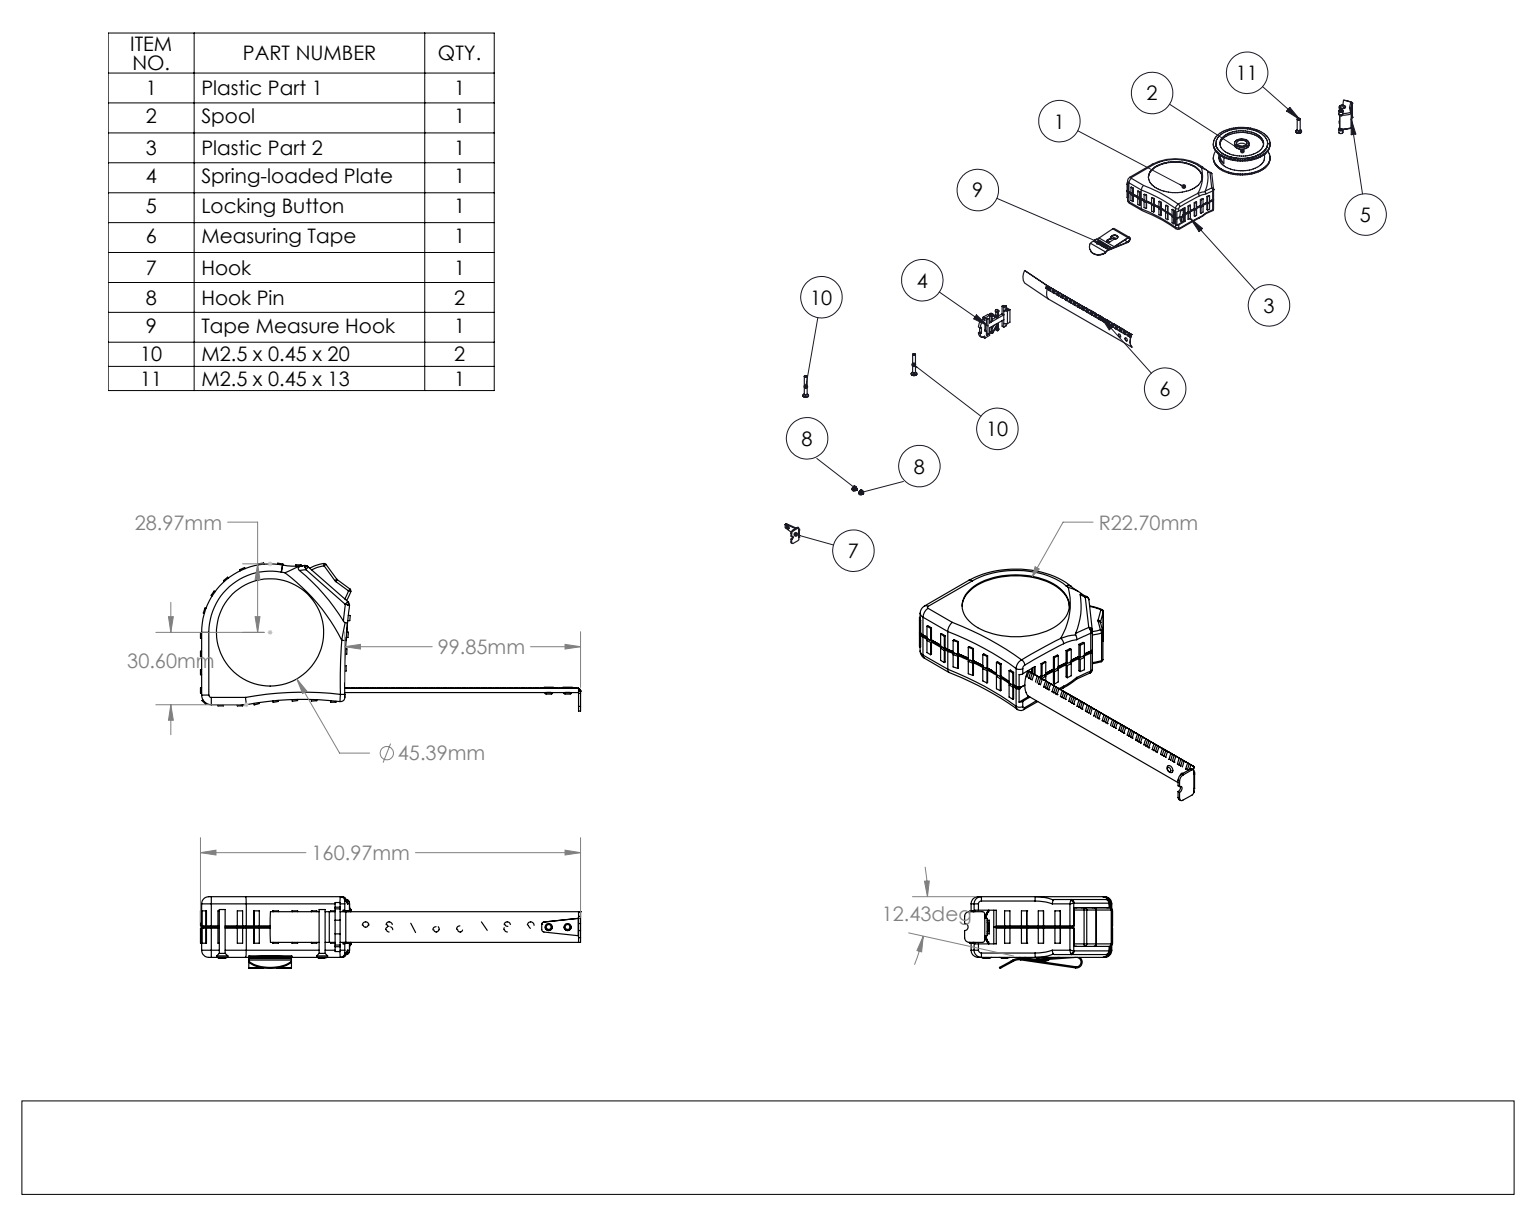
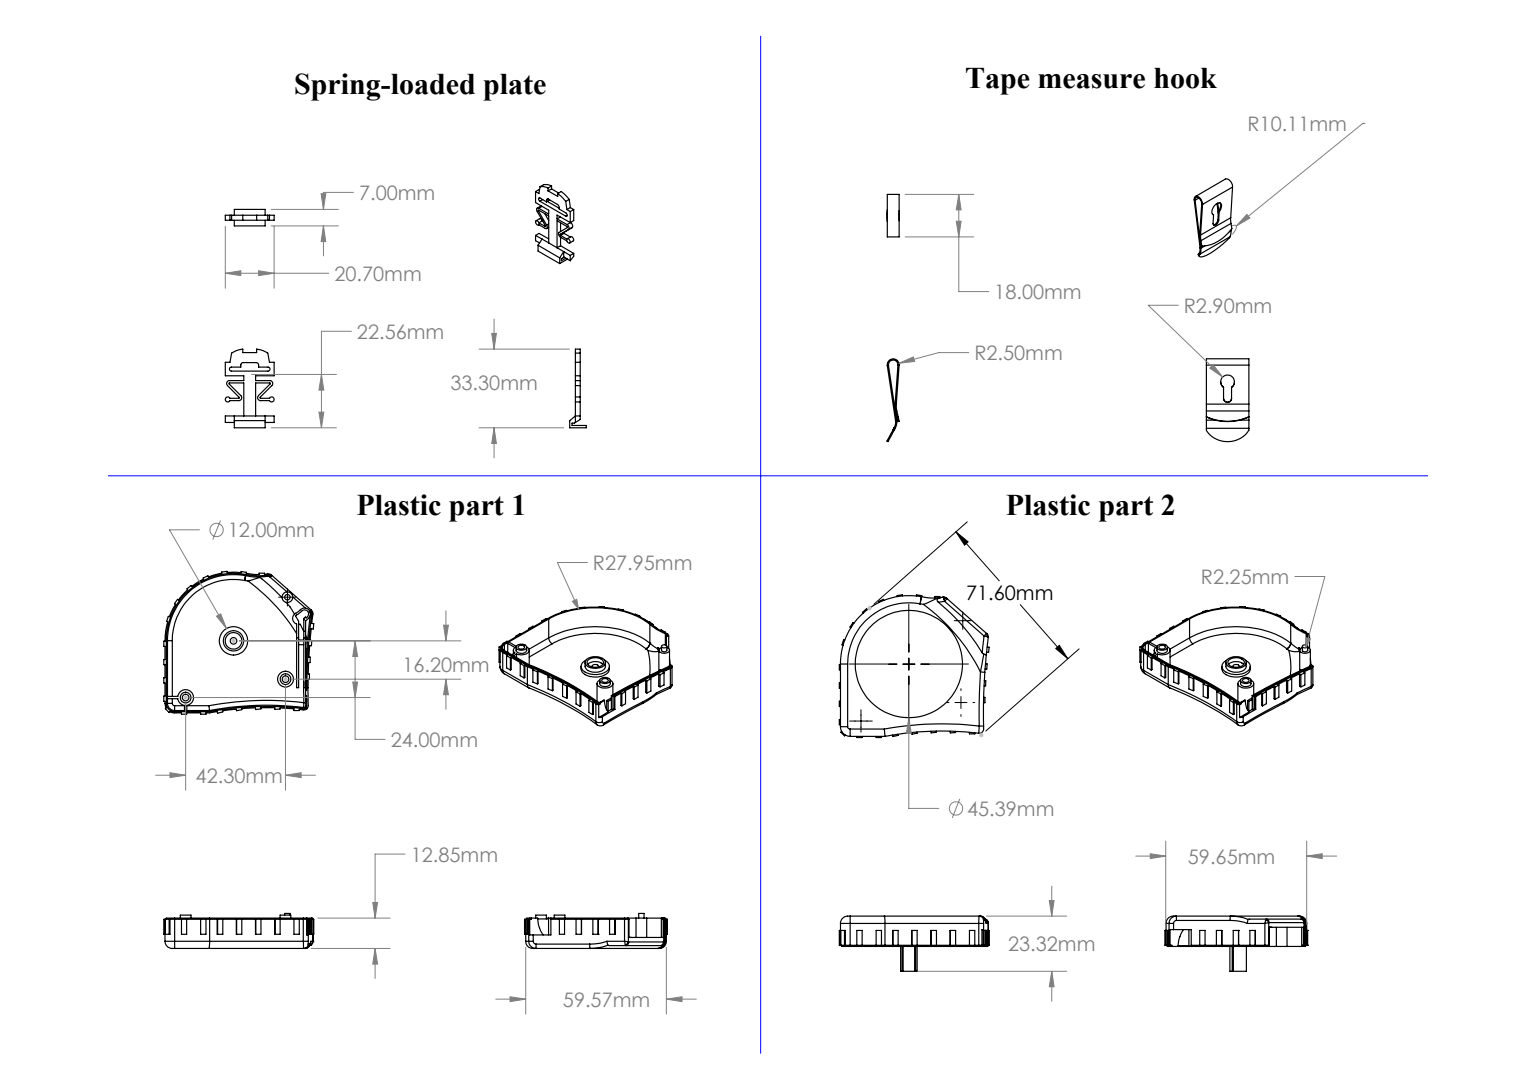
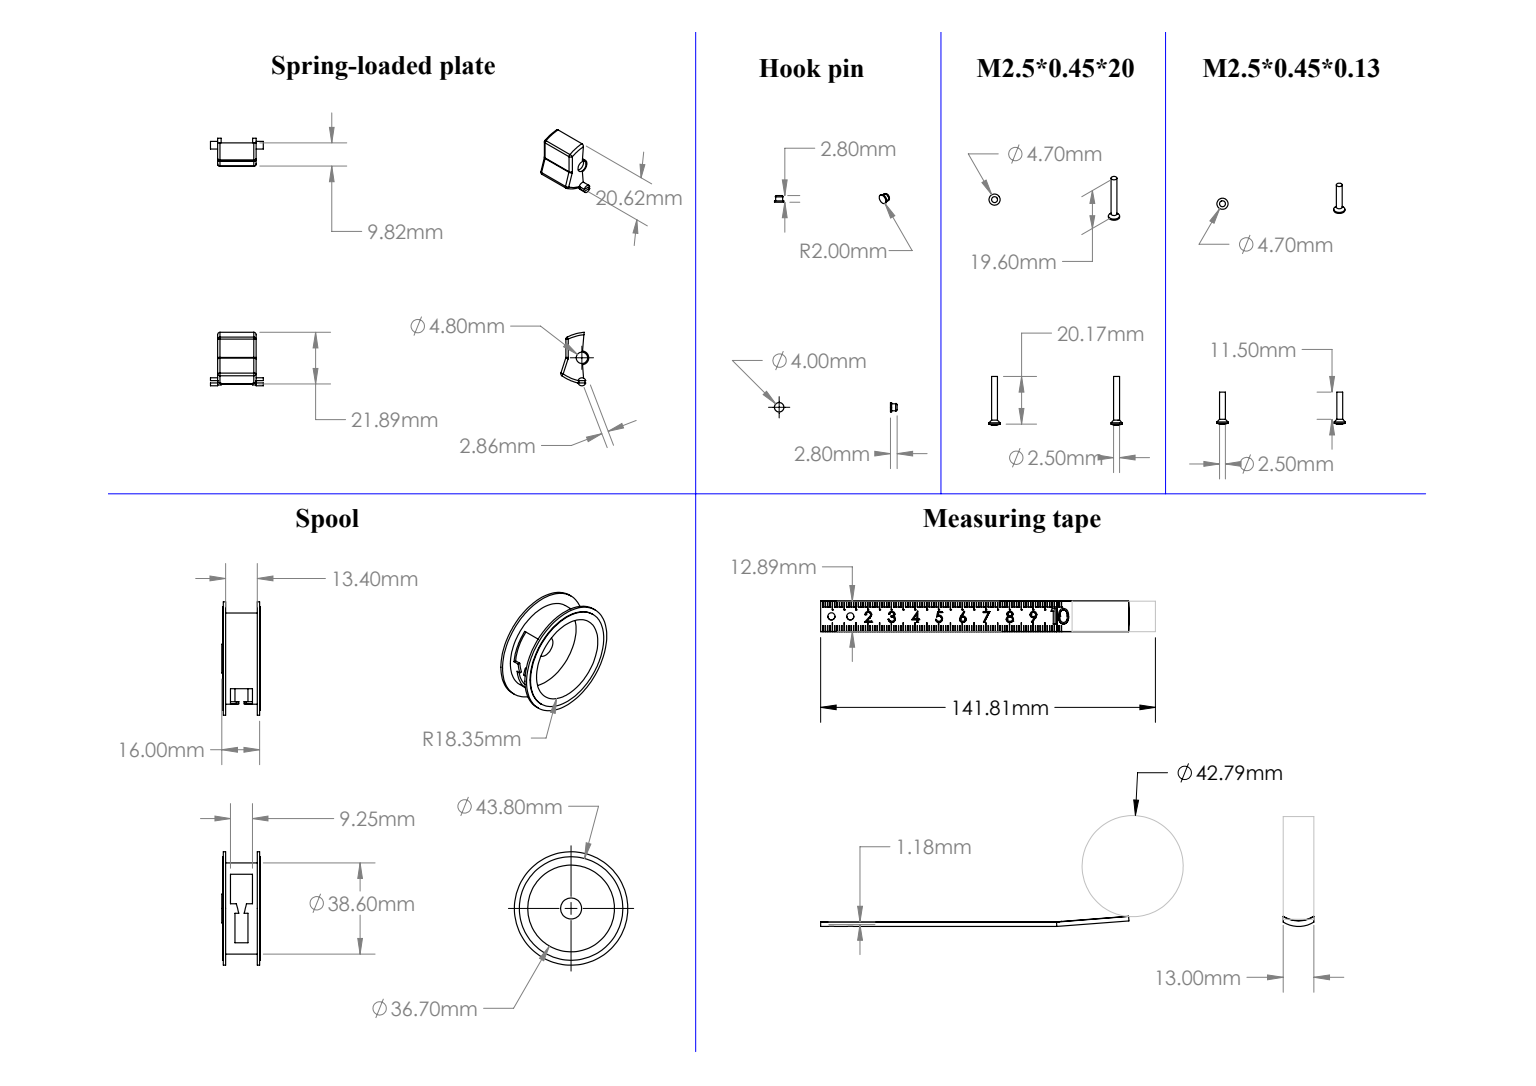
ISO-10303-21;
HEADER;
FILE_DESCRIPTION (('STEP AP203'),
    '1' );
FILE_NAME ('MAS-154',
    '2026-10-08T23:54:15',
    ( '' ),
    ( '' ),
    'SwSTEP 2.0',
    'SolidWorks 2024',
    '' );
FILE_SCHEMA (( 'AUTOMOTIVE_DESIGN' ));
ENDSEC;

DATA;
#1 = EDGE_LOOP ( 'NONE', ( #69285, #69519, #6373, #20333 ) ) ;
#2 = VECTOR ( 'NONE', #18887, 1000.000000000000000 ) ;
#3 = CARTESIAN_POINT ( 'NONE',  ( -28.32169924589829080, 0.3587747205143964613, -8.244178532169451401 ) ) ;
#4 = CARTESIAN_POINT ( 'NONE',  ( -80.94237186737068157, -25.14918324602283661, 7.008237357988867267 ) ) ;
#5 = EDGE_CURVE ( 'NONE', #2549, #11314, #80925, .T. ) ;
#6 = AXIS2_PLACEMENT_3D ( 'NONE', #5128, #50815, #66059 ) ;
#7 = CARTESIAN_POINT ( 'NONE',  ( -51.65200394065919909, -23.73791477778912196, 11.05961554403170766 ) ) ;
#9 = ORIENTED_EDGE ( 'NONE', *, *, #75672, .F. ) ;
#8 = CARTESIAN_POINT ( 'NONE',  ( 6.361473516681357410, -20.28576754457002451, 11.49999999999999645 ) ) ;
#10 = AXIS2_PLACEMENT_3D ( 'NONE', #33191, #48429, #34700 ) ;
#11 = EDGE_LOOP ( 'NONE', ( #61947, #2008, #96501, #28835 ) ) ;
#12 = CARTESIAN_POINT ( 'NONE',  ( -5.848988146064017180, 21.40304369876291446, 11.49999999999998934 ) ) ;
#13 = CARTESIAN_POINT ( 'NONE',  ( -4.704028875484805639, -20.06825252194306941, 11.49999999999998934 ) ) ;
#15 = ORIENTED_EDGE ( 'NONE', *, *, #21720, .F. ) ;
#14 = VECTOR ( 'NONE', #49997, 1000.000000000000000 ) ;
#16 = ORIENTED_EDGE ( 'NONE', *, *, #57693, .T. ) ;
#17 = DIRECTION ( 'NONE',  ( 1.000000000000000000, 3.773278334444166432E-23, 8.201307841325785021E-29 ) ) ;
#18 = CARTESIAN_POINT ( 'NONE',  ( -39.73355216781377663, -25.15155473006780795, 3.010709736661470348 ) ) ;
#19 = ORIENTED_EDGE ( 'NONE', *, *, #7474, .F. ) ;
#20 = CARTESIAN_POINT ( 'NONE',  ( -91.51201375565671015, -24.15543982623907482, -0.2315651400026614848 ) ) ;
#21 = VERTEX_POINT ( 'NONE', #59747 ) ;
#22 = CARTESIAN_POINT ( 'NONE',  ( -121.6228709571500559, -23.47596703998600631, 11.44779298504227683 ) ) ;
#23 = CARTESIAN_POINT ( 'NONE',  ( -44.52287095715004739, -23.94994826722564696, -0.6494450866342734718 ) ) ;
#24 = CARTESIAN_POINT ( 'NONE',  ( 9.770152518076534065, 18.40777400073588410, -1.500000000000002220 ) ) ;
#25 = CARTESIAN_POINT ( 'NONE',  ( 21.67628855941699939, -2.339797445609365756, 11.49999999999999645 ) ) ;
#26 = CARTESIAN_POINT ( 'NONE',  ( 25.13610348050010757, -5.148720480136078415, -8.780752235156151997 ) ) ;
#27 = LINE ( 'NONE', #61937, #7762 ) ;
#28 = CARTESIAN_POINT ( 'NONE',  ( 1.786768808452938950, -22.39398889530128756, -1.500000000000002220 ) ) ;
#29 = CARTESIAN_POINT ( 'NONE',  ( -118.5885948168727850, -24.51419770103160189, 9.386484678747168076 ) ) ;
#30 = ORIENTED_EDGE ( 'NONE', *, *, #89645, .T. ) ;
#31 = CARTESIAN_POINT ( 'NONE',  ( -4.993225604111834137, 0.3587747205143964613, -29.11654937215279304 ) ) ;
#32 = CARTESIAN_POINT ( 'NONE',  ( -51.15979583992254476, -25.14713903054791189, 3.043340899898625551 ) ) ;
#33 = EDGE_LOOP ( 'NONE', ( #82636, #82631 ) ) ;
#34 = ORIENTED_EDGE ( 'NONE', *, *, #61187, .T. ) ;
#35 = ORIENTED_EDGE ( 'NONE', *, *, #13828, .T. ) ;
#36 = B_SPLINE_CURVE_WITH_KNOTS ( 'NONE', 3,
 ( #15893, #77778, #86413, #8288 ),
 .UNSPECIFIED., .F., .F.,
 ( 4, 4 ),
 ( 0.000000000000000000, 1.000000000000000000 ),
 .UNSPECIFIED. ) ;
#37 = EDGE_CURVE ( 'NONE', #33217, #73517, #53079, .T. ) ;
#38 = CARTESIAN_POINT ( 'NONE',  ( -21.27170209485220198, -2.091907790468015005, -1.500000000000002220 ) ) ;
#39 = ORIENTED_EDGE ( 'NONE', *, *, #46353, .T. ) ;
#40 = CARTESIAN_POINT ( 'NONE',  ( -19.40065202112720755, 8.109199488025859992, -1.500000000000002220 ) ) ;
#41 = CARTESIAN_POINT ( 'NONE',  ( 8.376690734369038438, 12.50000000000004974, 2.100000000000000089 ) ) ;
#42 = CARTESIAN_POINT ( 'NONE',  ( -110.8023840715768671, -25.20836527976632624, 3.390575860289634313 ) ) ;
#43 = CARTESIAN_POINT ( 'NONE',  ( -49.64804092875103692, -25.07480650350090556, 7.411405559915849928 ) ) ;
#44 = CARTESIAN_POINT ( 'NONE',  ( 21.11370014442628218, -6.196533921283487345, -1.500000000000002220 ) ) ;
#45 = CARTESIAN_POINT ( 'NONE',  ( -52.62287095715006302, -23.94994826722515668, -0.6494450866351718643 ) ) ;
#46 = ORIENTED_EDGE ( 'NONE', *, *, #67580, .T. ) ;
#47 = DIRECTION ( 'NONE',  ( 0.000000000000000000, 1.000000000000000000, 0.000000000000000000 ) ) ;
#48 = B_SPLINE_CURVE_WITH_KNOTS ( 'NONE', 3,
 ( #59465, #45731, #6661, #91892, #14263, #52846 ),
 .UNSPECIFIED., .F., .F.,
 ( 4, 2, 4 ),
 ( 6.384118695835943749E-06, 0.001386860460836991790, 0.002767336802978147530 ),
 .UNSPECIFIED. ) ;
#49 = EDGE_CURVE ( 'NONE', #39472, #30477, #6341, .T. ) ;
#50 = FACE_OUTER_BOUND ( 'NONE', #1014, .T. ) ;
#51 = CARTESIAN_POINT ( 'NONE',  ( 2.550444227103870531, -20.70361394434535285, 11.49999999999999645 ) ) ;
#52 = EDGE_CURVE ( 'NONE', #64249, #62056, #30271, .T. ) ;
#53 = ADVANCED_FACE ( 'NONE', ( #51630 ), #45520, .T. ) ;
#54 = CYLINDRICAL_SURFACE ( 'NONE', #70588, 1.499999999999999556 ) ;
#55 = CARTESIAN_POINT ( 'NONE',  ( 0.000000000000000000, -4.056774720514426669, 0.000000000000000000 ) ) ;
#56 = ADVANCED_FACE ( 'NONE', ( #60747 ), #53135, .F. ) ;
#57 = CARTESIAN_POINT ( 'NONE',  ( -0.07181233839971890021, -22.12033284636826025, 9.440663514584143101 ) ) ;
#58 = CARTESIAN_POINT ( 'NONE',  ( 6.557060941508195739, 20.25493142521265355, 11.49999999999998934 ) ) ;
#59 = CARTESIAN_POINT ( 'NONE',  ( -31.24388727629349916, -25.30630219089158928, 5.533642405256624208 ) ) ;
#60 = CARTESIAN_POINT ( 'NONE',  ( -107.6235340483385130, -24.66019654487200441, 8.947790411086112172 ) ) ;
#61 = AXIS2_PLACEMENT_3D ( 'NONE', #34218, #56566, #41326 ) ;
#62 = CARTESIAN_POINT ( 'NONE',  ( -29.55620429048338949, -23.39166825546095296, 11.44779303307417706 ) ) ;
#63 = DIRECTION ( 'NONE',  ( -0.9762960071199348056, -0.2164396139380966033, -0.000000000000000000 ) ) ;
#64 = CARTESIAN_POINT ( 'NONE',  ( -19.74168752133572724, 10.86179948771369297, -1.500000000000002220 ) ) ;
#65 = CARTESIAN_POINT ( 'NONE',  ( -121.6228709571500417, -29.50250786944525672, 11.44777988621622811 ) ) ;
#66 = ORIENTED_EDGE ( 'NONE', *, *, #66534, .T. ) ;
#67 = DIRECTION ( 'NONE',  ( 0.000000000000000000, -0.000000000000000000, -1.000000000000000000 ) ) ;
#68 = CARTESIAN_POINT ( 'NONE',  ( 12.01011565470214393, -15.49198969801113890, 11.49999999999999645 ) ) ;
#69 = DIRECTION ( 'NONE',  ( -3.773278334453079030E-23, 0.9999999999976377785, 2.173523156925979128E-06 ) ) ;
#70 = CARTESIAN_POINT ( 'NONE',  ( 14.43441819135929194, -3.316774720514426456, -28.36222020317710957 ) ) ;
#71 = ADVANCED_FACE ( 'NONE', ( #37402 ), #6941, .F. ) ;
#72 = ORIENTED_EDGE ( 'NONE', *, *, #32563, .F. ) ;
#73 = CARTESIAN_POINT ( 'NONE',  ( -88.59478516332772813, -23.96169478059713853, 10.65365249895717703 ) ) ;
#74 = CARTESIAN_POINT ( 'NONE',  ( -124.7734663299911091, -25.37177631213229390, 5.922859790593148155 ) ) ;
#75 = FACE_OUTER_BOUND ( 'NONE', #16920, .T. ) ;
#77 = ADVANCED_FACE ( 'NONE', ( #5939 ), #75439, .F. ) ;
#76 = CARTESIAN_POINT ( 'NONE',  ( 19.18382676146983457, -4.683391092530263755, 11.49999999999998934 ) ) ;
#78 = B_SPLINE_CURVE_WITH_KNOTS ( 'NONE', 3,
 ( #65257, #57627, #41392, #64254 ),
 .UNSPECIFIED., .F., .F.,
 ( 4, 4 ),
 ( 0.2289244050901574346, 0.2299251521309229884 ),
 .UNSPECIFIED. ) ;
#79 = AXIS2_PLACEMENT_3D ( 'NONE', #87672, #18153, #64361 ) ;
#80 = VERTEX_POINT ( 'NONE', #68847 ) ;
#81 = CIRCLE ( 'NONE', #97288, 2.000000000000001776 ) ;
#82 = CARTESIAN_POINT ( 'NONE',  ( -109.4089209358690056, -25.26578872481861993, 3.901360433916359671 ) ) ;
#83 = ADVANCED_FACE ( 'NONE', ( #38389 ), #14547, .F. ) ;
#84 = VECTOR ( 'NONE', #37121, 1000.000000000000114 ) ;
#85 = SHAPE_DEFINITION_REPRESENTATION ( #13430, #26923 ) ;
#86 = VERTEX_POINT ( 'NONE', #90184 ) ;
#87 = CARTESIAN_POINT ( 'NONE',  ( -8.160000000000000142, -9.652339641703484574, -1.621096496867199033 ) ) ;
#88 = CARTESIAN_POINT ( 'NONE',  ( 30.93860345374796594, 0.6647747205144265426, 28.83647319851474933 ) ) ;
#89 = CARTESIAN_POINT ( 'NONE',  ( -41.52287095715006870, -23.47596703998600631, 11.44779298504229281 ) ) ;
#90 = CARTESIAN_POINT ( 'NONE',  ( -66.52287095715006160, -24.64898659630528854, 1.056161002820824368 ) ) ;
#91 = CARTESIAN_POINT ( 'NONE',  ( -1.836964591723098117, -5.876774720514410966, 19.23384392940399223 ) ) ;
#92 = CYLINDRICAL_SURFACE ( 'NONE', #60343, 8.452410033082761842 ) ;
#93 = CARTESIAN_POINT ( 'NONE',  ( -61.52287095715008292, -24.51283580621364777, 0.6167428607019722619 ) ) ;
#94 = CARTESIAN_POINT ( 'NONE',  ( -19.26508835251014773, 5.270845654819066084, 11.49999999999998934 ) ) ;
#95 = EDGE_CURVE ( 'NONE', #59480, #61101, #43375, .T. ) ;
#96 = CARTESIAN_POINT ( 'NONE',  ( -65.52287095715006160, -23.47596703998600631, 11.44779298504228748 ) ) ;
#97 = CARTESIAN_POINT ( 'NONE',  ( -45.58890605949096653, -24.52399227489127043, 9.353111116836528183 ) ) ;
#98 = ORIENTED_EDGE ( 'NONE', *, *, #94745, .T. ) ;
#99 = EDGE_CURVE ( 'NONE', #55720, #33243, #52622, .T. ) ;
#100 = EDGE_CURVE ( 'NONE', #61817, #96286, #13544, .T. ) ;
#101 = CARTESIAN_POINT ( 'NONE',  ( -104.6228709571500133, -23.96177878511308634, 10.65340807706329684 ) ) ;
#102 = CARTESIAN_POINT ( 'NONE',  ( -109.5174377349821953, -25.29012814469902182, 3.703579023877377807 ) ) ;
#103 = CARTESIAN_POINT ( 'NONE',  ( -35.52193570048709148, -23.48783264082477729, -1.443836473390077479 ) ) ;
#104 = CARTESIAN_POINT ( 'NONE',  ( -61.62287095715004881, -29.50247984919015209, -1.443849546365056913 ) ) ;
#105 = CARTESIAN_POINT ( 'NONE',  ( 8.971512145086506962, -2.028487854913504140, -5.500000000000000000 ) ) ;
#106 = CARTESIAN_POINT ( 'NONE',  ( 0.000000000000000000, -6.376774720514426953, 0.000000000000000000 ) ) ;
#107 = CARTESIAN_POINT ( 'NONE',  ( -63.62287095715004881, -23.48786465467241058, 11.44779295918254824 ) ) ;
#108 = LINE ( 'NONE', #99052, #42049 ) ;
#109 = ORIENTED_EDGE ( 'NONE', *, *, #9060, .T. ) ;
#110 = CARTESIAN_POINT ( 'NONE',  ( -6.888417027594036846, 19.07602104198033643, 11.49999999999998934 ) ) ;
#111 = B_SPLINE_CURVE_WITH_KNOTS ( 'NONE', 3,
 ( #12004, #4406, #74405, #5887 ),
 .UNSPECIFIED., .F., .F.,
 ( 4, 4 ),
 ( 0.5701930854029353402, 0.5791995166750508739 ),
 .UNSPECIFIED. ) ;
#112 = CARTESIAN_POINT ( 'NONE',  ( -8.978253834636468866, -6.376774720514426953, 0.000000000000000000 ) ) ;
#113 = DIRECTION ( 'NONE',  ( -3.773278334453080206E-23, 0.9999999999976377785, 2.173523156925979975E-06 ) ) ;
#114 = EDGE_LOOP ( 'NONE', ( #28040, #100187, #84080, #84178 ) ) ;
#115 = DIRECTION ( 'NONE',  ( 0.9940716917543757081, 0.000000000000000000, -0.1087265912856348327 ) ) ;
#116 = CARTESIAN_POINT ( 'NONE',  ( 17.11712468798820908, 10.61635618877791742, -1.500000000000002220 ) ) ;
#117 = CARTESIAN_POINT ( 'NONE',  ( -19.68365937621761219, -7.520201837432793468, 11.49999999999999645 ) ) ;
#118 = CARTESIAN_POINT ( 'NONE',  ( -16.97254739485517661, -14.18817111035334655, 11.49999999999998934 ) ) ;
#119 = CIRCLE ( 'NONE', #69815, 6.000000000000000888 ) ;
#120 = CARTESIAN_POINT ( 'NONE',  ( -17.34406541665444124, 10.97931167347951842, -1.500000000000002220 ) ) ;
#121 = CARTESIAN_POINT ( 'NONE',  ( -95.51720277341769361, -23.85016227208581441, -0.8807180028928280890 ) ) ;
#122 = CARTESIAN_POINT ( 'NONE',  ( 14.83405752585718496, 4.881907540129191148, -27.54622755360254516 ) ) ;
#123 = ORIENTED_EDGE ( 'NONE', *, *, #75034, .F. ) ;
#124 = CARTESIAN_POINT ( 'NONE',  ( -32.62287095715004881, -23.47593901973091235, -1.443836447539013301 ) ) ;
#125 = VERTEX_POINT ( 'NONE', #61249 ) ;
#126 = DIRECTION ( 'NONE',  ( 0.000000000000000000, 0.000000000000000000, 1.000000000000000000 ) ) ;
#127 = DIRECTION ( 'NONE',  ( -3.773278334453079618E-23, 0.9999999999976377785, 2.173523156925979975E-06 ) ) ;
#128 = ORIENTED_EDGE ( 'NONE', *, *, #60112, .T. ) ;
#129 = EDGE_LOOP ( 'NONE', ( #2287, #83763, #40797, #42125 ) ) ;
#130 = ORIENTED_EDGE ( 'NONE', *, *, #14486, .T. ) ;
#131 = LINE ( 'NONE', #46818, #56738 ) ;
#132 = CARTESIAN_POINT ( 'NONE',  ( -71.62287095715005592, -23.72773821059536559, 11.05748984161097681 ) ) ;
#133 = CARTESIAN_POINT ( 'NONE',  ( -68.53707658420209725, -24.66019654487199375, 8.947790411086122830 ) ) ;
#134 = CARTESIAN_POINT ( 'NONE',  ( 13.18972694569024640, 15.87703813876158598, -1.500000000000002220 ) ) ;
#135 = CARTESIAN_POINT ( 'NONE',  ( 1.064956243273112557, 21.61254047163424019, 11.49999999999999645 ) ) ;
#136 = ORIENTED_EDGE ( 'NONE', *, *, #10032, .F. ) ;
#137 = CARTESIAN_POINT ( 'NONE',  ( -83.62287095715005592, -24.64898659630528854, 1.056161002820826145 ) ) ;
#138 = CARTESIAN_POINT ( 'NONE',  ( 33.74607884027702909, -5.965225279485572685, -4.999864028243830916 ) ) ;
#139 = CARTESIAN_POINT ( 'NONE',  ( 1.438201247614206757, 22.34484416265529916, 11.49999999999998934 ) ) ;
#140 = DIRECTION ( 'NONE',  ( -1.000000000000000000, -3.773278334444167608E-23, -8.201307833595939069E-29 ) ) ;
#141 = DIRECTION ( 'NONE',  ( 0.000000000000000000, -2.173523156925979552E-06, 0.9999999999976378895 ) ) ;
#142 = ORIENTED_EDGE ( 'NONE', *, *, #69534, .F. ) ;
#143 = CARTESIAN_POINT ( 'NONE',  ( 32.98210467718394767, -3.587965230352024193, -12.99284425914657604 ) ) ;
#144 = CARTESIAN_POINT ( 'NONE',  ( -49.59335215026359833, -24.15620529776627379, 10.23563542870661003 ) ) ;
#145 = B_SPLINE_CURVE_WITH_KNOTS ( 'NONE', 3,
 ( #93012, #31119, #8793, #23489, #70690, #39734 ),
 .UNSPECIFIED., .F., .F.,
 ( 4, 2, 4 ),
 ( 0.000000000000000000, 0.001380764517853254455, 0.002761529035706508910 ),
 .UNSPECIFIED. ) ;
#146 = VECTOR ( 'NONE', #42347, 1000.000000000000114 ) ;
#147 = DIRECTION ( 'NONE',  ( 0.6599726524652350657, 0.000000000000000000, -0.7512896232465892110 ) ) ;
#148 = CARTESIAN_POINT ( 'NONE',  ( -15.06743543786183714, 14.52697759824333090, -1.500000000000002220 ) ) ;
#149 = VERTEX_POINT ( 'NONE', #67859 ) ;
#150 = B_SPLINE_CURVE_WITH_KNOTS ( 'NONE', 3,
 ( #38455, #85628, #62820, #87130 ),
 .UNSPECIFIED., .F., .F.,
 ( 4, 4 ),
 ( 2.775557561562891351E-17, 0.0001000000000000167286 ),
 .UNSPECIFIED. ) ;
#151 = B_SPLINE_CURVE_WITH_KNOTS ( 'NONE', 3,
 ( #689, #31133, #14407, #23004, #54988, #7294 ),
 .UNSPECIFIED., .F., .F.,
 ( 4, 2, 4 ),
 ( 3.593123586040311387E-14, 0.0002343744485612567175, 0.0004687488970865821619 ),
 .UNSPECIFIED. ) ;
#152 = CARTESIAN_POINT ( 'NONE',  ( -69.62287095715005592, -29.50248528299804818, 1.056150453629036701 ) ) ;
#153 = VERTEX_POINT ( 'NONE', #84561 ) ;
#154 = CARTESIAN_POINT ( 'NONE',  ( -109.6330811136520111, -23.48786465467241769, 11.44779295918253759 ) ) ;
#155 = CARTESIAN_POINT ( 'NONE',  ( 1.812468502196824760, -21.08352789287561180, -1.500000000000002220 ) ) ;
#156 = EDGE_LOOP ( 'NONE', ( #85113, #7630, #40085, #37423 ) ) ;
#157 = CARTESIAN_POINT ( 'NONE',  ( -50.65003834120983583, -24.15503026093913164, -0.2815557561904566963 ) ) ;
#158 = EDGE_CURVE ( 'NONE', #46090, #80749, #42232, .T. ) ;
#159 = CARTESIAN_POINT ( 'NONE',  ( 14.98227958311676744, 15.82868232077399462, 11.49999999999998934 ) ) ;
#160 = CARTESIAN_POINT ( 'NONE',  ( -7.586742644780859912, -6.376774720514413630, 19.78730719034165020 ) ) ;
#161 = ADVANCED_FACE ( 'NONE', ( #15045 ), #7938, .F. ) ;
#162 = LINE ( 'NONE', #7772, #59931 ) ;
#163 = CARTESIAN_POINT ( 'NONE',  ( -79.62287095715005592, -23.47593901973091235, -1.443836447539004642 ) ) ;
#164 = CARTESIAN_POINT ( 'NONE',  ( 14.98227958311676744, 15.82868232077399462, -1.500000000000002220 ) ) ;
#165 = CARTESIAN_POINT ( 'NONE',  ( -66.92287095715006728, -23.47593901973090169, -1.443836447538997536 ) ) ;
#166 = ORIENTED_EDGE ( 'NONE', *, *, #99366, .F. ) ;
#167 = CARTESIAN_POINT ( 'NONE',  ( 7.479587785762670471, -5.876774720514418071, 20.73799387832858088 ) ) ;
#168 = DIRECTION ( 'NONE',  ( 0.000000000000000000, -1.000000000000000000, 0.000000000000000000 ) ) ;
#169 = ORIENTED_EDGE ( 'NONE', *, *, #41304, .T. ) ;
#170 = EDGE_CURVE ( 'NONE', #72067, #41555, #93164, .T. ) ;
#171 = EDGE_CURVE ( 'NONE', #82004, #10266, #15546, .T. ) ;
#172 = ORIENTED_EDGE ( 'NONE', *, *, #47372, .F. ) ;
#173 = EDGE_CURVE ( 'NONE', #72214, #47216, #85698, .T. ) ;
#174 = EDGE_LOOP ( 'NONE', ( #58420, #72344, #98648 ) ) ;
#175 = DIRECTION ( 'NONE',  ( -1.000000000000000000, -3.773278334444166432E-23, -8.201307841325785021E-29 ) ) ;
#176 = CARTESIAN_POINT ( 'NONE',  ( -10.24059822343752479, -5.876774720514426953, -2.394817856121274864E-14 ) ) ;
#177 = CARTESIAN_POINT ( 'NONE',  ( 4.903939382885006637, -20.63555827282145572, 11.49999999999998934 ) ) ;
#178 = CARTESIAN_POINT ( 'NONE',  ( -80.35919894935766195, -25.30543142107805465, 4.505481316334992492 ) ) ;
#179 = CARTESIAN_POINT ( 'NONE',  ( -79.38827465850120291, -25.03138204137674805, 7.124171970841336687 ) ) ;
#180 = CARTESIAN_POINT ( 'NONE',  ( 30.77564450787170003, 1.477225279485574028, -9.689394075852829857 ) ) ;
#181 = CARTESIAN_POINT ( 'NONE',  ( 32.95642386911166710, 3.601225610321291182, -13.01540364303327380 ) ) ;
#182 = CARTESIAN_POINT ( 'NONE',  ( -4.359330469889163950, 18.88329184224734192, 11.49999999999998934 ) ) ;
#183 = CARTESIAN_POINT ( 'NONE',  ( -39.97931365918082491, -25.30060000302003331, 6.009290021095885059 ) ) ;
#184 = ORIENTED_EDGE ( 'NONE', *, *, #85046, .F. ) ;
#185 = CARTESIAN_POINT ( 'NONE',  ( -14.34788840963776124, 13.16932220997287928, 11.49999999999999645 ) ) ;
#186 = LINE ( 'NONE', #37749, #11453 ) ;
#187 = CARTESIAN_POINT ( 'NONE',  ( 1.305682803664691249, -5.965225279485572685, 29.57950906855421991 ) ) ;
#188 = ADVANCED_FACE ( 'NONE', ( #94676 ), #86066, .T. ) ;
#189 = ORIENTED_EDGE ( 'NONE', *, *, #66768, .T. ) ;
#190 = CARTESIAN_POINT ( 'NONE',  ( 3.475076759263674209, -5.876774720514402084, 18.20843037655054530 ) ) ;
#191 = CARTESIAN_POINT ( 'NONE',  ( 16.26279755680690542, -6.475225279485573360, -27.67997040356620531 ) ) ;
#192 = CARTESIAN_POINT ( 'NONE',  ( -64.62287095715005592, -23.47593901973091235, -1.443836447539007972 ) ) ;
#193 = CARTESIAN_POINT ( 'NONE',  ( -101.2856530191658919, -25.24578106541012446, 3.795013565542035838 ) ) ;
#195 = ADVANCED_FACE ( 'NONE', ( #77436 ), #54627, .F. ) ;
#194 = CARTESIAN_POINT ( 'NONE',  ( -18.74126595726828626, 5.813943427813767606, 11.49999999999998934 ) ) ;
#196 = FACE_OUTER_BOUND ( 'NONE', #11738, .T. ) ;
#197 = ORIENTED_EDGE ( 'NONE', *, *, #96086, .T. ) ;
#198 = CARTESIAN_POINT ( 'NONE',  ( -19.30636564405121902, 9.640216152154000184, -1.500000000000002220 ) ) ;
#199 = DIRECTION ( 'NONE',  ( 0.000000000000000000, 0.000000000000000000, 1.000000000000000000 ) ) ;
#200 = DIRECTION ( 'NONE',  ( 0.000000000000000000, 0.000000000000000000, 1.000000000000000000 ) ) ;
#201 = VECTOR ( 'NONE', #49390, 1000.000000000000000 ) ;
#202 = LINE ( 'NONE', #46883, #26152 ) ;
#203 = CARTESIAN_POINT ( 'NONE',  ( -13.16640216892762894, -18.94680327863774849, -1.500000000000002220 ) ) ;
#204 = DATE_TIME_ROLE ( 'creation_date' ) ;
#205 = CARTESIAN_POINT ( 'NONE',  ( -93.51856585546278211, -23.73766607897670511, -1.055555164236453569 ) ) ;
#206 = CARTESIAN_POINT ( 'NONE',  ( 4.518955212990007908, -6.376774720514422512, 20.94857968174986951 ) ) ;
#207 = CARTESIAN_POINT ( 'NONE',  ( -113.5228709571500616, -29.50250786944525672, 11.44777988621622988 ) ) ;
#208 = LINE ( 'NONE', #38761, #30674 ) ;
#209 = CARTESIAN_POINT ( 'NONE',  ( -110.2723682709820565, -25.18516355925999406, 3.295595804301087117 ) ) ;
#210 = CARTESIAN_POINT ( 'NONE',  ( -73.52287095715004739, -23.96177878511308990, 10.65340807706330217 ) ) ;
#211 = CARTESIAN_POINT ( 'NONE',  ( -111.3738206124644279, -25.18425799667088327, 4.292346856177868375 ) ) ;
#212 = CARTESIAN_POINT ( 'NONE',  ( 18.06118663784855372, 8.336529998961283994, 11.49999999999998934 ) ) ;
#213 = DIRECTION ( 'NONE',  ( -0.000000000000000000, 1.000000000000000000, -0.000000000000000000 ) ) ;
#214 = CARTESIAN_POINT ( 'NONE',  ( 11.68167410197319001, -16.05257874518773065, -1.500000000000002220 ) ) ;
#215 = CARTESIAN_POINT ( 'NONE',  ( -0.4362980769230789257, -5.876774720514411854, 19.46153846153846345 ) ) ;
#216 = EDGE_CURVE ( 'NONE', #67134, #36357, #40895, .T. ) ;
#217 = VECTOR ( 'NONE', #39385, 1000.000000000000000 ) ;
#218 = AXIS2_PLACEMENT_3D ( 'NONE', #55658, #4225, #12317 ) ;
#219 = CARTESIAN_POINT ( 'NONE',  ( -56.62287095715005592, -29.50250243563736774, 8.947779886222145151 ) ) ;
#220 = CARTESIAN_POINT ( 'NONE',  ( 11.98973536156539943, -4.132774720514426292, -26.26140391504922178 ) ) ;
#221 = CARTESIAN_POINT ( 'NONE',  ( -10.81534556030752725, -17.66751395530895152, 11.49999999999999645 ) ) ;
#222 = DIRECTION ( 'NONE',  ( -0.000000000000000000, -1.000000000000000000, -0.000000000000000000 ) ) ;
#223 = ADVANCED_FACE ( 'NONE', ( #39891 ), #24162, .F. ) ;
#224 = LINE ( 'NONE', #31165, #81402 ) ;
#225 = CARTESIAN_POINT ( 'NONE',  ( 16.48639501038195121, -15.69157857782056276, 11.49999999999999645 ) ) ;
#226 = ORIENTED_EDGE ( 'NONE', *, *, #92027, .F. ) ;
#227 = CARTESIAN_POINT ( 'NONE',  ( -58.52287095715006160, -24.65952944569304250, 1.056160979905695463 ) ) ;
#228 = CARTESIAN_POINT ( 'NONE',  ( -106.6228709571500559, -24.64898659630368627, 1.056161002820831474 ) ) ;
#229 = B_SPLINE_CURVE_WITH_KNOTS ( 'NONE', 3,
 ( #25806, #12065, #89208, #96813 ),
 .UNSPECIFIED., .F., .F.,
 ( 4, 4 ),
 ( 0.000000000000000000, 0.0001000000000000028644 ),
 .UNSPECIFIED. ) ;
#230 = ORIENTED_EDGE ( 'NONE', *, *, #33610, .F. ) ;
#231 = CARTESIAN_POINT ( 'NONE',  ( 5.087728227403598424, 19.53446797131710611, 11.49999999999998934 ) ) ;
#232 = CARTESIAN_POINT ( 'NONE',  ( -108.6228709571500275, -24.33927499327853639, 9.819080762295818943 ) ) ;
#233 = DIRECTION ( 'NONE',  ( -3.773278334453080206E-23, 0.9999999999976377785, 2.173523156925979975E-06 ) ) ;
#234 = VERTEX_POINT ( 'NONE', #92668 ) ;
#235 = EDGE_LOOP ( 'NONE', ( #88022, #66563, #60750, #15385 ) ) ;
#236 = DIRECTION ( 'NONE',  ( 0.000000000000000000, 0.9999999999976377785, 2.173523156925979975E-06 ) ) ;
#237 = CARTESIAN_POINT ( 'NONE',  ( -19.55383134093860420, 11.88776249338449986, 11.49999999999998934 ) ) ;
#238 = CARTESIAN_POINT ( 'NONE',  ( -51.23509499458276650, -25.18439743769400252, 3.726222305450818784 ) ) ;
#239 = CARTESIAN_POINT ( 'NONE',  ( -20.67203406374276398, -6.343553224398504220, -1.500000000000002220 ) ) ;
#240 = DIRECTION ( 'NONE',  ( -0.000000000000000000, 1.000000000000000000, -0.000000000000000000 ) ) ;
#241 = CARTESIAN_POINT ( 'NONE',  ( 4.013313563623547964, -20.52093592976233438, 11.49999999999999645 ) ) ;
#242 = ORIENTED_EDGE ( 'NONE', *, *, #44768, .T. ) ;
#243 = CARTESIAN_POINT ( 'NONE',  ( -124.5206819125863262, -24.15543982623907482, -0.2315651400026562945 ) ) ;
#244 = CARTESIAN_POINT ( 'NONE',  ( -18.71521858236628333, -11.60751834597489740, 11.49999999999998934 ) ) ;
#245 = LINE ( 'NONE', #62665, #68980 ) ;
#246 = CARTESIAN_POINT ( 'NONE',  ( -30.47287095715008576, -24.05150381395742443, 10.46526688926917181 ) ) ;
#247 = ORIENTED_EDGE ( 'NONE', *, *, #73065, .T. ) ;
#248 = AXIS2_PLACEMENT_3D ( 'NONE', #29119, #5785, #36741 ) ;
#249 = CARTESIAN_POINT ( 'NONE',  ( 4.886128916861816052, -6.376774720514411854, 19.14085035285361514 ) ) ;
#250 = DIRECTION ( 'NONE',  ( -1.000000000000000000, 0.000000000000000000, 0.000000000000000000 ) ) ;
#251 = EDGE_LOOP ( 'NONE', ( #52195, #19336, #31483, #49094, #27965, #14246, #22960, #25333, #21362, #63679, #17102, #94843, #14089, #95653, #36853, #77118, #64971, #20831, #46153, #91222, #51880, #19595, #36808, #17745, #12211, #19237, #59711, #42959 ) ) ;
#252 = DIRECTION ( 'NONE',  ( -1.000000000000000000, -3.773278334444167608E-23, -8.201307833595939069E-29 ) ) ;
#253 = ORIENTED_EDGE ( 'NONE', *, *, #52923, .F. ) ;
#254 = ORIENTED_EDGE ( 'NONE', *, *, #68054, .T. ) ;
#255 = CARTESIAN_POINT ( 'NONE',  ( -61.64687923781918499, -25.15699314367416051, 3.101158825156976384 ) ) ;
#256 = CARTESIAN_POINT ( 'NONE',  ( -101.5300974081266787, -25.27404751924990123, 3.391562929131038295 ) ) ;
#257 = CARTESIAN_POINT ( 'NONE',  ( -36.47913385759269289, -24.65952944569304606, 1.056160979905694353 ) ) ;
#258 = CARTESIAN_POINT ( 'NONE',  ( 20.32696876622996029, 2.630761579057304900, -1.500000000000002220 ) ) ;
#259 = EDGE_LOOP ( 'NONE', ( #70483, #94459, #10754, #74894, #15740 ) ) ;
#260 = CARTESIAN_POINT ( 'NONE',  ( -99.47179591409185662, -25.28893848418214674, 5.641873549842387980 ) ) ;
#261 = CARTESIAN_POINT ( 'NONE',  ( -44.54012218498173326, -24.34968618360933590, 0.1864209137778786995 ) ) ;
#262 = FACE_OUTER_BOUND ( 'NONE', #1139, .T. ) ;
#263 = CARTESIAN_POINT ( 'NONE',  ( 20.12748746789148413, 9.599020362109589755, -1.500000000000002220 ) ) ;
#264 = PLANE ( 'NONE',  #88586 ) ;
#265 = CARTESIAN_POINT ( 'NONE',  ( -1.358974358974357921, -5.876774720514419847, 20.75510817307693046 ) ) ;
#266 = ORIENTED_EDGE ( 'NONE', *, *, #94468, .T. ) ;
#267 = B_SPLINE_CURVE_WITH_KNOTS ( 'NONE', 3,
 ( #48600, #903, #40970, #18128 ),
 .UNSPECIFIED., .F., .F.,
 ( 4, 4 ),
 ( 0.000000000000000000, 9.999999999998900014E-05 ),
 .UNSPECIFIED. ) ;
#268 = DIRECTION ( 'NONE',  ( 1.286817348990133655E-16, 0.000000000000000000, -1.000000000000000000 ) ) ;
#269 = CARTESIAN_POINT ( 'NONE',  ( -29.01900995608618317, -25.26247959377253238, 7.711473047842090978 ) ) ;
#270 = CARTESIAN_POINT ( 'NONE',  ( -11.07951500695464553, -17.62175104703424466, 11.49999999999998934 ) ) ;
#271 = CIRCLE ( 'NONE', #60197, 22.69500000000000384 ) ;
#272 = ORIENTED_EDGE ( 'NONE', *, *, #40497, .T. ) ;
#274 = EDGE_LOOP ( 'NONE', ( #98900, #37261, #35431, #93188 ) ) ;
#273 = CARTESIAN_POINT ( 'NONE',  ( -54.62287095715005592, -23.72747288104441665, -1.053458166803663776 ) ) ;
#275 = CARTESIAN_POINT ( 'NONE',  ( -51.52241826985714113, -25.12217690167820550, 6.308159032981181191 ) ) ;
#276 = CARTESIAN_POINT ( 'NONE',  ( -20.98013922110768448, -1.350454208470041273, -1.500000000000002220 ) ) ;
#277 = ORIENTED_EDGE ( 'NONE', *, *, #15628, .T. ) ;
#278 = CARTESIAN_POINT ( 'NONE',  ( -69.52287095715006160, -23.96177878511308634, 10.65340807706329862 ) ) ;
#280 = EDGE_CURVE ( 'NONE', #84354, #30802, #77932, .T. ) ;
#279 = LINE ( 'NONE', #14000, #91749 ) ;
#281 = CARTESIAN_POINT ( 'NONE',  ( 8.476323908314187250, -3.316774720514010788, -27.09030197646909599 ) ) ;
#282 = CARTESIAN_POINT ( 'NONE',  ( 30.53060340732036337, 1.682774720514426114, -1.352392034746782823 ) ) ;
#283 = CARTESIAN_POINT ( 'NONE',  ( -92.63100859344015703, -24.15620529776628445, 10.23563542870660292 ) ) ;
#284 = CARTESIAN_POINT ( 'NONE',  ( 19.24418710706453339, -0.5000000000000000000, -2.153101996372891236 ) ) ;
#286 = ORIENTED_EDGE ( 'NONE', *, *, #56606, .F. ) ;
#285 = CARTESIAN_POINT ( 'NONE',  ( 21.60277357391871433, -5.133695162202882578, 11.49999999999999645 ) ) ;
#287 = CARTESIAN_POINT ( 'NONE',  ( -3.212051231530180573, 17.72614232434105119, -9.000000000000000000 ) ) ;
#288 = CARTESIAN_POINT ( 'NONE',  ( 30.09341516180546350, 1.682774720514426114, -11.39311774897855756 ) ) ;
#289 = ORIENTED_EDGE ( 'NONE', *, *, #88515, .T. ) ;
#290 = EDGE_CURVE ( 'NONE', #36098, #73116, #17648, .T. ) ;
#291 = CARTESIAN_POINT ( 'NONE',  ( 20.84710439121840864, 8.857176948214046774, 11.49999999999998934 ) ) ;
#292 = ADVANCED_FACE ( 'NONE', ( #39393 ), #87066, .F. ) ;
#294 = VERTEX_POINT ( 'NONE', #62753 ) ;
#293 = CARTESIAN_POINT ( 'NONE',  ( -28.87481646230549615, -25.02372474006351410, 6.909395630504118202 ) ) ;
#295 = B_SPLINE_CURVE_WITH_KNOTS ( 'NONE', 3,
 ( #30244, #17024, #22619, #37869 ),
 .UNSPECIFIED., .F., .F.,
 ( 4, 4 ),
 ( 0.6892680438423023359, 0.6902687908830678065 ),
 .UNSPECIFIED. ) ;
#296 = VECTOR ( 'NONE', #83307, 1000.000000000000000 ) ;
#297 = EDGE_CURVE ( 'NONE', #11247, #80389, #48523, .T. ) ;
#298 = ORIENTED_EDGE ( 'NONE', *, *, #47645, .F. ) ;
#299 = LOCAL_TIME ( 0, 54, 15.00000000000000000, #26164 ) ;
#300 = EDGE_CURVE ( 'NONE', #37450, #64205, #96659, .T. ) ;
#301 = CARTESIAN_POINT ( 'NONE',  ( 32.06540688909005610, 6.475225279485576024, -12.44045471929206137 ) ) ;
#302 = CARTESIAN_POINT ( 'NONE',  ( -19.13055903301823335, -6.388282315271819556, -1.500000000000002220 ) ) ;
#303 = CARTESIAN_POINT ( 'NONE',  ( -81.62287095715004170, -24.66019654487199020, 8.947790411086131712 ) ) ;
#304 = ORIENTED_EDGE ( 'NONE', *, *, #22085, .F. ) ;
#305 = FACE_OUTER_BOUND ( 'NONE', #66048, .T. ) ;
#306 = CARTESIAN_POINT ( 'NONE',  ( -11.14805103425725719, -19.39388463112642214, -1.500000000000002220 ) ) ;
#307 = ORIENTED_EDGE ( 'NONE', *, *, #64377, .T. ) ;
#308 = ORIENTED_EDGE ( 'NONE', *, *, #56022, .T. ) ;
#309 = CARTESIAN_POINT ( 'NONE',  ( -101.3040450898205620, -25.16257414492327626, 6.746837491236538753 ) ) ;
#310 = DIRECTION ( 'NONE',  ( 3.773278334444166432E-23, -1.000000000000000000, 0.000000000000000000 ) ) ;
#311 = LINE ( 'NONE', #38370, #36067 ) ;
#312 = DIRECTION ( 'NONE',  ( -0.9994733861282923959, -0.000000000000000000, -0.03244919754393515293 ) ) ;
#313 = EDGE_CURVE ( 'NONE', #82268, #35739, #55515, .T. ) ;
#314 = CARTESIAN_POINT ( 'NONE',  ( -130.5728709571500588, -24.04615231314292245, -0.4716817114508914388 ) ) ;
#315 = CARTESIAN_POINT ( 'NONE',  ( -9.627943313441900131, 16.98966435471970726, 11.49999999999998934 ) ) ;
#316 = DIRECTION ( 'NONE',  ( 0.000000000000000000, 0.000000000000000000, -1.000000000000000000 ) ) ;
#317 = CARTESIAN_POINT ( 'NONE',  ( 17.49997855696484095, 12.48231381050728928, -1.500000000000002220 ) ) ;
#318 = CARTESIAN_POINT ( 'NONE',  ( -128.5901389850763508, -23.73766607897672287, -1.055555164236423149 ) ) ;
#319 = CARTESIAN_POINT ( 'NONE',  ( -121.5228709571500332, -23.73907113216989728, -1.053371485793244355 ) ) ;
#320 = LINE ( 'NONE', #47507, #53904 ) ;
#321 = CARTESIAN_POINT ( 'NONE',  ( -80.62287095715004170, -23.84081130438200802, 10.88220057463249546 ) ) ;
#322 = CARTESIAN_POINT ( 'NONE',  ( 4.181975289622855918, -22.47981636197143374, -1.500000000000002220 ) ) ;
#323 = VECTOR ( 'NONE', #80047, 1000.000000000000000 ) ;
#324 = COORDINATED_UNIVERSAL_TIME_OFFSET ( 0, 0, .AHEAD. ) ;
#325 = CARTESIAN_POINT ( 'NONE',  ( -96.59678146177949998, -23.73791477778911840, 11.05961554403170410 ) ) ;
#326 = CARTESIAN_POINT ( 'NONE',  ( -92.62287095715007013, -23.94994826722565762, -0.6494450866342730277 ) ) ;
#327 = CARTESIAN_POINT ( 'NONE',  ( -12.91570554291229023, -15.35452705144416896, 11.49999999999999645 ) ) ;
#328 = CARTESIAN_POINT ( 'NONE',  ( -79.92757955003747838, -25.31594328122231730, 4.561565462960619932 ) ) ;
#329 = CARTESIAN_POINT ( 'NONE',  ( -65.05438548721848235, 6.475225279485573360, 0.7300228001186309656 ) ) ;
#330 = DIRECTION ( 'NONE',  ( -0.000000000000000000, -0.000000000000000000, -1.000000000000000000 ) ) ;
#331 = CARTESIAN_POINT ( 'NONE',  ( -115.6228709571500559, -29.50248789122583659, 2.256150453626215580 ) ) ;
#332 = ORIENTED_EDGE ( 'NONE', *, *, #93875, .T. ) ;
#333 = CARTESIAN_POINT ( 'NONE',  ( -85.62287095715005592, -23.47593901973091235, -1.443836447539002865 ) ) ;
#334 = CARTESIAN_POINT ( 'NONE',  ( -109.9631709994365423, -25.11668225391187548, 2.867640993816269912 ) ) ;
#335 = CARTESIAN_POINT ( 'NONE',  ( -3.058130702743298901, -21.54894043062209263, 11.49999999999998934 ) ) ;
#336 = CARTESIAN_POINT ( 'NONE',  ( -45.52287095715009002, -24.52323809116982645, 9.355190652339423707 ) ) ;
#337 = CARTESIAN_POINT ( 'NONE',  ( -3.719764837209879271, -19.30396570740023421, -1.500000000000002220 ) ) ;
#338 = DIRECTION ( 'NONE',  ( 0.000000000000000000, -0.000000000000000000, -1.000000000000000000 ) ) ;
#339 = CARTESIAN_POINT ( 'NONE',  ( -97.52287095715006160, -29.50248528299804818, 1.056150453629042030 ) ) ;
#340 = CONTEXT_DEPENDENT_SHAPE_REPRESENTATION ( #56359, #40896 ) ;
#341 = CARTESIAN_POINT ( 'NONE',  ( -38.55620429048340014, -23.47596703998600276, 11.44779298504227505 ) ) ;
#342 = CARTESIAN_POINT ( 'NONE',  ( 2.708118538500707828, -6.376774720514424288, 20.94830092343283212 ) ) ;
#343 = CARTESIAN_POINT ( 'NONE',  ( -20.56140336115741718, 0.6910293267889283664, 11.49999999999999645 ) ) ;
#344 = CARTESIAN_POINT ( 'NONE',  ( 30.59073162224239084, 4.540774720514408891, 26.30400772315274338 ) ) ;
#345 = AXIS2_PLACEMENT_3D ( 'NONE', #4716, #83319, #98039 ) ;
#346 = CARTESIAN_POINT ( 'NONE',  ( -120.5530855258607659, -24.73486907724918638, 1.287355809206965684 ) ) ;
#347 = EDGE_LOOP ( 'NONE', ( #79694, #28906, #10200, #93002 ) ) ;
#348 = EDGE_CURVE ( 'NONE', #76528, #58306, #14323, .T. ) ;
#349 = CARTESIAN_POINT ( 'NONE',  ( -99.52764846858842418, -25.31296290679074090, 3.999772165348554509 ) ) ;
#350 = CARTESIAN_POINT ( 'NONE',  ( -39.56145255469812128, -25.28892524838338929, 3.766659524289464045 ) ) ;
#351 = CARTESIAN_POINT ( 'NONE',  ( -78.52287095715006160, -24.65952944569304606, 1.056160979905698794 ) ) ;
#352 = CARTESIAN_POINT ( 'NONE',  ( -90.62287095715004170, -29.50247984919015209, -1.443849546365051806 ) ) ;
#353 = EDGE_CURVE ( 'NONE', #31349, #84710, #49410, .T. ) ;
#354 = CARTESIAN_POINT ( 'NONE',  ( -25.96779814532654385, -24.61459876899060362, 7.161766614681138066 ) ) ;
#355 = CARTESIAN_POINT ( 'NONE',  ( -42.62287095715004881, -23.72773821059535848, 11.05748984161097503 ) ) ;
#356 = AXIS2_PLACEMENT_3D ( 'NONE', #17788, #64990, #90170 ) ;
#357 = CARTESIAN_POINT ( 'NONE',  ( 19.36532470938277228, 12.59445105952145738, 11.49999999999999645 ) ) ;
#358 = CARTESIAN_POINT ( 'NONE',  ( 21.74077840044056842, -6.890983112422549794, -1.500000000000002220 ) ) ;
#359 = CARTESIAN_POINT ( 'NONE',  ( -74.58800651555678485, -24.34968618360933945, 0.1864209137778816139 ) ) ;
#360 = CARTESIAN_POINT ( 'NONE',  ( -75.52287095715007581, -23.47596703998600631, 11.44779298504228571 ) ) ;
#361 = CARTESIAN_POINT ( 'NONE',  ( -86.52287095715006160, -24.64965694238575011, 8.947790433994196491 ) ) ;
#362 = LOCAL_TIME ( 0, 54, 15.00000000000000000, #80832 ) ;
#363 = CARTESIAN_POINT ( 'NONE',  ( 20.99545381566289137, 7.807860396396394620, 11.49999999999999645 ) ) ;
#364 = EDGE_LOOP ( 'NONE', ( #5040, #85322, #20289, #51409 ) ) ;
#365 = PLANE ( 'NONE',  #20104 ) ;
#366 = CARTESIAN_POINT ( 'NONE',  ( -38.62287095715006302, -24.33927499327853994, 9.819080762295817166 ) ) ;
#367 = CARTESIAN_POINT ( 'NONE',  ( 20.11839708684271244, 8.774209887332036217, 11.49999999999998934 ) ) ;
#368 = CC_DESIGN_PERSON_AND_ORGANIZATION_ASSIGNMENT ( #61991, #8201, ( #21497 ) ) ;
#369 = CARTESIAN_POINT ( 'NONE',  ( -10.34999999999999254, 2.573529411764704733, 1.544117647058823151 ) ) ;
#370 = CARTESIAN_POINT ( 'NONE',  ( -44.57673106130640406, -24.66019654487199375, 8.947790411086115725 ) ) ;
#371 = CARTESIAN_POINT ( 'NONE',  ( -68.94601647182436466, -25.22897554200561387, 6.368117921112105506 ) ) ;
#372 = ORIENTED_EDGE ( 'NONE', *, *, #92617, .T. ) ;
#373 = CARTESIAN_POINT ( 'NONE',  ( -48.98775370671620522, -25.18486450346212990, 6.713331287310639439 ) ) ;
#374 = CARTESIAN_POINT ( 'NONE',  ( -96.62287095715005592, -23.47593901973091235, -1.443836447539001089 ) ) ;
#375 = ORIENTED_EDGE ( 'NONE', *, *, #50984, .T. ) ;
#376 = CARTESIAN_POINT ( 'NONE',  ( 4.362881659454829197, 20.01674633476859810, -1.500000000000002220 ) ) ;
#377 = ORIENTED_EDGE ( 'NONE', *, *, #89296, .T. ) ;
#378 = ORIENTED_EDGE ( 'NONE', *, *, #89968, .F. ) ;
#379 = ORIENTED_EDGE ( 'NONE', *, *, #40213, .F. ) ;
#380 = EDGE_LOOP ( 'NONE', ( #36956, #93992, #32879, #72303 ) ) ;
#381 = CARTESIAN_POINT ( 'NONE',  ( -17.29220519630379016, 15.29500218549028645, -1.500000000000002220 ) ) ;
#382 = CARTESIAN_POINT ( 'NONE',  ( -49.11363384361381890, -25.26016026082141508, 3.839858232430332308 ) ) ;
#383 = CARTESIAN_POINT ( 'NONE',  ( 13.49383759531269433, -15.17088004136028090, -1.500000000000002220 ) ) ;
#384 = EDGE_LOOP ( 'NONE', ( #413, #73949, #56206, #45383 ) ) ;
#385 = DIRECTION ( 'NONE',  ( -3.773278334444167608E-23, 1.000000000000000000, 0.000000000000000000 ) ) ;
#386 = LINE ( 'NONE', #63821, #6032 ) ;
#387 = B_SPLINE_CURVE_WITH_KNOTS ( 'NONE', 3,
 ( #75454, #7448, #84075, #77452, #61762, #29795 ),
 .UNSPECIFIED., .F., .F.,
 ( 4, 2, 4 ),
 ( 0.000000000000000000, 0.001380901958385387027, 0.002761803916770774053 ),
 .UNSPECIFIED. ) ;
#388 = CARTESIAN_POINT ( 'NONE',  ( -47.62287095715004881, -23.48783264082478084, -1.443836473390070596 ) ) ;
#389 = CARTESIAN_POINT ( 'NONE',  ( -70.53622126975956519, -24.83618233451450052, 1.606449574219541487 ) ) ;
#391 = ORIENTED_EDGE ( 'NONE', *, *, #52, .F. ) ;
#390 = CARTESIAN_POINT ( 'NONE',  ( -19.99255411920323056, 7.849732829375159149, 11.49999999999999645 ) ) ;
#392 = LINE ( 'NONE', #46576, #50078 ) ;
#393 = CARTESIAN_POINT ( 'NONE',  ( -28.98875734969026396, -5.965225279485572685, -0.08597719988137648983 ) ) ;
#394 = ORIENTED_EDGE ( 'NONE', *, *, #52108, .F. ) ;
#395 = CARTESIAN_POINT ( 'NONE',  ( 14.61947915221463923, 14.71393552341326760, -1.500000000000002220 ) ) ;
#396 = VERTEX_POINT ( 'NONE', #32781 ) ;
#398 = ORIENTED_EDGE ( 'NONE', *, *, #80161, .T. ) ;
#397 = CARTESIAN_POINT ( 'NONE',  ( -0.02075734969026423599, 0.3587747205144213303, -0.08597719988137648983 ) ) ;
#399 = AXIS2_PLACEMENT_3D ( 'NONE', #34022, #78666, #9681 ) ;
#400 = B_SPLINE_SURFACE_WITH_KNOTS ( 'NONE', 3, 3, ( 
 ( #90759, #84138, #13620, #97377 ),
 ( #20238, #51206, #1425, #69923 ),
 ( #7519, #31361, #38474, #24247 ),
 ( #55220, #22724, #15629, #916 ),
 ( #54714, #47601, #100343, #77019 ),
 ( #86148, #39973, #7021, #31868 ),
 ( #32361, #93755, #84641, #46094 ) ),
 .UNSPECIFIED., .F., .F., .F.,
 ( 4, 3, 4 ),
 ( 4, 4 ),
 ( 0.7945040050992240310, 0.8970133687736498995, 0.9995227324480757680 ),
 ( 0.4095980817935837015, 0.4107999040036969807 ),
 .UNSPECIFIED. ) ;
#401 = CARTESIAN_POINT ( 'NONE',  ( -111.5891399377753004, -24.35071581493544457, 9.817618358456018157 ) ) ;
#402 = CARTESIAN_POINT ( 'NONE',  ( -129.5228709571500758, -23.47596703998600631, 11.44779298504227683 ) ) ;
#403 = ORIENTED_EDGE ( 'NONE', *, *, #6348, .T. ) ;
#404 = VERTEX_POINT ( 'NONE', #20055 ) ;
#405 = CARTESIAN_POINT ( 'NONE',  ( 4.588387839717440464, -6.376774720514401196, 18.52756237589653665 ) ) ;
#406 = DIRECTION ( 'NONE',  ( 0.000000000000000000, 1.000000000000000000, -0.000000000000000000 ) ) ;
#407 = CARTESIAN_POINT ( 'NONE',  ( -65.63576524279528712, -24.52300882791528380, 0.6510814631126250474 ) ) ;
#408 = CARTESIAN_POINT ( 'NONE',  ( 21.96865551644221881, -1.217672407684077918, 11.49999999999999645 ) ) ;
#409 = CARTESIAN_POINT ( 'NONE',  ( 13.10664265030973930, -0.3587747205144256601, -28.18129937523770678 ) ) ;
#410 = CARTESIAN_POINT ( 'NONE',  ( -1.585881643086899606, 22.48459252949185228, 11.49999999999998934 ) ) ;
#411 = CARTESIAN_POINT ( 'NONE',  ( -1.027814097295878693, -20.98676634966329146, 11.49999999999998934 ) ) ;
#412 = CARTESIAN_POINT ( 'NONE',  ( 6.586338672804227024, -6.376774720514415407, 20.10086663068103618 ) ) ;
#413 = ORIENTED_EDGE ( 'NONE', *, *, #99246, .F. ) ;
#414 = VECTOR ( 'NONE', #39030, 1000.000000000000114 ) ;
#415 = EDGE_CURVE ( 'NONE', #68317, #49971, #89571, .T. ) ;
#416 = ORIENTED_EDGE ( 'NONE', *, *, #89969, .T. ) ;
#417 = EDGE_CURVE ( 'NONE', #44756, #35967, #96677, .T. ) ;
#418 = FACE_OUTER_BOUND ( 'NONE', #18116, .T. ) ;
#419 = DIRECTION ( 'NONE',  ( -3.773278334453079030E-23, 0.9999999999976377785, 2.173523156925979128E-06 ) ) ;
#420 = VERTEX_POINT ( 'NONE', #73844 ) ;
#421 = CARTESIAN_POINT ( 'NONE',  ( 19.82261944725993175, 7.364942908566579405, -1.500000000000002220 ) ) ;
#422 = CARTESIAN_POINT ( 'NONE',  ( -99.62287095715005592, -23.48786465467241769, 11.44779295918254114 ) ) ;
#423 = CARTESIAN_POINT ( 'NONE',  ( -50.75822869421170225, -25.26041111912611115, 7.539272917437609856 ) ) ;
#424 = CARTESIAN_POINT ( 'NONE',  ( -121.6252488971726677, -24.15543982623907482, -0.2315651400026574047 ) ) ;
#425 = CARTESIAN_POINT ( 'NONE',  ( -79.52287095715006160, -24.64898659630367916, 1.056161002820826145 ) ) ;
#426 = CARTESIAN_POINT ( 'NONE',  ( -127.5228709571500616, -23.48786465467242479, 11.44779295918253581 ) ) ;
#427 = CARTESIAN_POINT ( 'NONE',  ( 15.99899278244174639, -15.33069297701436184, -1.500000000000002220 ) ) ;
#428 = CARTESIAN_POINT ( 'NONE',  ( -71.51636566736119960, -23.73766607897670156, -1.055555164236456012 ) ) ;
#429 = EDGE_CURVE ( 'NONE', #17186, #23237, #19052, .T. ) ;
#430 = ORIENTED_EDGE ( 'NONE', *, *, #35955, .T. ) ;
#431 = DIRECTION ( 'NONE',  ( 0.000000000000000000, 0.000000000000000000, -1.000000000000000000 ) ) ;
#432 = DIRECTION ( 'NONE',  ( -3.469446951953614189E-15, 1.000000000000000000, 8.673617379884035472E-16 ) ) ;
#433 = CARTESIAN_POINT ( 'NONE',  ( -126.5893519502692754, -24.51314013834316796, 0.6176544820404223923 ) ) ;
#434 = CARTESIAN_POINT ( 'NONE',  ( -100.6255027387640979, -24.83618233451450763, 1.606449574219537713 ) ) ;
#435 = DIRECTION ( 'NONE',  ( -0.000000000000000000, 1.000000000000000000, -0.000000000000000000 ) ) ;
#436 = VECTOR ( 'NONE', #75067, 1000.000000000000000 ) ;
#437 = CARTESIAN_POINT ( 'NONE',  ( 8.422564666779264186, -17.53554878399664574, 11.49999999999998934 ) ) ;
#438 = LOCAL_TIME ( 0, 54, 15.00000000000000000, #59492 ) ;
#439 = CARTESIAN_POINT ( 'NONE',  ( -12.70309173801008562, -17.24390854791867511, -1.500000000000002220 ) ) ;
#440 = CARTESIAN_POINT ( 'NONE',  ( -62.55373037630388211, -23.96119346886881019, -0.6495511937832096905 ) ) ;
#441 = CARTESIAN_POINT ( 'NONE',  ( -60.65501803048972107, -23.85049219812968602, 10.88485053497088728 ) ) ;
#442 = CARTESIAN_POINT ( 'NONE',  ( -51.53639160008312103, -24.51314013834315730, 0.6176544820404109570 ) ) ;
#443 = CARTESIAN_POINT ( 'NONE',  ( -100.7282901814618583, -25.27359982393476656, 3.329829818474457692 ) ) ;
#444 = CARTESIAN_POINT ( 'NONE',  ( -0.6305239314742796530, -22.70799625201654592, -1.500000000000002220 ) ) ;
#445 = CARTESIAN_POINT ( 'NONE',  ( -98.63223275675622403, -23.96119346886881019, -0.6495511937832081362 ) ) ;
#446 = CARTESIAN_POINT ( 'NONE',  ( 27.86270917940689174, -5.965225279485572685, 29.49402280011862487 ) ) ;
#447 = CARTESIAN_POINT ( 'NONE',  ( -19.70454523906213495, -2.556213046838741842, 11.49999999999999645 ) ) ;
#448 = CARTESIAN_POINT ( 'NONE',  ( 6.259688558337090036, -6.376774720514413630, 19.73360741988579292 ) ) ;
#449 = AXIS2_PLACEMENT_3D ( 'NONE', #43723, #56962, #58459 ) ;
#450 = CARTESIAN_POINT ( 'NONE',  ( -38.62287095715005592, -29.50250786944525672, 11.44777988621624232 ) ) ;
#451 = VERTEX_POINT ( 'NONE', #89074 ) ;
#452 = DIRECTION ( 'NONE',  ( -1.000000000000000000, -0.000000000000000000, 0.000000000000000000 ) ) ;
#453 = CARTESIAN_POINT ( 'NONE',  ( -80.52287095715006160, -24.99156044556202616, 7.747789690856173195 ) ) ;
#454 = CARTESIAN_POINT ( 'NONE',  ( 10.34999999999999254, 4.999999999999998224, 2.100000000000000089 ) ) ;
#455 = CARTESIAN_POINT ( 'NONE',  ( 21.64940796807912449, -0.2623997510114038922, -1.500000000000002220 ) ) ;
#456 = CARTESIAN_POINT ( 'NONE',  ( -29.62287095715004881, -23.64926103841893124, 11.05761042169888597 ) ) ;
#457 = CARTESIAN_POINT ( 'NONE',  ( -19.27395093635484713, 2.380100695660296140, -1.500000000000002220 ) ) ;
#458 = CARTESIAN_POINT ( 'NONE',  ( -55.58285685940607834, -24.73531770709094957, 8.716586749053510275 ) ) ;
#459 = CARTESIAN_POINT ( 'NONE',  ( 4.164567180745167185, 19.39263604865329071, 11.49999999999998934 ) ) ;
#460 = EDGE_CURVE ( 'NONE', #77487, #13521, #16037, .T. ) ;
#461 = ORIENTED_EDGE ( 'NONE', *, *, #57251, .T. ) ;
#462 = CARTESIAN_POINT ( 'NONE',  ( -17.59887021274124663, -10.25344800880639262, 11.49999999999999645 ) ) ;
#463 = LINE ( 'NONE', #45650, #65151 ) ;
#464 = EDGE_CURVE ( 'NONE', #42504, #27734, #71857, .T. ) ;
#466 = AXIS2_PLACEMENT_3D ( 'NONE', #79939, #73829, #3833 ) ;
#465 = CARTESIAN_POINT ( 'NONE',  ( -9.383883476483159569, 17.86611652351680846, 2.100000000000000089 ) ) ;
#467 = ORIENTED_EDGE ( 'NONE', *, *, #43495, .T. ) ;
#468 = B_SPLINE_CURVE_WITH_KNOTS ( 'NONE', 3,
 ( #83772, #68559, #83277, #53344, #90893, #52341 ),
 .UNSPECIFIED., .F., .F.,
 ( 4, 2, 4 ),
 ( 0.000000000000000000, 0.001380901958385393966, 0.002761803916770787931 ),
 .UNSPECIFIED. ) ;
#469 = CARTESIAN_POINT ( 'NONE',  ( -30.64427850938830744, -23.56000036390796026, 11.50200000000000600 ) ) ;
#470 = CARTESIAN_POINT ( 'NONE',  ( -111.3776484685884469, -25.29712067403330877, 4.332404411321261861 ) ) ;
#471 = CARTESIAN_POINT ( 'NONE',  ( -48.90136019426822145, -25.25214628733238342, 5.866402775706137440 ) ) ;
#472 = DIRECTION ( 'NONE',  ( 1.000000000000000000, 0.000000000000000000, 0.000000000000000000 ) ) ;
#473 = DIRECTION ( 'NONE',  ( -1.000000000000000000, -0.000000000000000000, -0.000000000000000000 ) ) ;
#474 = CARTESIAN_POINT ( 'NONE',  ( 19.67429046578372365, -4.105084037421226739, -1.500000000000002220 ) ) ;
#475 = DIRECTION ( 'NONE',  ( -0.9496245541219268116, -6.454799914155188842E-16, -0.3133898629642187239 ) ) ;
#476 = AXIS2_PLACEMENT_3D ( 'NONE', #41465, #33338, #88143 ) ;
#477 = VERTEX_POINT ( 'NONE', #49023 ) ;
#478 = CARTESIAN_POINT ( 'NONE',  ( -107.6228709571500701, -23.48786465467241769, 11.44779295918253936 ) ) ;
#479 = CARTESIAN_POINT ( 'NONE',  ( 1.119804705421552748, 22.86502198858056545, 11.49999999999999645 ) ) ;
#480 = CARTESIAN_POINT ( 'NONE',  ( -10.65177407370799045, -20.06881281718593613, 11.49999999999998934 ) ) ;
#481 = EDGE_LOOP ( 'NONE', ( #19965, #25245, #83249, #77513 ) ) ;
#482 = CARTESIAN_POINT ( 'NONE',  ( -71.70841769935766763, -25.25720466352798255, 6.192981421160952848 ) ) ;
#483 = VECTOR ( 'NONE', #28798, 1000.000000000000000 ) ;
#484 = DIRECTION ( 'NONE',  ( 0.000000000000000000, -0.9999999999976377785, -2.173523156925979975E-06 ) ) ;
#485 = CARTESIAN_POINT ( 'NONE',  ( -38.58688038665032138, -24.35071581493542325, 9.817618358456030592 ) ) ;
#486 = DIRECTION ( 'NONE',  ( 0.000000000000000000, 0.9999999999976377785, 2.173523156925979975E-06 ) ) ;
#487 = EDGE_CURVE ( 'NONE', #56501, #14750, #63985, .T. ) ;
#488 = APPROVAL ( #44397, 'UNSPECIFIED' ) ;
#489 = CARTESIAN_POINT ( 'NONE',  ( -128.5559268670633628, -23.96169478059714919, 10.65365249895717170 ) ) ;
#490 = DIRECTION ( 'NONE',  ( 0.000000000000000000, 0.000000000000000000, 1.000000000000000000 ) ) ;
#491 = EDGE_LOOP ( 'NONE', ( #43848, #52174, #5109, #74657 ) ) ;
#492 = CARTESIAN_POINT ( 'NONE',  ( 19.91419669613914678, 4.404666692190684962, 11.49999999999998934 ) ) ;
#493 = ORIENTED_EDGE ( 'NONE', *, *, #85072, .F. ) ;
#494 = CARTESIAN_POINT ( 'NONE',  ( -18.50152239663938403, 13.63810111590111163, 11.49999999999998934 ) ) ;
#495 = CARTESIAN_POINT ( 'NONE',  ( -54.50227307414417766, -24.15620529776628089, 10.23563542870661180 ) ) ;
#497 = VERTEX_POINT ( 'NONE', #65759 ) ;
#496 = ADVANCED_FACE ( 'NONE', ( #26678 ), #64262, .F. ) ;
#498 = CARTESIAN_POINT ( 'NONE',  ( -108.5134006316627051, -24.51419770103157347, 9.386484678747168076 ) ) ;
#499 = CARTESIAN_POINT ( 'NONE',  ( -80.77625289099501060, -25.13967656840255671, 7.064051687917259237 ) ) ;
#500 = VECTOR ( 'NONE', #98403, 1000.000000000000114 ) ;
#501 = CARTESIAN_POINT ( 'NONE',  ( -111.5228709571500616, -23.47596703998600631, 11.44779298504228038 ) ) ;
#503 = VERTEX_POINT ( 'NONE', #81467 ) ;
#502 = CARTESIAN_POINT ( 'NONE',  ( 19.59546714036918758, 8.467717511154198462, 11.49999999999999645 ) ) ;
#504 = CC_DESIGN_APPROVAL ( #6561, ( #31288 ) ) ;
#505 = ORIENTED_EDGE ( 'NONE', *, *, #37962, .F. ) ;
#506 = CARTESIAN_POINT ( 'NONE',  ( -2.516727866726558460, 22.04588476715296963, -1.500000000000002220 ) ) ;
#507 = CARTESIAN_POINT ( 'NONE',  ( 6.115004186001010922, -19.73231167505474559, 11.49999999999998934 ) ) ;
#508 = ADVANCED_BREP_SHAPE_REPRESENTATION ( '', ( #42246, #37391 ), #19636 ) ;
#509 = EDGE_LOOP ( 'NONE', ( #49662, #42848, #63810, #16595 ) ) ;
#511 = ORIENTED_EDGE ( 'NONE', *, *, #19314, .F. ) ;
#510 = AXIS2_PLACEMENT_3D ( 'NONE', #90538, #91038, #83925 ) ;
#512 = CARTESIAN_POINT ( 'NONE',  ( -109.8219511710470897, -25.27682916472742747, 5.738454893586274252 ) ) ;
#513 = CARTESIAN_POINT ( 'NONE',  ( -69.85667726116794540, -25.25978459231412288, 3.590539514744167437 ) ) ;
#514 = ORIENTED_EDGE ( 'NONE', *, *, #94702, .T. ) ;
#515 = CARTESIAN_POINT ( 'NONE',  ( -91.51496719381653122, -23.96119346886880663, -0.6495511937832073590 ) ) ;
#516 = ORIENTED_EDGE ( 'NONE', *, *, #47148, .F. ) ;
#517 = VECTOR ( 'NONE', #47089, 1000.000000000000000 ) ;
#518 = CARTESIAN_POINT ( 'NONE',  ( -58.65647576671169361, -23.48786465467241058, 11.44779295918254824 ) ) ;
#519 = B_SPLINE_CURVE_WITH_KNOTS ( 'NONE', 3,
 ( #29528, #59008, #59497, #60009 ),
 .UNSPECIFIED., .F., .F.,
 ( 4, 4 ),
 ( 0.000000000000000000, 9.999999999999592548E-05 ),
 .UNSPECIFIED. ) ;
#520 = CARTESIAN_POINT ( 'NONE',  ( -72.62287095715005592, -29.50250786944525672, 11.44777988621623699 ) ) ;
#521 = CARTESIAN_POINT ( 'NONE',  ( 20.60118427460899326, -2.865472796819775958, -1.500000000000002220 ) ) ;
#522 = EDGE_CURVE ( 'NONE', #9188, #31632, #19306, .T. ) ;
#523 = CARTESIAN_POINT ( 'NONE',  ( 21.44370820036873937, 4.193779532373530294, 11.49999999999999645 ) ) ;
#524 = CARTESIAN_POINT ( 'NONE',  ( -36.52287095715006870, -23.47596703998600631, 11.44779298504229281 ) ) ;
#525 = CARTESIAN_POINT ( 'NONE',  ( -100.0539824966801064, -25.04132515376273815, 7.523549795824772346 ) ) ;
#526 = CARTESIAN_POINT ( 'NONE',  ( -22.07377061809603092, 4.253497373390751513, 11.49999999999998934 ) ) ;
#527 = DIRECTION ( 'NONE',  ( 0.000000000000000000, 2.173523156925980399E-06, -0.9999999999976378895 ) ) ;
#528 = DIRECTION ( 'NONE',  ( 0.000000000000000000, 2.173523156925980399E-06, -0.9999999999976378895 ) ) ;
#529 = LINE ( 'NONE', #48220, #79852 ) ;
#530 = B_SPLINE_SURFACE_WITH_KNOTS ( 'NONE', 3, 3, ( 
 ( #12800, #88452, #89940, #49903 ),
 ( #43775, #66634, #74220, #34665 ),
 ( #5201, #18924, #97549, #50393 ),
 ( #28532, #11815, #19922, #44276 ),
 ( #73230, #59496, #20407, #74703 ),
 ( #28049, #59007, #65137, #96551 ),
 ( #89446, #36159, #5698, #12302 ) ),
 .UNSPECIFIED., .F., .F., .F.,
 ( 4, 3, 4 ),
 ( 4, 4 ),
 ( 0.0004766839783837975792, 0.1029713700210903304, 0.2054660560637968647 ),
 ( 0.8297050600404040077, 0.8311006089866127544 ),
 .UNSPECIFIED. ) ;
#531 = EDGE_LOOP ( 'NONE', ( #4697, #60989, #55794, #22828 ) ) ;
#532 = EDGE_LOOP ( 'NONE', ( #32047, #70301, #41788, #57216 ) ) ;
#533 = EDGE_CURVE ( 'NONE', #69177, #58343, #27177, .T. ) ;
#534 = VERTEX_POINT ( 'NONE', #2346 ) ;
#535 = B_SPLINE_CURVE_WITH_KNOTS ( 'NONE', 3,
 ( #98354, #82143, #12628, #12120 ),
 .UNSPECIFIED., .F., .F.,
 ( 4, 4 ),
 ( 0.000000000000000000, 9.999999999998897304E-05 ),
 .UNSPECIFIED. ) ;
#536 = CARTESIAN_POINT ( 'NONE',  ( 9.714863677370791706, 19.00186346016302608, -1.500000000000002220 ) ) ;
#537 = ORIENTED_EDGE ( 'NONE', *, *, #81268, .F. ) ;
#538 = CARTESIAN_POINT ( 'NONE',  ( -19.68365937621761219, -7.520201837432793468, 11.49999999999998934 ) ) ;
#539 = CARTESIAN_POINT ( 'NONE',  ( -30.49551068477055082, -24.38002254354092102, 0.3015907515355735202 ) ) ;
#540 = CARTESIAN_POINT ( 'NONE',  ( 10.26108024787556516, -17.11367029881254709, -1.500000000000002220 ) ) ;
#541 = CARTESIAN_POINT ( 'NONE',  ( -50.52448152296889106, -25.00182538069147142, 7.747789668545043362 ) ) ;
#542 = CARTESIAN_POINT ( 'NONE',  ( -50.18441529348658747, -25.04472180003372728, 7.555573460512422734 ) ) ;
#543 = CARTESIAN_POINT ( 'NONE',  ( 21.99661117994144988, 0.4758108284031232760, -1.500000000000002220 ) ) ;
#544 = CARTESIAN_POINT ( 'NONE',  ( 2.499999999999995115, 19.99999999999999645, 2.100000000000000089 ) ) ;
#545 = ORIENTED_EDGE ( 'NONE', *, *, #54619, .T. ) ;
#546 = CARTESIAN_POINT ( 'NONE',  ( -30.64535876238280565, -23.53198925593397917, 11.48393099501408976 ) ) ;
#547 = EDGE_CURVE ( 'NONE', #74034, #7838, #11942, .T. ) ;
#548 = VECTOR ( 'NONE', #22485, 1000.000000000000114 ) ;
#549 = CARTESIAN_POINT ( 'NONE',  ( -54.62287095715004170, -23.47596703998600631, 11.44779298504227505 ) ) ;
#550 = CARTESIAN_POINT ( 'NONE',  ( -19.40898059523135544, 7.551958013340856368, 11.49999999999999645 ) ) ;
#551 = ADVANCED_FACE ( 'NONE', ( #80960 ), #76509, .T. ) ;
#552 = CARTESIAN_POINT ( 'NONE',  ( 31.63587494018430135, -3.477878053198200536, 27.33969830395653844 ) ) ;
#553 = VECTOR ( 'NONE', #56652, 1000.000000000000114 ) ;
#554 = LINE ( 'NONE', #43992, #61943 ) ;
#555 = PLANE ( 'NONE',  #88668 ) ;
#556 = CARTESIAN_POINT ( 'NONE',  ( 20.93798385506118365, 3.901641247904229282, 11.49999999999998934 ) ) ;
#557 = CARTESIAN_POINT ( 'NONE',  ( -29.58953762381671737, -24.57142930420317128, 8.947790468830323363 ) ) ;
#558 = CARTESIAN_POINT ( 'NONE',  ( -54.62287095715005592, -23.47593901973091235, -1.443836447539009749 ) ) ;
#559 = CARTESIAN_POINT ( 'NONE',  ( -61.52287095715006160, -23.47596703998600631, 11.44779298504228926 ) ) ;
#560 = DIRECTION ( 'NONE',  ( 0.000000000000000000, -0.9999999999976377785, -2.173523156925979128E-06 ) ) ;
#561 = CARTESIAN_POINT ( 'NONE',  ( -5.199590022849982063, -21.90925200621149571, -1.500000000000002220 ) ) ;
#562 = CARTESIAN_POINT ( 'NONE',  ( -56.52287095715006870, -23.47596703998600631, 11.44779298504228926 ) ) ;
#563 = ORIENTED_EDGE ( 'NONE', *, *, #297, .T. ) ;
#564 = LINE ( 'NONE', #70079, #40146 ) ;
#565 = CARTESIAN_POINT ( 'NONE',  ( 7.987771016649366729, -18.01272016045900415, 11.49999999999999645 ) ) ;
#566 = LINE ( 'NONE', #91908, #14699 ) ;
#567 = DIRECTION ( 'NONE',  ( -1.000000000000000000, 0.000000000000000000, -3.469446951953617147E-16 ) ) ;
#568 = ORIENTED_EDGE ( 'NONE', *, *, #24222, .F. ) ;
#569 = CARTESIAN_POINT ( 'NONE',  ( -123.6228709571500559, -24.65952944569304961, 1.056160979905703234 ) ) ;
#570 = LINE ( 'NONE', #31018, #59416 ) ;
#571 = CARTESIAN_POINT ( 'NONE',  ( -100.3128489789178559, -25.25095783679409323, 5.229225670637348777 ) ) ;
#572 = CARTESIAN_POINT ( 'NONE',  ( 8.071512145086529699, -9.528487854913505473, 6.500000000000001776 ) ) ;
#573 = B_SPLINE_CURVE_WITH_KNOTS ( 'NONE', 3,
 ( #10709, #72616, #34049, #51647, #59764, #80721 ),
 .UNSPECIFIED., .F., .F.,
 ( 4, 2, 4 ),
 ( 0.07528258264012024914, 0.07727090165436052704, 0.07925922066860080495 ),
 .UNSPECIFIED. ) ;
#574 = VECTOR ( 'NONE', #95324, 1000.000000000000114 ) ;
#575 = CARTESIAN_POINT ( 'NONE',  ( 12.99534586470982234, -14.87506298573330632, 11.49999999999998934 ) ) ;
#576 = ORIENTED_EDGE ( 'NONE', *, *, #40914, .F. ) ;
#577 = CARTESIAN_POINT ( 'NONE',  ( -109.7483548522739056, -25.21846411683590716, 3.465899786825440643 ) ) ;
#578 = VECTOR ( 'NONE', #51125, 1000.000000000000114 ) ;
#579 = EDGE_CURVE ( 'NONE', #41954, #33250, #45247, .T. ) ;
#580 = SHAPE_DEFINITION_REPRESENTATION ( #87904, #55609 ) ;
#581 = ORIENTED_EDGE ( 'NONE', *, *, #67321, .F. ) ;
#582 = CARTESIAN_POINT ( 'NONE',  ( -124.5228709571500758, -23.95044443724993144, 10.65354141964648882 ) ) ;
#583 = PLANE ( 'NONE',  #76593 ) ;
#584 = CARTESIAN_POINT ( 'NONE',  ( -65.62287095715005592, -23.48786465467241058, 11.44779295918254647 ) ) ;
#585 = CARTESIAN_POINT ( 'NONE',  ( -99.20586904084365187, -25.26638419840477923, 7.003176680450737379 ) ) ;
#586 = CARTESIAN_POINT ( 'NONE',  ( 8.160000000000000142, -2.191226316053958875E-18, 2.701633758479787833E-17 ) ) ;
#587 = CARTESIAN_POINT ( 'NONE',  ( 15.63605935613269438, -6.475225279485573360, -27.55169773172585934 ) ) ;
#588 = AXIS2_PLACEMENT_3D ( 'NONE', #34020, #81693, #56876 ) ;
#589 = CARTESIAN_POINT ( 'NONE',  ( -124.5228709571500616, -24.65952944569305316, 1.056160979905705899 ) ) ;
#590 = CARTESIAN_POINT ( 'NONE',  ( -16.75416981316412190, 10.96944243606782443, 11.49999999999998934 ) ) ;
#591 = CARTESIAN_POINT ( 'NONE',  ( -4.621320343559618848, 12.50000000000004974, 2.100000000000000089 ) ) ;
#592 = DIRECTION ( 'NONE',  ( -3.773278334453079030E-23, 0.9999999999976377785, 2.173523156925979128E-06 ) ) ;
#593 = ORIENTED_EDGE ( 'NONE', *, *, #9471, .T. ) ;
#594 = CARTESIAN_POINT ( 'NONE',  ( -56.62287095715005592, -29.50247984919015209, -1.443849546365056913 ) ) ;
#595 = CARTESIAN_POINT ( 'NONE',  ( -73.55620429048340725, -23.47596703998600276, 11.44779298504227683 ) ) ;
#596 = CARTESIAN_POINT ( 'NONE',  ( -120.6228709571500701, -25.00158670708909625, 2.256160236439166411 ) ) ;
#597 = CARTESIAN_POINT ( 'NONE',  ( -82.55620429048339304, -24.64965694238575011, 8.947790433994194714 ) ) ;
#598 = CARTESIAN_POINT ( 'NONE',  ( 0.000000000000000000, -1.473225279485573802, 0.000000000000000000 ) ) ;
#599 = DIRECTION ( 'NONE',  ( 0.000000000000000000, 0.000000000000000000, -1.000000000000000000 ) ) ;
#600 = ADVANCED_FACE ( 'NONE', ( #28667 ), #59629, .T. ) ;
#601 = B_SPLINE_SURFACE_WITH_KNOTS ( 'NONE', 3, 3, ( 
 ( #8281, #91510, #21989, #83905 ),
 ( #45359, #37730, #99610, #3190 ),
 ( #17899, #80295, #25507, #32618 ),
 ( #86404, #64098, #23997, #54966 ),
 ( #40733, #10788, #71692, #86901 ),
 ( #56977, #17393, #95016, #41752 ),
 ( #33623, #16383, #33120, #56480 ),
 ( #47349, #16889, #87404, #94515 ),
 ( #78273, #1679, #8784, #39722 ),
 ( #55974, #49366, #64605, #63593 ) ),
 .UNSPECIFIED., .F., .F., .F.,
 ( 4, 3, 3, 4 ),
 ( 4, 4 ),
 ( 0.7022005934544808259, 0.7765311282028796169, 0.8508616629512784080, 0.9995227324480761011 ),
 ( 0.4495482509261787829, 0.4508289003306459319 ),
 .UNSPECIFIED. ) ;
#602 = CARTESIAN_POINT ( 'NONE',  ( -3.035630128403670192, -5.876774720514413630, 19.71630089903357685 ) ) ;
#603 = EDGE_CURVE ( 'NONE', #68323, #2429, #30152, .T. ) ;
#604 = CARTESIAN_POINT ( 'NONE',  ( 5.541369867593821219, -5.876774720514425177, 21.42815349816763160 ) ) ;
#605 = ORIENTED_EDGE ( 'NONE', *, *, #96875, .F. ) ;
#606 = B_SPLINE_CURVE_WITH_KNOTS ( 'NONE', 3,
 ( #65863, #97282, #4446, #35397 ),
 .UNSPECIFIED., .F., .F.,
 ( 4, 4 ),
 ( 0.3500358765290026430, 0.3590423078011182323 ),
 .UNSPECIFIED. ) ;
#607 =( REPRESENTATION_RELATIONSHIP ('NONE','NONE', #96270, #9419 ) REPRESENTATION_RELATIONSHIP_WITH_TRANSFORMATION ( #9956 )SHAPE_REPRESENTATION_RELATIONSHIP( ) );
#608 = CARTESIAN_POINT ( 'NONE',  ( 9.679018533540549640, -17.85022214266596308, -1.500000000000002220 ) ) ;
#609 = CARTESIAN_POINT ( 'NONE',  ( -115.5228709571500474, -23.47593901973090524, -1.443836447538996204 ) ) ;
#610 = VECTOR ( 'NONE', #64166, 1000.000000000000000 ) ;
#611 = ADVANCED_FACE ( 'NONE', ( #5824 ), #44904, .F. ) ;
#612 = CARTESIAN_POINT ( 'NONE',  ( -127.6228709571500275, -23.48786465467242124, 11.44779295918253403 ) ) ;
#613 = ADVANCED_FACE ( 'NONE', ( #67746 ), #98663, .F. ) ;
#614 = ORIENTED_EDGE ( 'NONE', *, *, #19902, .T. ) ;
#615 = CARTESIAN_POINT ( 'NONE',  ( -114.5228709571500616, -29.50250786944525672, 11.44777988621622988 ) ) ;
#616 = CARTESIAN_POINT ( 'NONE',  ( -17.82723130383223165, -9.322377578706960932, -1.500000000000002220 ) ) ;
#617 = AXIS2_PLACEMENT_3D ( 'NONE', #79498, #95727, #71902 ) ;
#618 = CARTESIAN_POINT ( 'NONE',  ( 19.82261944725993175, 7.364942908566579405, 11.49999999999999645 ) ) ;
#619 = ADVANCED_FACE ( 'NONE', ( #75826 ), #60135, .F. ) ;
#620 = CARTESIAN_POINT ( 'NONE',  ( -21.51168160490077952, -5.175097382202364926, -1.500000000000002220 ) ) ;
#621 = CARTESIAN_POINT ( 'NONE',  ( -10.41206725544052780, -17.73373708237225799, -1.500000000000002220 ) ) ;
#622 = CARTESIAN_POINT ( 'NONE',  ( -60.55976763516859052, -23.85016227208580375, -0.8807180028928355275 ) ) ;
#623 = VERTEX_POINT ( 'NONE', #90068 ) ;
#624 = CARTESIAN_POINT ( 'NONE',  ( -94.52287095715003318, -24.66019654487199730, 8.947790411086124607 ) ) ;
#625 = ORIENTED_EDGE ( 'NONE', *, *, #15400, .T. ) ;
#626 = CARTESIAN_POINT ( 'NONE',  ( -85.62287095715004170, -23.85229601348996908, 10.88205029486207742 ) ) ;
#627 = EDGE_LOOP ( 'NONE', ( #68451, #54996, #83617, #2674, #2516, #91000, #34023, #57845, #97952, #9654, #26816, #51309 ) ) ;
#628 = VERTEX_POINT ( 'NONE', #45401 ) ;
#629 = ORIENTED_EDGE ( 'NONE', *, *, #80597, .T. ) ;
#630 = CARTESIAN_POINT ( 'NONE',  ( -103.5228709571500758, -23.48786465467241769, 11.44779295918254114 ) ) ;
#631 = CARTESIAN_POINT ( 'NONE',  ( -50.18456845782914399, -25.03449303489322020, 7.555577232638461815 ) ) ;
#632 = CARTESIAN_POINT ( 'NONE',  ( -68.63108587404039440, -24.35071581493542681, 9.817618358456032368 ) ) ;
#633 = CARTESIAN_POINT ( 'NONE',  ( -15.36756058500021282, 13.76162614515376426, -1.500000000000002220 ) ) ;
#634 = EDGE_CURVE ( 'NONE', #82156, #32410, #91059, .T. ) ;
#635 = CARTESIAN_POINT ( 'NONE',  ( -2.642555958445479192, -21.45212208726272607, 11.49999999999999645 ) ) ;
#636 = ORIENTED_EDGE ( 'NONE', *, *, #46341, .F. ) ;
#637 = CARTESIAN_POINT ( 'NONE',  ( -46.62287095715004881, -24.64965695001467694, 8.947790433994185832 ) ) ;
#638 = CARTESIAN_POINT ( 'NONE',  ( 2.834823996951755465, -5.876774720514406525, 18.76222163777333307 ) ) ;
#639 = CARTESIAN_POINT ( 'NONE',  ( -6.430504157862594994, -21.42354456762059201, -1.500000000000002220 ) ) ;
#640 = CARTESIAN_POINT ( 'NONE',  ( -47.54693701500606551, -24.15620529776627379, 10.23563542870660825 ) ) ;
#641 = DIRECTION ( 'NONE',  ( 0.000000000000000000, -0.000000000000000000, 1.000000000000000000 ) ) ;
#642 = VERTEX_POINT ( 'NONE', #43407 ) ;
#643 = CARTESIAN_POINT ( 'NONE',  ( -117.7763468626476850, -25.31365013357615368, 6.500921039148880531 ) ) ;
#644 = CARTESIAN_POINT ( 'NONE',  ( -76.62287095715009855, -23.95044443724992433, 10.65354141964649948 ) ) ;
#645 = B_SPLINE_CURVE_WITH_KNOTS ( 'NONE', 3,
 ( #31561, #54913, #56430, #2635, #32062, #40689 ),
 .UNSPECIFIED., .F., .F.,
 ( 4, 2, 4 ),
 ( 0.000000000000000000, 0.0005049716539041804782, 0.001009943307808368112 ),
 .UNSPECIFIED. ) ;
#646 = CARTESIAN_POINT ( 'NONE',  ( -0.7727808018759799724, -20.89725122839497828, -1.500000000000002220 ) ) ;
#647 = VERTEX_POINT ( 'NONE', #21533 ) ;
#649 = EDGE_CURVE ( 'NONE', #44273, #78408, #52510, .T. ) ;
#648 = FACE_OUTER_BOUND ( 'NONE', #26996, .T. ) ;
#650 = ORIENTED_EDGE ( 'NONE', *, *, #19881, .T. ) ;
#651 = CARTESIAN_POINT ( 'NONE',  ( -128.6228709571500417, -23.47596703998600631, 11.44779298504227860 ) ) ;
#652 = CARTESIAN_POINT ( 'NONE',  ( 15.88363568188429653, -14.04911357082368006, -1.500000000000002220 ) ) ;
#653 = EDGE_CURVE ( 'NONE', #30045, #37372, #13928, .T. ) ;
#654 = VERTEX_POINT ( 'NONE', #37281 ) ;
#655 = CARTESIAN_POINT ( 'NONE',  ( -69.62287095715005592, -23.48783264082478084, -1.443836473390067265 ) ) ;
#656 = CARTESIAN_POINT ( 'NONE',  ( -20.50126671893153940, -7.481214725051755110, -1.500000000000002220 ) ) ;
#657 = CARTESIAN_POINT ( 'NONE',  ( -7.338700834008208496, -6.376774720514410077, 19.35116211686183263 ) ) ;
#658 = CARTESIAN_POINT ( 'NONE',  ( -76.52212335552069078, -23.48786465467240703, 11.44779295918254647 ) ) ;
#659 = DIRECTION ( 'NONE',  ( 0.000000000000000000, 0.000000000000000000, 1.000000000000000000 ) ) ;
#660 = CARTESIAN_POINT ( 'NONE',  ( 12.66963027563507005, -17.75133666976559255, -1.500000000000002220 ) ) ;
#661 = CARTESIAN_POINT ( 'NONE',  ( 6.480733632922428988, -5.876774720514425177, 21.47849199606610782 ) ) ;
#662 = ORIENTED_EDGE ( 'NONE', *, *, #86913, .T. ) ;
#663 = CARTESIAN_POINT ( 'NONE',  ( 0.6000000000000007550, 0.000000000000000000, 24.00000000000000000 ) ) ;
#664 = CYLINDRICAL_SURFACE ( 'NONE', #80009, 2.040000000000000036 ) ;
#666 = ORIENTED_EDGE ( 'NONE', *, *, #32067, .F. ) ;
#665 = EDGE_CURVE ( 'NONE', #22596, #17009, #37775, .T. ) ;
#667 = EDGE_CURVE ( 'NONE', #75528, #29344, #20541, .T. ) ;
#668 = ORIENTED_EDGE ( 'NONE', *, *, #7979, .F. ) ;
#669 = EDGE_CURVE ( 'NONE', #38959, #72936, #20443, .T. ) ;
#670 = ORIENTED_EDGE ( 'NONE', *, *, #44735, .F. ) ;
#671 = CARTESIAN_POINT ( 'NONE',  ( -28.72238104702265105, -24.94777617903022460, 2.725261753396577280 ) ) ;
#672 = LINE ( 'NONE', #31619, #25422 ) ;
#673 = CARTESIAN_POINT ( 'NONE',  ( -6.347832186973104029, -20.24257907634199682, -1.500000000000002220 ) ) ;
#674 = CARTESIAN_POINT ( 'NONE',  ( -94.51866586401287407, -23.73766607897670156, -1.055555164236450905 ) ) ;
#675 = CARTESIAN_POINT ( 'NONE',  ( -79.88583274576632220, -25.27791948829852586, 7.452192272885968194 ) ) ;
#676 = AXIS2_PLACEMENT_3D ( 'NONE', #42786, #67617, #36160 ) ;
#677 = LINE ( 'NONE', #8797, #47034 ) ;
#678 = DIRECTION ( 'NONE',  ( 0.000000000000000000, -1.000000000000000000, 0.000000000000000000 ) ) ;
#679 = CARTESIAN_POINT ( 'NONE',  ( 0.06232057257353295493, 19.38168652127415825, -1.500000000000002220 ) ) ;
#680 = EDGE_CURVE ( 'NONE', #63086, #95598, #33946, .T. ) ;
#681 = CARTESIAN_POINT ( 'NONE',  ( -70.23274567164976645, -25.31150975387220825, 5.317581533080277367 ) ) ;
#682 = ORIENTED_EDGE ( 'NONE', *, *, #31445, .F. ) ;
#683 = CARTESIAN_POINT ( 'NONE',  ( -3.338044803349280443, -19.22079736023769669, 11.49999999999999645 ) ) ;
#684 = FACE_OUTER_BOUND ( 'NONE', #2410, .T. ) ;
#685 = CARTESIAN_POINT ( 'NONE',  ( -107.5895376238167387, -24.65952944569304250, 1.056160979905697683 ) ) ;
#686 = ORIENTED_EDGE ( 'NONE', *, *, #93583, .T. ) ;
#687 = VECTOR ( 'NONE', #5114, 1000.000000000000000 ) ;
#688 = CARTESIAN_POINT ( 'NONE',  ( 4.780030342074717886, -6.376774720514424288, 21.16398229115527130 ) ) ;
#689 = CARTESIAN_POINT ( 'NONE',  ( -70.74026866089612042, -25.30511070033976395, 4.894904393956083233 ) ) ;
#690 = PLANE ( 'NONE',  #1809 ) ;
#691 = CARTESIAN_POINT ( 'NONE',  ( -29.49875734969026198, 5.965225279485572685, 10.11402280011862587 ) ) ;
#692 = CARTESIAN_POINT ( 'NONE',  ( 9.421224358276909072, -17.24829524558457194, -1.500000000000002220 ) ) ;
#693 = B_SPLINE_CURVE_WITH_KNOTS ( 'NONE', 3,
 ( #53453, #45830, #13000, #66827, #15360, #59703 ),
 .UNSPECIFIED., .F., .F.,
 ( 4, 2, 4 ),
 ( 0.000000000000000000, 0.001380764517854760629, 0.002761529035709521258 ),
 .UNSPECIFIED. ) ;
#694 = CARTESIAN_POINT ( 'NONE',  ( -28.98875734969026396, -6.376774720514426953, -0.08597719988137648983 ) ) ;
#695 = ORIENTED_EDGE ( 'NONE', *, *, #80167, .T. ) ;
#696 = CARTESIAN_POINT ( 'NONE',  ( 0.9236959384754221958, 21.56878955078795812, -1.500000000000002220 ) ) ;
#697 = CARTESIAN_POINT ( 'NONE',  ( -40.62644336949313129, -24.92564183028978775, 1.928384488918254203 ) ) ;
#698 = DIRECTION ( 'NONE',  ( -1.000000000000000000, -3.773278334444166432E-23, -8.201307841325785021E-29 ) ) ;
#699 = CARTESIAN_POINT ( 'NONE',  ( 23.03040035405544472, 1.057182387018521963, -1.500000000000002220 ) ) ;
#700 = PERSON_AND_ORGANIZATION ( #70597, #27821 ) ;
#701 = CARTESIAN_POINT ( 'NONE',  ( -74.58953762381673869, -23.47596703998600276, 11.44779298504227683 ) ) ;
#702 = CARTESIAN_POINT ( 'NONE',  ( -130.5728709571500588, -23.56000036390797092, -1.497999999999531040 ) ) ;
#703 = CARTESIAN_POINT ( 'NONE',  ( -121.5573564770503481, -23.48786465467241769, 11.44779295918253759 ) ) ;
#704 = CARTESIAN_POINT ( 'NONE',  ( -100.5429575306527141, -25.04353918802791057, 7.561013281394894925 ) ) ;
#705 = CARTESIAN_POINT ( 'NONE',  ( 5.642884982650352654, -6.376774720514426065, 20.85668005806743608 ) ) ;
#706 = CARTESIAN_POINT ( 'NONE',  ( -129.5560488346142733, -23.73766607897671221, -1.055555164236443577 ) ) ;
#707 = B_SPLINE_CURVE_WITH_KNOTS ( 'NONE', 3,
 ( #87065, #79953, #96189, #10439 ),
 .UNSPECIFIED., .F., .F.,
 ( 4, 4 ),
 ( 0.000000000000000000, 9.999999999998897304E-05 ),
 .UNSPECIFIED. ) ;
#708 = CARTESIAN_POINT ( 'NONE',  ( -99.52609871227460303, -25.26400865036767485, 4.842596224614812428 ) ) ;
#709 = CARTESIAN_POINT ( 'NONE',  ( -19.77041435686880533, -2.435487021107205940, -1.500000000000002220 ) ) ;
#710 = CARTESIAN_POINT ( 'NONE',  ( 32.25249349869195470, 1.477225279485574028, -12.65342752644894553 ) ) ;
#711 = CARTESIAN_POINT ( 'NONE',  ( -17.21045110277357182, -9.822940424218707278, -1.500000000000002220 ) ) ;
#712 = CARTESIAN_POINT ( 'NONE',  ( 0.3908843598833069422, -5.876774720514419847, 20.63520656483649773 ) ) ;
#713 = CARTESIAN_POINT ( 'NONE',  ( -39.73251464975087544, -25.29116557167905555, 3.010156479320208689 ) ) ;
#714 = CIRCLE ( 'NONE', #18542, 2.249999999999998668 ) ;
#715 = CARTESIAN_POINT ( 'NONE',  ( 1.949999999999999956, -0.1925000000000007261, 0.1924999999999992828 ) ) ;
#716 = CARTESIAN_POINT ( 'NONE',  ( -15.27568272636907665, 14.01247568063241999, 11.49999999999999645 ) ) ;
#717 = CARTESIAN_POINT ( 'NONE',  ( -101.6228709571500701, -23.47596703998600631, 11.44779298504227683 ) ) ;
#718 = CARTESIAN_POINT ( 'NONE',  ( -106.6228709571500559, -24.66019654487199730, 8.947790411086122830 ) ) ;
#719 = CARTESIAN_POINT ( 'NONE',  ( 19.62911079104473444, -11.51699945595908758, 11.49999999999999645 ) ) ;
#721 = ADVANCED_FACE ( 'NONE', ( #54500 ), #56013, .F. ) ;
#720 = ORIENTED_EDGE ( 'NONE', *, *, #23043, .T. ) ;
#722 = CARTESIAN_POINT ( 'NONE',  ( -69.58785280780001870, -24.34968618360933945, 0.1864209137778826408 ) ) ;
#724 = EDGE_CURVE ( 'NONE', #36801, #45447, #208, .T. ) ;
#723 = LINE ( 'NONE', #93064, #9580 ) ;
#725 = ORIENTED_EDGE ( 'NONE', *, *, #42551, .T. ) ;
#726 = CARTESIAN_POINT ( 'NONE',  ( 12.43249465596513126, -15.92577207200969092, -1.500000000000002220 ) ) ;
#727 = LINE ( 'NONE', #23045, #75918 ) ;
#728 = EDGE_CURVE ( 'NONE', #23841, #79650, #27659, .T. ) ;
#729 = CARTESIAN_POINT ( 'NONE',  ( 30.09341516180546350, 1.477225279485574028, -11.39311774897855933 ) ) ;
#730 = ADVANCED_FACE ( 'NONE', ( #69730 ), #16418, .F. ) ;
#731 = ORIENTED_EDGE ( 'NONE', *, *, #77412, .T. ) ;
#732 = ADVANCED_FACE ( 'NONE', ( #15922 ), #55009, .F. ) ;
#733 = VERTEX_POINT ( 'NONE', #24036 ) ;
#734 = FACE_OUTER_BOUND ( 'NONE', #68634, .T. ) ;
#735 = CARTESIAN_POINT ( 'NONE',  ( 16.68310095749102118, 15.68496000196893370, 11.49999999999998934 ) ) ;
#736 = CARTESIAN_POINT ( 'NONE',  ( -50.90914965406638260, -25.27420588080167718, 3.408962287336470887 ) ) ;
#737 = CARTESIAN_POINT ( 'NONE',  ( 18.46943957830784555, -11.30625484363265265, -1.500000000000002220 ) ) ;
#738 = CARTESIAN_POINT ( 'NONE',  ( -36.62287095715006302, -23.72773821059535493, 11.05748984161097681 ) ) ;
#739 = CARTESIAN_POINT ( 'NONE',  ( 16.07097863352054290, 13.35096362007907622, 11.49999999999999645 ) ) ;
#740 = ORIENTED_EDGE ( 'NONE', *, *, #89907, .T. ) ;
#741 = EDGE_CURVE ( 'NONE', #6280, #91104, #48516, .T. ) ;
#742 = CARTESIAN_POINT ( 'NONE',  ( -73.52287095715007581, -23.48786465467241058, 11.44779295918254647 ) ) ;
#743 = CARTESIAN_POINT ( 'NONE',  ( -124.6238252180020396, -24.51314013834316086, 0.6176544820404203939 ) ) ;
#744 = CARTESIAN_POINT ( 'NONE',  ( -10.13730173486854369, -19.54584281717935568, 11.49999999999998934 ) ) ;
#745 = VECTOR ( 'NONE', #16065, 1000.000000000000114 ) ;
#746 = DIRECTION ( 'NONE',  ( -0.9848077530122087975, 0.1736481776669262789, 0.000000000000000000 ) ) ;
#747 = CARTESIAN_POINT ( 'NONE',  ( 16.26279755680690542, 1.684774720514426560, -27.67997040356620531 ) ) ;
#748 = ORIENTED_EDGE ( 'NONE', *, *, #93099, .F. ) ;
#749 = CARTESIAN_POINT ( 'NONE',  ( -49.59807878744301490, -25.18440185366671358, 3.677862597024960323 ) ) ;
#750 = DIRECTION ( 'NONE',  ( 1.286817348990133162E-16, 0.000000000000000000, -1.000000000000000000 ) ) ;
#751 = ORIENTED_EDGE ( 'NONE', *, *, #1684, .T. ) ;
#752 = CARTESIAN_POINT ( 'NONE',  ( -123.6228709571500701, -23.72773821059535848, 11.05748984161097503 ) ) ;
#753 = ORIENTED_EDGE ( 'NONE', *, *, #9909, .F. ) ;
#754 = EDGE_LOOP ( 'NONE', ( #42777, #20631, #2418, #87464 ) ) ;
#755 = CARTESIAN_POINT ( 'NONE',  ( -106.6228709571500985, -23.96127896941632329, -0.6493128931037804863 ) ) ;
#756 = LINE ( 'NONE', #77367, #21131 ) ;
#757 = CARTESIAN_POINT ( 'NONE',  ( -4.358143420448500116, -6.376774720514413630, 19.75705121608222115 ) ) ;
#758 = CARTESIAN_POINT ( 'NONE',  ( 4.362881659454829197, 20.01674633476859810, -1.500000000000002220 ) ) ;
#759 = EDGE_CURVE ( 'NONE', #82155, #14495, #100103, .T. ) ;
#760 = AXIS2_PLACEMENT_3D ( 'NONE', #34476, #5513, #96870 ) ;
#761 = ORIENTED_EDGE ( 'NONE', *, *, #9232, .T. ) ;
#762 = CARTESIAN_POINT ( 'NONE',  ( -71.62287095715004170, -24.51387760970724372, 9.387446482453425389 ) ) ;
#763 = CARTESIAN_POINT ( 'NONE',  ( -10.28806225508158612, 4.941275956067651798, 28.69510307482446976 ) ) ;
#764 = LINE ( 'NONE', #6878, #56406 ) ;
#765 = CARTESIAN_POINT ( 'NONE',  ( 10.93216147639808611, 19.43004700418156361, 11.49999999999998934 ) ) ;
#766 = B_SPLINE_CURVE_WITH_KNOTS ( 'NONE', 3,
 ( #71091, #41147, #3090, #48763, #55877, #78669 ),
 .UNSPECIFIED., .F., .F.,
 ( 4, 2, 4 ),
 ( 0.0004434240296263077972, 0.001023314793611319017, 0.001603205557596327959 ),
 .UNSPECIFIED. ) ;
#767 = CARTESIAN_POINT ( 'NONE',  ( -90.52287095715006160, -23.47593901973090524, -1.443836447538996426 ) ) ;
#768 = CARTESIAN_POINT ( 'NONE',  ( -1.649669150391666506, -5.876774720514411854, 19.67464842890028365 ) ) ;
#769 = EDGE_CURVE ( 'NONE', #68993, #8748, #86444, .T. ) ;
#770 = ORIENTED_EDGE ( 'NONE', *, *, #77456, .F. ) ;
#771 = CARTESIAN_POINT ( 'NONE',  ( -5.366453405989236813, -2.000000000000001776, 19.19609335255483984 ) ) ;
#772 = DIRECTION ( 'NONE',  ( 0.000000000000000000, 0.9999999999976377785, 2.173523156925979975E-06 ) ) ;
#773 = CARTESIAN_POINT ( 'NONE',  ( 15.94631523246878579, 13.42178585792578360, 11.49999999999998934 ) ) ;
#774 = ORIENTED_EDGE ( 'NONE', *, *, #31657, .T. ) ;
#777 = ORIENTED_EDGE ( 'NONE', *, *, #8668, .F. ) ;
#776 = EDGE_CURVE ( 'NONE', #85237, #35109, #65247, .T. ) ;
#775 = CARTESIAN_POINT ( 'NONE',  ( 8.160000000000000142, 9.789768006247301813, -0.8564937190954607926 ) ) ;
#778 = ORIENTED_EDGE ( 'NONE', *, *, #93642, .F. ) ;
#779 = CARTESIAN_POINT ( 'NONE',  ( -58.52287095715006160, -23.47596703998600631, 11.44779298504228926 ) ) ;
#780 = CARTESIAN_POINT ( 'NONE',  ( -13.85205798638896901, 15.75786377350088507, -1.500000000000002220 ) ) ;
#781 = ORIENTED_EDGE ( 'NONE', *, *, #1325, .T. ) ;
#782 = CARTESIAN_POINT ( 'NONE',  ( -69.52287095715007581, -23.73934037231756022, 11.05740245334329330 ) ) ;
#783 = DIRECTION ( 'NONE',  ( 6.030048488936326810E-14, 0.000000000000000000, -1.000000000000000000 ) ) ;
#784 = CARTESIAN_POINT ( 'NONE',  ( 11.32388168880214074, -5.356774720514423827, -25.00917421515942962 ) ) ;
#785 = CARTESIAN_POINT ( 'NONE',  ( -106.5228709571500758, -29.50248528299804818, 1.056150453629043584 ) ) ;
#786 = FACE_OUTER_BOUND ( 'NONE', #65075, .T. ) ;
#787 = CARTESIAN_POINT ( 'NONE',  ( -118.5228709571500758, -23.47596703998600631, 11.44779298504227860 ) ) ;
#789 = ORIENTED_EDGE ( 'NONE', *, *, #58186, .F. ) ;
#788 = CARTESIAN_POINT ( 'NONE',  ( 12.10043277420606778, 18.60588626676543100, 11.49999999999999645 ) ) ;
#790 = CARTESIAN_POINT ( 'NONE',  ( -44.52287095715006160, -29.50250786944525672, 11.44777988621624232 ) ) ;
#791 = CYLINDRICAL_SURFACE ( 'NONE', #74774, 1.699999999999999734 ) ;
#792 = ORIENTED_EDGE ( 'NONE', *, *, #8058, .T. ) ;
#793 = CARTESIAN_POINT ( 'NONE',  ( -22.46375958613465684, 3.124547546656453179, 11.49999999999998934 ) ) ;
#794 = EDGE_CURVE ( 'NONE', #47537, #59400, #86947, .T. ) ;
#796 = ORIENTED_EDGE ( 'NONE', *, *, #76715, .T. ) ;
#795 = DIRECTION ( 'NONE',  ( 0.000000000000000000, 0.000000000000000000, -1.000000000000000000 ) ) ;
#797 = EDGE_LOOP ( 'NONE', ( #41880, #27016, #53336, #74875 ) ) ;
#798 = VECTOR ( 'NONE', #16545, 1000.000000000000000 ) ;
#799 = DIRECTION ( 'NONE',  ( 0.000000000000000000, -0.9999999999976377785, -2.173523156925979975E-06 ) ) ;
#800 = ADVANCED_FACE ( 'NONE', ( #47892 ), #62620, .T. ) ;
#801 = CARTESIAN_POINT ( 'NONE',  ( 19.31759285448427477, -5.727529672960866236, -1.500000000000002220 ) ) ;
#802 = CARTESIAN_POINT ( 'NONE',  ( -80.62287095715004170, -24.63287334234178871, 0.9662140553045442948 ) ) ;
#803 = VERTEX_POINT ( 'NONE', #71229 ) ;
#804 = CARTESIAN_POINT ( 'NONE',  ( 31.79364159983995464, -5.965225279485572685, -11.59305536555894278 ) ) ;
#805 = CARTESIAN_POINT ( 'NONE',  ( -22.19192207843486386, -2.872123673023632584, -1.500000000000002220 ) ) ;
#806 = B_SPLINE_CURVE_WITH_KNOTS ( 'NONE', 3,
 ( #95087, #80363, #46546, #70382 ),
 .UNSPECIFIED., .F., .F.,
 ( 4, 4 ),
 ( 0.000000000000000000, 9.999999999998900014E-05 ),
 .UNSPECIFIED. ) ;
#807 = EDGE_CURVE ( 'NONE', #15795, #18354, #1717, .T. ) ;
#808 = ORIENTED_EDGE ( 'NONE', *, *, #72055, .T. ) ;
#809 = EDGE_LOOP ( 'NONE', ( #59193, #38629, #23114, #8310 ) ) ;
#810 = CYLINDRICAL_SURFACE ( 'NONE', #30356, 0.2499999999997798983 ) ;
#811 = CARTESIAN_POINT ( 'NONE',  ( -94.62789002903245716, -24.35071581493543036, 9.817618358456030592 ) ) ;
#812 = DIRECTION ( 'NONE',  ( 0.000000000000000000, 0.000000000000000000, -1.000000000000000000 ) ) ;
#813 = PLANE ( 'NONE',  #66018 ) ;
#814 = CARTESIAN_POINT ( 'NONE',  ( -63.93038602344318377, -24.37807914296826084, 0.3010598746230576661 ) ) ;
#815 = CARTESIAN_POINT ( 'NONE',  ( -5.392953615240748455, 18.82278424538476713, 11.49999999999998934 ) ) ;
#816 = CARTESIAN_POINT ( 'NONE',  ( -102.5228709571500616, -24.51283580621452884, 0.6167428607045936095 ) ) ;
#817 = ORIENTED_EDGE ( 'NONE', *, *, #100163, .F. ) ;
#818 = CARTESIAN_POINT ( 'NONE',  ( 8.645823604709390153, 19.67543227842514852, 11.49999999999998934 ) ) ;
#819 = CARTESIAN_POINT ( 'NONE',  ( -2.794793911895765870, -5.876774720514415407, 20.33046051580616265 ) ) ;
#820 = CARTESIAN_POINT ( 'NONE',  ( 22.02124265030973760, 7.743225279485574042, 13.95402280011862395 ) ) ;
#821 = CARTESIAN_POINT ( 'NONE',  ( -117.9228709571500673, -23.47593901973090524, -1.443836447538996426 ) ) ;
#822 = LINE ( 'NONE', #56131, #34201 ) ;
#824 = AXIS2_PLACEMENT_3D ( 'NONE', #32054, #1622, #63528 ) ;
#823 = CARTESIAN_POINT ( 'NONE',  ( 20.41593879258296695, -10.28030303932802880, -1.500000000000002220 ) ) ;
#825 = COORDINATED_UNIVERSAL_TIME_OFFSET ( 0, 0, .AHEAD. ) ;
#826 = FACE_OUTER_BOUND ( 'NONE', #14399, .T. ) ;
#827 = CARTESIAN_POINT ( 'NONE',  ( -70.83259324169414128, -25.30884602800411542, 5.409333232728893215 ) ) ;
#828 = CARTESIAN_POINT ( 'NONE',  ( 2.999408428739025023, -19.78128511538675127, 11.49999999999999645 ) ) ;
#829 = FACE_OUTER_BOUND ( 'NONE', #39415, .T. ) ;
#830 = CARTESIAN_POINT ( 'NONE',  ( -107.5228709571500758, -24.64898659630367916, 1.056161002820831474 ) ) ;
#831 = CARTESIAN_POINT ( 'NONE',  ( 22.81105451610979173, 8.475225279485572472, -17.31691820600746823 ) ) ;
#832 = DIRECTION ( 'NONE',  ( 0.000000000000000000, 1.000000000000000000, -1.571307496355802709E-16 ) ) ;
#833 = VERTEX_POINT ( 'NONE', #64644 ) ;
#834 = CARTESIAN_POINT ( 'NONE',  ( -24.90875734969025501, -3.316774720514426456, 26.43402280011862615 ) ) ;
#835 = VECTOR ( 'NONE', #24110, 1000.000000000000114 ) ;
#836 = CARTESIAN_POINT ( 'NONE',  ( -21.33044368757495590, -4.375833669458513597, -1.500000000000002220 ) ) ;
#837 = CARTESIAN_POINT ( 'NONE',  ( -117.5895376238167245, -23.48783264082479505, -1.443836473390058384 ) ) ;
#838 = CARTESIAN_POINT ( 'NONE',  ( 19.59260286812380514, -1.442238090573773501, -1.500000000000002220 ) ) ;
#839 = VECTOR ( 'NONE', #13846, 1000.000000000000114 ) ;
#840 = DIRECTION ( 'NONE',  ( -1.000000000000000000, -0.000000000000000000, -0.000000000000000000 ) ) ;
#841 = B_SPLINE_CURVE_WITH_KNOTS ( 'NONE', 3,
 ( #34192, #48421, #56038, #33689 ),
 .UNSPECIFIED., .F., .F.,
 ( 4, 4 ),
 ( 0.4007861916091369769, 0.4097926228812525662 ),
 .UNSPECIFIED. ) ;
#842 = CARTESIAN_POINT ( 'NONE',  ( -104.6228709571500559, -23.48786465467241413, 11.44779295918254114 ) ) ;
#843 = DATE_TIME_ROLE ( 'classification_date' ) ;
#844 = CARTESIAN_POINT ( 'NONE',  ( -91.58604265345489637, -24.51419770103159124, 9.386484678747176957 ) ) ;
#845 = DIRECTION ( 'NONE',  ( 0.000000000000000000, -1.000000000000000000, 0.000000000000000000 ) ) ;
#846 = CARTESIAN_POINT ( 'NONE',  ( -0.1859688948871585645, 20.53422428922035081, 11.49999999999999645 ) ) ;
#847 = DIRECTION ( 'NONE',  ( 0.000000000000000000, 2.173523156925980399E-06, -0.9999999999976378895 ) ) ;
#848 = CARTESIAN_POINT ( 'NONE',  ( -120.5186651893930332, -24.40034930558991633, 0.3402023900116107336 ) ) ;
#849 = CARTESIAN_POINT ( 'NONE',  ( 3.115699594417459473, -22.39947108414558485, 11.49999999999999645 ) ) ;
#850 = ORIENTED_EDGE ( 'NONE', *, *, #79432, .T. ) ;
#851 =( NAMED_UNIT ( * ) SI_UNIT ( $, .STERADIAN. ) SOLID_ANGLE_UNIT ( ) );
#852 = ADVANCED_FACE ( 'NONE', ( #2225 ), #99180, .T. ) ;
#853 = CARTESIAN_POINT ( 'NONE',  ( -99.53249707683190195, -25.26387314544760798, 4.095394624650092297 ) ) ;
#854 = CARTESIAN_POINT ( 'NONE',  ( -37.52287095715009713, -24.33832256527048798, 0.1851278514138569864 ) ) ;
#856 = ADVANCED_FACE ( 'NONE', ( #96063 ), #49405, .F. ) ;
#855 = CARTESIAN_POINT ( 'NONE',  ( -125.6246426838371661, -24.40133493613050675, 9.663955038902798833 ) ) ;
#857 = CARTESIAN_POINT ( 'NONE',  ( -85.62287095715004170, -24.83602698348159166, 1.605859176311267955 ) ) ;
#858 = EDGE_CURVE ( 'NONE', #31747, #84710, #60382, .T. ) ;
#859 = CARTESIAN_POINT ( 'NONE',  ( -33.62287095715004881, -24.50216790748205042, 0.6166512839542545033 ) ) ;
#860 = ADVANCED_FACE ( 'NONE', ( #87444 ), #66138, .T. ) ;
#861 = CARTESIAN_POINT ( 'NONE',  ( -2.794871794871795156, -6.376774720514417183, 20.36318108974359475 ) ) ;
#862 = EDGE_CURVE ( 'NONE', #94971, #29990, #58017, .T. ) ;
#863 = ORIENTED_EDGE ( 'NONE', *, *, #769, .F. ) ;
#864 = CARTESIAN_POINT ( 'NONE',  ( -20.32320236877023589, 10.94715076914730290, 11.49999999999999645 ) ) ;
#865 = CARTESIAN_POINT ( 'NONE',  ( 22.20583189720066741, -5.198064566299082756, 11.49999999999998934 ) ) ;
#866 = CARTESIAN_POINT ( 'NONE',  ( -74.59223927811392230, -24.15543982623907127, -0.2315651400026650930 ) ) ;
#867 = CARTESIAN_POINT ( 'NONE',  ( -115.5228709571500758, -23.84081130425358097, 10.88220057483157888 ) ) ;
#868 = CARTESIAN_POINT ( 'NONE',  ( -57.52287095715007581, -23.72747288104470087, -1.053458166803227014 ) ) ;
#869 = AXIS2_PLACEMENT_3D ( 'NONE', #18946, #2744, #41811 ) ;
#870 = CARTESIAN_POINT ( 'NONE',  ( 21.67916507323446496, -5.852930566066080864, 11.49999999999999645 ) ) ;
#871 = VERTEX_POINT ( 'NONE', #10823 ) ;
#872 = CARTESIAN_POINT ( 'NONE',  ( -84.52287095715006160, -23.72747288104470087, -1.053458166803226126 ) ) ;
#873 = CARTESIAN_POINT ( 'NONE',  ( -43.52287095715008292, -24.33927499327853639, 9.819080762295813614 ) ) ;
#874 = CARTESIAN_POINT ( 'NONE',  ( 21.59112034314636119, 3.954845139028329015, 11.49999999999998934 ) ) ;
#875 = CARTESIAN_POINT ( 'NONE',  ( -5.596556251055551101, -5.876774720514411854, 19.35667676486397681 ) ) ;
#876 = CARTESIAN_POINT ( 'NONE',  ( -44.48278020699296320, -24.66019654487199020, 8.947790411086115725 ) ) ;
#877 = DIRECTION ( 'NONE',  ( -3.773278334444167608E-23, 1.000000000000000000, 0.000000000000000000 ) ) ;
#878 = EDGE_LOOP ( 'NONE', ( #26481, #100063 ) ) ;
#879 = CARTESIAN_POINT ( 'NONE',  ( -112.5228709571500616, -23.48786465467241769, 11.44779295918253936 ) ) ;
#880 = CARTESIAN_POINT ( 'NONE',  ( -66.62287095715005592, -29.50247984919015209, -1.443849546365055359 ) ) ;
#881 = VERTEX_POINT ( 'NONE', #41793 ) ;
#882 = CARTESIAN_POINT ( 'NONE',  ( -12.74120943341865342, -16.01528480738631899, -1.500000000000002220 ) ) ;
#883 = EDGE_LOOP ( 'NONE', ( #19897, #19757, #32178, #74503 ) ) ;
#884 = VERTEX_POINT ( 'NONE', #79824 ) ;
#885 = ORIENTED_EDGE ( 'NONE', *, *, #55746, .F. ) ;
#886 = ORIENTED_EDGE ( 'NONE', *, *, #84728, .F. ) ;
#887 = CARTESIAN_POINT ( 'NONE',  ( -3.381418692465893105, -22.81955385325859709, -1.500000000000002220 ) ) ;
#888 = CARTESIAN_POINT ( 'NONE',  ( -112.5228709571500758, -24.35013146730204170, 9.818937971375092388 ) ) ;
#889 = CARTESIAN_POINT ( 'NONE',  ( 2.300710779914242110, 20.15441874099239783, -1.500000000000002220 ) ) ;
#890 = ORIENTED_EDGE ( 'NONE', *, *, #15558, .F. ) ;
#891 = CARTESIAN_POINT ( 'NONE',  ( 6.660000000000001030, -10.15233964170348457, -1.303165529866009420 ) ) ;
#892 = CARTESIAN_POINT ( 'NONE',  ( -92.54440427696837901, -24.65952944569304961, 1.056160979905703901 ) ) ;
#893 = CARTESIAN_POINT ( 'NONE',  ( -40.22287095715006444, -23.47596703998600276, 11.44779298504227683 ) ) ;
#894 = CARTESIAN_POINT ( 'NONE',  ( 3.903461913076534451, -6.376774720514404748, 18.52532880998198905 ) ) ;
#896 = VERTEX_POINT ( 'NONE', #88950 ) ;
#895 = CARTESIAN_POINT ( 'NONE',  ( 21.44729954461699251, -1.519088741117538000, 11.49999999999999645 ) ) ;
#897 = CARTESIAN_POINT ( 'NONE',  ( -75.53432955309628483, -25.00158670708910691, 2.256160236439223699 ) ) ;
#898 = CARTESIAN_POINT ( 'NONE',  ( -61.50934325614997533, -23.96169478059712787, 10.65365249895718591 ) ) ;
#899 = ORIENTED_EDGE ( 'NONE', *, *, #89411, .F. ) ;
#900 = CARTESIAN_POINT ( 'NONE',  ( 14.61947915221463923, 14.71393552341326760, 11.49999999999998934 ) ) ;
#901 = AXIS2_PLACEMENT_3D ( 'NONE', #66757, #28172, #59131 ) ;
#902 = ORIENTED_EDGE ( 'NONE', *, *, #44602, .F. ) ;
#904 = ORIENTED_EDGE ( 'NONE', *, *, #47832, .F. ) ;
#903 = CARTESIAN_POINT ( 'NONE',  ( -91.58953762381672448, -24.64898659630368627, 1.056161002820390937 ) ) ;
#905 = VECTOR ( 'NONE', #69263, 1000.000000000000227 ) ;
#906 = CARTESIAN_POINT ( 'NONE',  ( -111.6258004380657667, -24.35071581493544457, 9.817618358456018157 ) ) ;
#907 = DIRECTION ( 'NONE',  ( -1.000000000000000000, 0.000000000000000000, -4.956352788505167212E-16 ) ) ;
#908 = VERTEX_POINT ( 'NONE', #11817 ) ;
#909 = VERTEX_POINT ( 'NONE', #3236 ) ;
#910 = CARTESIAN_POINT ( 'NONE',  ( -5.850750514176234596, -5.876774720514412742, 19.74039977944280366 ) ) ;
#911 = CARTESIAN_POINT ( 'NONE',  ( -42.58700419767085776, -24.35071581493543036, 9.817618358456037697 ) ) ;
#912 = AXIS2_PLACEMENT_3D ( 'NONE', #19260, #5043, #27389 ) ;
#913 = CARTESIAN_POINT ( 'NONE',  ( -4.929522925832171332, 6.376774720514426953, -28.63504101147569614 ) ) ;
#914 = CARTESIAN_POINT ( 'NONE',  ( -20.57682416348112397, 7.868404785394932155, 11.49999999999999645 ) ) ;
#915 = VECTOR ( 'NONE', #18164, 1000.000000000000000 ) ;
#916 = CARTESIAN_POINT ( 'NONE',  ( -89.51147662468558508, -24.15620529776628445, 10.23563542870660115 ) ) ;
#917 = CARTESIAN_POINT ( 'NONE',  ( -22.55165446212525993, 1.111233042438415808, 11.49999999999998934 ) ) ;
#918 = AXIS2_PLACEMENT_3D ( 'NONE', #95863, #26357, #9125 ) ;
#919 = CARTESIAN_POINT ( 'NONE',  ( 16.07406896385161943, -13.52096256729613266, -1.500000000000002220 ) ) ;
#920 = CARTESIAN_POINT ( 'NONE',  ( 6.727829057902616761, -6.376774720514417183, 20.13865202822440281 ) ) ;
#922 = VERTEX_POINT ( 'NONE', #41276 ) ;
#921 = CARTESIAN_POINT ( 'NONE',  ( 0.000000000000000000, 4.772774720514425972, 0.000000000000000000 ) ) ;
#923 = VERTEX_POINT ( 'NONE', #72230 ) ;
#924 = CARTESIAN_POINT ( 'NONE',  ( -59.62287095715004170, -23.72773821059535848, 11.05748984161097503 ) ) ;
#925 = EDGE_CURVE ( 'NONE', #37824, #10565, #2724, .T. ) ;
#926 = EDGE_CURVE ( 'NONE', #39625, #82409, #57518, .T. ) ;
#927 = CARTESIAN_POINT ( 'NONE',  ( -113.6228709571500559, -24.64965695001469115, 8.947790433994176951 ) ) ;
#928 = ORIENTED_EDGE ( 'NONE', *, *, #10258, .T. ) ;
#929 = CARTESIAN_POINT ( 'NONE',  ( 18.68757921870947669, -9.911485057863893999, -1.500000000000002220 ) ) ;
#930 = CARTESIAN_POINT ( 'NONE',  ( 27.53860345374808105, 1.477225279485574028, 19.84760796525321425 ) ) ;
#931 = CARTESIAN_POINT ( 'NONE',  ( -51.93149462243456327, -25.03148440107001349, 6.174051623307587278 ) ) ;
#932 = PLANE ( 'NONE',  #63196 ) ;
#933 = LINE ( 'NONE', #45613, #45946 ) ;
#934 = CARTESIAN_POINT ( 'NONE',  ( 1.000208336950358934, 2.877919977996279334E-16, -2.349999999999999645 ) ) ;
#935 = CARTESIAN_POINT ( 'NONE',  ( -19.06252244145942498, 11.34236556261432405, -1.500000000000002220 ) ) ;
#936 = CARTESIAN_POINT ( 'NONE',  ( -8.094297649259210914, -10.08546205824535669, 1.310587897985993955 ) ) ;
#937 = VERTEX_POINT ( 'NONE', #35666 ) ;
#938 = CARTESIAN_POINT ( 'NONE',  ( -51.44679290749079570, -25.24860047834440380, 5.195306865420171505 ) ) ;
#939 = CARTESIAN_POINT ( 'NONE',  ( -37.50486701413690582, -23.96119346886880663, -0.6495511937831990323 ) ) ;
#940 = CARTESIAN_POINT ( 'NONE',  ( -40.41248649115142655, -25.30361164129646667, 5.542177216901341907 ) ) ;
#941 = CARTESIAN_POINT ( 'NONE',  ( -37.52287095715006870, -29.50250243563736774, 8.947779886222148704 ) ) ;
#942 = CARTESIAN_POINT ( 'NONE',  ( -33.62287095715005592, -24.64965695001467694, 8.947790433994189385 ) ) ;
#943 = CARTESIAN_POINT ( 'NONE',  ( -3.206006181753352724, -19.19236486397402430, 11.49999999999998934 ) ) ;
#944 = VECTOR ( 'NONE', #15821, 1000.000000000000114 ) ;
#945 = CARTESIAN_POINT ( 'NONE',  ( 19.99361899508246765, -7.638522130635823082, 11.49999999999998934 ) ) ;
#946 = CARTESIAN_POINT ( 'NONE',  ( -17.66201745896767505, -0.3587747205144061202, -23.06272557202527906 ) ) ;
#947 = CARTESIAN_POINT ( 'NONE',  ( -60.53567020741864013, -24.73531770709804078, 8.716586749031112191 ) ) ;
#948 = B_SPLINE_CURVE_WITH_KNOTS ( 'NONE', 3,
 ( #77472, #76473, #31821, #61779 ),
 .UNSPECIFIED., .F., .F.,
 ( 4, 4 ),
 ( 0.000000000000000000, 0.0001000000000000167422 ),
 .UNSPECIFIED. ) ;
#949 = DIRECTION ( 'NONE',  ( 0.000000000000000000, 0.000000000000000000, 1.000000000000000000 ) ) ;
#950 = DIRECTION ( 'NONE',  ( -3.773278334453079618E-23, 0.9999999999976377785, 2.173523156925979975E-06 ) ) ;
#951 = CARTESIAN_POINT ( 'NONE',  ( 7.379361219544559702, 21.46082085352547963, -1.500000000000002220 ) ) ;
#952 = LINE ( 'NONE', #47638, #10957 ) ;
#953 = CARTESIAN_POINT ( 'NONE',  ( -101.7776484685884242, -29.50249165161862663, 3.986241424695394109 ) ) ;
#954 = CARTESIAN_POINT ( 'NONE',  ( -11.18921147948170614, -16.41150865552512883, 11.49999999999999645 ) ) ;
#955 = CARTESIAN_POINT ( 'NONE',  ( 5.327901167172695907, -6.376774720514418959, 20.73192761314082233 ) ) ;
#956 = CARTESIAN_POINT ( 'NONE',  ( -115.5562042904833930, -23.47596703998600631, 11.44779298504227683 ) ) ;
#957 = CYLINDRICAL_SURFACE ( 'NONE', #40692, 15.00000000000000178 ) ;
#958 = ORIENTED_EDGE ( 'NONE', *, *, #76806, .T. ) ;
#959 = CARTESIAN_POINT ( 'NONE',  ( 30.53060340732035982, 4.594240983522013266, 19.84760796525321780 ) ) ;
#960 = CARTESIAN_POINT ( 'NONE',  ( -6.720452724358975338, -5.876774720514411854, 19.46153846153846700 ) ) ;
#961 = FACE_OUTER_BOUND ( 'NONE', #23845, .T. ) ;
#962 = CARTESIAN_POINT ( 'NONE',  ( -10.61912389536305490, -18.88692380039396213, -1.500000000000002220 ) ) ;
#963 = CARTESIAN_POINT ( 'NONE',  ( -32.52287095715003318, -24.66019654487198665, 8.947790411086131712 ) ) ;
#964 = CARTESIAN_POINT ( 'NONE',  ( 19.19537281719634336, 3.394423509666608663, -1.500000000000002220 ) ) ;
#965 = CARTESIAN_POINT ( 'NONE',  ( -55.62373614600970484, -25.00182538069146432, 7.747789668545041586 ) ) ;
#966 = ADVANCED_FACE ( 'NONE', ( #4713 ), #44278, .F. ) ;
#967 = B_SPLINE_CURVE_WITH_KNOTS ( 'NONE', 3,
 ( #57525, #87455, #75217, #13308, #59017, #73728 ),
 .UNSPECIFIED., .F., .F.,
 ( 4, 2, 4 ),
 ( 0.000000000000000000, 0.001381509804613668827, 0.002763019609227337654 ),
 .UNSPECIFIED. ) ;
#968 = ORIENTED_EDGE ( 'NONE', *, *, #28936, .T. ) ;
#969 = CARTESIAN_POINT ( 'NONE',  ( -17.41452279269062586, 10.58001483151439004, 11.49999999999999645 ) ) ;
#970 = CARTESIAN_POINT ( 'NONE',  ( -75.62287095715005592, -29.50248528299804818, 1.056150453629038477 ) ) ;
#971 = AXIS2_PLACEMENT_3D ( 'NONE', #59783, #12083, #52157 ) ;
#972 = CARTESIAN_POINT ( 'NONE',  ( -112.5228709571500616, -29.50248528299804818, 1.056150453629043584 ) ) ;
#973 = ORIENTED_EDGE ( 'NONE', *, *, #55206, .F. ) ;
#974 = CARTESIAN_POINT ( 'NONE',  ( -30.62155233649868791, -24.14929313691196455, 10.49653219292474482 ) ) ;
#975 = DIRECTION ( 'NONE',  ( 0.000000000000000000, 2.173523156925980399E-06, -0.9999999999976378895 ) ) ;
#976 = CARTESIAN_POINT ( 'NONE',  ( -48.92504535501358021, -25.25214610244555402, 5.781339582145927025 ) ) ;
#977 = VECTOR ( 'NONE', #82147, 1000.000000000000000 ) ;
#978 = EDGE_CURVE ( 'NONE', #73446, #63682, #95404, .T. ) ;
#979 = CARTESIAN_POINT ( 'NONE',  ( -40.46892088308801050, -25.00182538069146432, 7.747789668545040698 ) ) ;
#980 = CARTESIAN_POINT ( 'NONE',  ( -1.022535880784302353, -6.376774720514415407, 19.99258394656883908 ) ) ;
#981 = CARTESIAN_POINT ( 'NONE',  ( 15.17442925503088169, 13.16703847180013831, -1.500000000000002220 ) ) ;
#982 = CARTESIAN_POINT ( 'NONE',  ( -109.5222136733952425, -23.48783264082476663, -1.443836473390089692 ) ) ;
#984 = ORIENTED_EDGE ( 'NONE', *, *, #31906, .F. ) ;
#983 = EDGE_CURVE ( 'NONE', #84470, #85538, #62713, .T. ) ;
#985 = FACE_OUTER_BOUND ( 'NONE', #37343, .T. ) ;
#986 = CIRCLE ( 'NONE', #64243, 28.96799999999999287 ) ;
#987 = EDGE_CURVE ( 'NONE', #54720, #90018, #13072, .T. ) ;
#988 = B_SPLINE_CURVE_WITH_KNOTS ( 'NONE', 3,
 ( #63516, #24426, #84820, #46266, #93, #55901 ),
 .UNSPECIFIED., .F., .F.,
 ( 4, 2, 4 ),
 ( 6.384118678609355280E-06, 0.001386860460828372816, 0.002767336802978136254 ),
 .UNSPECIFIED. ) ;
#989 = CARTESIAN_POINT ( 'NONE',  ( -16.74478417649319084, -15.65585335247391896, 11.49999999999999645 ) ) ;
#990 = CARTESIAN_POINT ( 'NONE',  ( -22.17926634000774655, 4.976981427743210951, -1.500000000000002220 ) ) ;
#991 = VERTEX_POINT ( 'NONE', #66636 ) ;
#992 = CARTESIAN_POINT ( 'NONE',  ( -53.62287095715004881, -23.48786465467241058, 11.44779295918255002 ) ) ;
#993 = EDGE_CURVE ( 'NONE', #81513, #4283, #67618, .T. ) ;
#994 = FACE_OUTER_BOUND ( 'NONE', #44526, .T. ) ;
#995 = CARTESIAN_POINT ( 'NONE',  ( -38.60080858671575044, -23.96169478059712432, 10.65365249895718591 ) ) ;
#996 = EDGE_CURVE ( 'NONE', #93569, #23708, #38610, .T. ) ;
#997 = CARTESIAN_POINT ( 'NONE',  ( -30.57287095715006231, -24.76473628883709210, 8.626942252220645813 ) ) ;
#998 = DIRECTION ( 'NONE',  ( 0.7512896232465891000, 0.000000000000000000, 0.6599726524652351767 ) ) ;
#999 = LINE ( 'NONE', #16714, #29049 ) ;
#1000 = ORIENTED_EDGE ( 'NONE', *, *, #17276, .T. ) ;
#1001 = CARTESIAN_POINT ( 'NONE',  ( 4.102729645046709450, 19.96921287702725323, -1.500000000000002220 ) ) ;
#1002 = EDGE_LOOP ( 'NONE', ( #73125, #62557, #56487, #47720 ) ) ;
#1003 = B_SPLINE_CURVE_WITH_KNOTS ( 'NONE', 3,
 ( #3545, #34489, #96382, #65465 ),
 .UNSPECIFIED., .F., .F.,
 ( 4, 4 ),
 ( 0.3990514020202980405, 0.4000521490610636222 ),
 .UNSPECIFIED. ) ;
#1004 = ADVANCED_FACE ( 'NONE', ( #59498 ), #12802, .F. ) ;
#1005 = CARTESIAN_POINT ( 'NONE',  ( -22.94451526424785115, -1.264959178018935315, 11.49999999999998934 ) ) ;
#1006 = CARTESIAN_POINT ( 'NONE',  ( -7.294102189209645815, -5.876774720514413630, 19.89644244529368677 ) ) ;
#1007 = CARTESIAN_POINT ( 'NONE',  ( -54.54770071756311722, -24.15620529776628089, 10.23563542870661180 ) ) ;
#1008 = ORIENTED_EDGE ( 'NONE', *, *, #52103, .F. ) ;
#1009 = AXIS2_PLACEMENT_3D ( 'NONE', #6067, #84185, #60383 ) ;
#1010 = CARTESIAN_POINT ( 'NONE',  ( -114.5228709571500332, -23.73934037231757443, 11.05740245334327909 ) ) ;
#1011 = CARTESIAN_POINT ( 'NONE',  ( -53.63292963077573461, -24.35071581493542681, 9.817618358456032368 ) ) ;
#1013 = ORIENTED_EDGE ( 'NONE', *, *, #9905, .F. ) ;
#1012 = CARTESIAN_POINT ( 'NONE',  ( 14.64190796094839264, -15.47823801613018269, 11.49999999999999645 ) ) ;
#1014 = EDGE_LOOP ( 'NONE', ( #26843, #62311, #71409, #34493 ) ) ;
#1015 = CARTESIAN_POINT ( 'NONE',  ( -21.61287440533560300, 5.199345243644041936, 11.49999999999998934 ) ) ;
#1016 = CARTESIAN_POINT ( 'NONE',  ( 19.39950376024442846, -7.079068461131618584, -1.500000000000002220 ) ) ;
#1017 = ORIENTED_EDGE ( 'NONE', *, *, #45920, .T. ) ;
#1018 = CARTESIAN_POINT ( 'NONE',  ( -112.6228709571500275, -23.72773821059535493, 11.05748984161097503 ) ) ;
#1019 = CARTESIAN_POINT ( 'NONE',  ( -95.59439228026970170, -24.15602025860896163, 10.28564288303536856 ) ) ;
#1020 = VERTEX_POINT ( 'NONE', #99033 ) ;
#1021 = CARTESIAN_POINT ( 'NONE',  ( -65.55620429048339304, -25.00158670708909625, 2.256160236439165967 ) ) ;
#1022 = ORIENTED_EDGE ( 'NONE', *, *, #35675, .F. ) ;
#1023 = LINE ( 'NONE', #62942, #83670 ) ;
#1024 = DIRECTION ( 'NONE',  ( 0.6177208787939497681, 0.000000000000000000, 0.7863974287229267279 ) ) ;
#1025 = CARTESIAN_POINT ( 'NONE',  ( -0.8937202392249329330, 20.86669477224961256, -1.500000000000002220 ) ) ;
#1027 = ADVANCED_FACE ( 'NONE', ( #74222 ), #19924, .F. ) ;
#1026 = CARTESIAN_POINT ( 'NONE',  ( -20.50126671893153940, -7.481214725051755110, 11.49999999999999645 ) ) ;
#1028 = LINE ( 'NONE', #84756, #39864 ) ;
#1029 = LINE ( 'NONE', #92367, #64525 ) ;
#1030 = CARTESIAN_POINT ( 'NONE',  ( 3.503984654965784706, -22.18958196551723816, -1.500000000000002220 ) ) ;
#1031 = VECTOR ( 'NONE', #20783, 1000.000000000000114 ) ;
#1032 = CARTESIAN_POINT ( 'NONE',  ( -118.5523285634779285, -24.66019654487199730, 8.947790411086115725 ) ) ;
#1033 = EDGE_CURVE ( 'NONE', #57047, #32034, #87223, .T. ) ;
#1034 = CARTESIAN_POINT ( 'NONE',  ( 33.74607884027702909, 0.3587747205144265483, -4.999864028243830916 ) ) ;
#1035 = CARTESIAN_POINT ( 'NONE',  ( 4.819673832743241348, -5.876774720514421624, 21.07066438048017076 ) ) ;
#1036 = EDGE_LOOP ( 'NONE', ( #90357, #82914, #11882, #85657 ) ) ;
#1037 = B_SPLINE_CURVE_WITH_KNOTS ( 'NONE', 3,
 ( #83711, #77090, #7589, #22297, #6590, #13190, #44164, #53277 ),
 .UNSPECIFIED., .F., .F.,
 ( 4, 2, 2, 4 ),
 ( -0.001240666984356056379, -0.0002401179793396601269, 0.0007604310256767361255, 0.002761529035709532100 ),
 .UNSPECIFIED. ) ;
#1038 = ORIENTED_EDGE ( 'NONE', *, *, #61912, .F. ) ;
#1039 = ORIENTED_EDGE ( 'NONE', *, *, #99470, .T. ) ;
#1040 = B_SPLINE_CURVE_WITH_KNOTS ( 'NONE', 3,
 ( #7269, #70178, #76768, #9271 ),
 .UNSPECIFIED., .F., .F.,
 ( 4, 4 ),
 ( 0.001505373688938434684, 0.001772001984008341434 ),
 .UNSPECIFIED. ) ;
#1041 = EDGE_CURVE ( 'NONE', #71460, #94222, #85959, .T. ) ;
#1042 = EDGE_LOOP ( 'NONE', ( #24675, #4803, #49008, #11806 ) ) ;
#1043 = VECTOR ( 'NONE', #77178, 1000.000000000000114 ) ;
#1044 = CARTESIAN_POINT ( 'NONE',  ( 9.194277187580093269, -19.27880637823015419, -1.500000000000002220 ) ) ;
#1046 = EDGE_CURVE ( 'NONE', #8729, #14476, #30027, .T. ) ;
#1045 = CARTESIAN_POINT ( 'NONE',  ( -22.19192207843486386, -2.872123673023632584, 11.49999999999999645 ) ) ;
#1047 = EDGE_LOOP ( 'NONE', ( #92275, #38229, #66850, #54927 ) ) ;
#1048 = VECTOR ( 'NONE', #3635, 1000.000000000000114 ) ;
#1049 = CARTESIAN_POINT ( 'NONE',  ( -1.165634184549018126, -21.02984315360824752, 11.49999999999998934 ) ) ;
#1050 = CARTESIAN_POINT ( 'NONE',  ( -30.60107339264236259, -24.67525583858868643, 1.095666116063849449 ) ) ;
#1051 = CARTESIAN_POINT ( 'NONE',  ( 13.74685606122050885, 14.44317598224977672, -1.500000000000002220 ) ) ;
#1052 = CARTESIAN_POINT ( 'NONE',  ( 22.81105451610979173, 1.684774720501991618, -20.71691820600746681 ) ) ;
#1053 = VECTOR ( 'NONE', #44095, 1000.000000000000000 ) ;
#1054 = CARTESIAN_POINT ( 'NONE',  ( 3.025806405283164136, -6.376774720514420736, 20.84867811309776542 ) ) ;
#1055 = CARTESIAN_POINT ( 'NONE',  ( -21.79611004543898289, 2.820803583321412678, -1.500000000000002220 ) ) ;
#1056 = CARTESIAN_POINT ( 'NONE',  ( -87.52287095714999055, -23.94994826722564696, -0.6494450866342719175 ) ) ;
#1057 = ORIENTED_EDGE ( 'NONE', *, *, #25862, .T. ) ;
#1058 = DIRECTION ( 'NONE',  ( -1.000000000000000000, 8.503546450866701308E-16, 0.000000000000000000 ) ) ;
#1059 = DIRECTION ( 'NONE',  ( -3.773278334453079030E-23, 0.9999999999976377785, 2.173523156925979128E-06 ) ) ;
#1060 = CARTESIAN_POINT ( 'NONE',  ( 18.01467621842780176, -10.50282939286117667, 11.49999999999999645 ) ) ;
#1061 = VECTOR ( 'NONE', #9585, 1000.000000000000000 ) ;
#1062 = CARTESIAN_POINT ( 'NONE',  ( 29.72095141006403196, -6.296447751620394939, 26.96056093718771152 ) ) ;
#1063 = FACE_OUTER_BOUND ( 'NONE', #36465, .T. ) ;
#1064 = CARTESIAN_POINT ( 'NONE',  ( -117.5228709571500616, -23.73907113216989728, -1.053371485793242357 ) ) ;
#1065 = CARTESIAN_POINT ( 'NONE',  ( 3.515848477382193416, 21.04717058667041130, 11.49999999999998934 ) ) ;
#1066 = DIRECTION ( 'NONE',  ( -1.000000000000000000, -3.773278334444167608E-23, -8.201307833595939069E-29 ) ) ;
#1067 = CARTESIAN_POINT ( 'NONE',  ( -117.5228709571500758, -24.51387760970726504, 9.387446482453405849 ) ) ;
#1068 = DIRECTION ( 'NONE',  ( 0.000000000000000000, 0.000000000000000000, -1.000000000000000000 ) ) ;
#1069 = DIRECTION ( 'NONE',  ( 0.000000000000000000, 0.000000000000000000, -1.000000000000000000 ) ) ;
#1070 = CC_DESIGN_PERSON_AND_ORGANIZATION_ASSIGNMENT ( #71725, #64639, ( #71682 ) ) ;
#1071 = CARTESIAN_POINT ( 'NONE',  ( -1.585881643086899606, 22.48459252949185228, -1.500000000000002220 ) ) ;
#1072 = FACE_OUTER_BOUND ( 'NONE', #12168, .T. ) ;
#1073 = EDGE_LOOP ( 'NONE', ( #75781, #8008, #64546, #16292 ) ) ;
#1074 = CARTESIAN_POINT ( 'NONE',  ( -51.52532898735692868, -25.26458355271423528, 6.117596087636846036 ) ) ;
#1075 = CARTESIAN_POINT ( 'NONE',  ( -31.49622502664552215, -24.15620529776627379, 10.23563542870661536 ) ) ;
#1076 = CARTESIAN_POINT ( 'NONE',  ( -16.08770303010339831, 11.32657509950784736, 11.49999999999999645 ) ) ;
#1077 = CARTESIAN_POINT ( 'NONE',  ( -28.62287095715006657, -24.50666107542846461, 1.056161637124864550 ) ) ;
#1078 = DIRECTION ( 'NONE',  ( -0.000000000000000000, 0.000000000000000000, -1.000000000000000000 ) ) ;
#1079 = ORIENTED_EDGE ( 'NONE', *, *, #35575, .T. ) ;
#1080 = CARTESIAN_POINT ( 'NONE',  ( -99.51411512703360529, -24.15543982623907837, -0.2315651400026449425 ) ) ;
#1081 = CARTESIAN_POINT ( 'NONE',  ( -59.52287095715006160, -24.64965694238407323, 8.947790433994201820 ) ) ;
#1082 = CARTESIAN_POINT ( 'NONE',  ( -2.794871794871791604, -6.376774720514427841, 21.75000000000001066 ) ) ;
#1083 = B_SPLINE_CURVE_WITH_KNOTS ( 'NONE', 3,
 ( #84838, #100040, #85334, #8226, #70121, #30551, #38664, #92444 ),
 .UNSPECIFIED., .F., .F.,
 ( 4, 2, 2, 4 ),
 ( -0.001240355328177004729, -0.0002398155169400588947, 0.0007607242942968869392, 0.002761803916770778390 ),
 .UNSPECIFIED. ) ;
#1084 = AXIS2_PLACEMENT_3D ( 'NONE', #98728, #67807, #14988 ) ;
#1085 = DIRECTION ( 'NONE',  ( 0.000000000000000000, 0.000000000000000000, -1.000000000000000000 ) ) ;
#1086 = CARTESIAN_POINT ( 'NONE',  ( 0.5484783294719396407, -19.75002165935583776, 11.49999999999998934 ) ) ;
#1087 = ORIENTED_EDGE ( 'NONE', *, *, #72726, .T. ) ;
#1088 = VECTOR ( 'NONE', #73324, 1000.000000000000114 ) ;
#1089 = CARTESIAN_POINT ( 'NONE',  ( -120.5228709571500048, -23.85229601348996198, 10.88205029486208097 ) ) ;
#1090 = DATE_TIME_ROLE ( 'classification_date' ) ;
#1091 = EDGE_LOOP ( 'NONE', ( #49889, #307, #15501, #45982, #27971, #95161, #30577, #51579 ) ) ;
#1092 = DIRECTION ( 'NONE',  ( -0.9913618264504691080, -4.164321980682960499E-15, 0.1311553622875927805 ) ) ;
#1093 = CARTESIAN_POINT ( 'NONE',  ( -107.6228709571500701, -24.65952944569304961, 1.056160979905703901 ) ) ;
#1094 = CARTESIAN_POINT ( 'NONE',  ( -100.4304529591284307, -25.30235285477424867, 4.722036383736525345 ) ) ;
#1095 = FACE_OUTER_BOUND ( 'NONE', #14726, .T. ) ;
#1096 = LINE ( 'NONE', #22405, #90649 ) ;
#1097 = CARTESIAN_POINT ( 'NONE',  ( -41.52287095715005449, -24.66019654487198665, 8.947790411086121054 ) ) ;
#1098 = CARTESIAN_POINT ( 'NONE',  ( 0.1645010273463769490, 0.3687607960183755251, -1.417169167140624575 ) ) ;
#1100 = EDGE_CURVE ( 'NONE', #65855, #79408, #1096, .T. ) ;
#1099 = CARTESIAN_POINT ( 'NONE',  ( 2.999408428739025023, -19.78128511538675127, -1.500000000000002220 ) ) ;
#1101 = CARTESIAN_POINT ( 'NONE',  ( -36.62287095715005592, -29.50247984919015209, -1.443849546365060466 ) ) ;
#1102 = CARTESIAN_POINT ( 'NONE',  ( -116.5175123996784095, -24.35071581493543746, 9.817618358456021710 ) ) ;
#1103 = ORIENTED_EDGE ( 'NONE', *, *, #49017, .T. ) ;
#1104 = TOROIDAL_SURFACE ( 'NONE', #25364, 80.18232118519038920, 8.160000000000000142 ) ;
#1105 = DIRECTION ( 'NONE',  ( -0.000000000000000000, 2.173523156925979552E-06, -0.9999999999976378895 ) ) ;
#1106 = CARTESIAN_POINT ( 'NONE',  ( -110.3346797185884327, -25.18430153814381356, 3.293943118072274689 ) ) ;
#1107 = EDGE_CURVE ( 'NONE', #68694, #33348, #54517, .T. ) ;
#1108 = LINE ( 'NONE', #45778, #75272 ) ;
#1109 = CARTESIAN_POINT ( 'NONE',  ( -108.5228709571500474, -24.50216790748205042, 0.6166512839542558355 ) ) ;
#1110 = EDGE_CURVE ( 'NONE', #52812, #39486, #60646, .T. ) ;
#1111 = DIRECTION ( 'NONE',  ( -1.000000000000000000, -3.773278334444167608E-23, -8.201307833595939069E-29 ) ) ;
#1112 = CARTESIAN_POINT ( 'NONE',  ( -83.64043043277688128, -23.73766607897670511, -1.055555164236457122 ) ) ;
#1113 = AXIS2_PLACEMENT_3D ( 'NONE', #3266, #34207, #17467 ) ;
#1114 = CARTESIAN_POINT ( 'NONE',  ( -63.62287095715004881, -24.66019654487199020, 8.947790411086131712 ) ) ;
#1116 = AXIS2_PLACEMENT_3D ( 'NONE', #81771, #19857, #64077 ) ;
#1115 = DIRECTION ( 'NONE',  ( -3.773278334453079030E-23, 0.9999999999976377785, 2.173523156925979128E-06 ) ) ;
#1117 = EDGE_LOOP ( 'NONE', ( #16397, #1638, #88766, #59303 ) ) ;
#1118 = CIRCLE ( 'NONE', #27053, 1.306876713926001354 ) ;
#1119 = CARTESIAN_POINT ( 'NONE',  ( 20.23811035156253979, -1.552196809741442696, -1.500000000000002220 ) ) ;
#1120 = ADVANCED_FACE ( 'NONE', ( #78198 ), #85315, .T. ) ;
#1121 = CARTESIAN_POINT ( 'NONE',  ( 31.69157588112856061, 3.316774720514426456, 29.47507169338741662 ) ) ;
#1122 = VECTOR ( 'NONE', #15146, 1000.000000000000114 ) ;
#1123 = DIRECTION ( 'NONE',  ( 0.000000000000000000, 0.000000000000000000, -1.000000000000000000 ) ) ;
#1124 = ORIENTED_EDGE ( 'NONE', *, *, #36022, .T. ) ;
#1125 = CARTESIAN_POINT ( 'NONE',  ( -122.5228709571500616, -23.47596703998600631, 11.44779298504227860 ) ) ;
#1126 = CARTESIAN_POINT ( 'NONE',  ( 11.25103634530202790, -16.72154935384561725, -1.500000000000002220 ) ) ;
#1127 = CARTESIAN_POINT ( 'NONE',  ( 19.19679251752027227, 8.867671107084703408, 11.49999999999999645 ) ) ;
#1128 = CARTESIAN_POINT ( 'NONE',  ( 20.57361055066190758, -8.084994430987380909, -1.500000000000002220 ) ) ;
#1129 = B_SPLINE_CURVE_WITH_KNOTS ( 'NONE', 3,
 ( #52521, #22538, #53530, #29675 ),
 .UNSPECIFIED., .F., .F.,
 ( 4, 4 ),
 ( 0.000000000000000000, 9.999999999998897304E-05 ),
 .UNSPECIFIED. ) ;
#1130 = CARTESIAN_POINT ( 'NONE',  ( -17.31529204923715071, 11.11782870402162260, 11.49999999999998934 ) ) ;
#1131 = FACE_OUTER_BOUND ( 'NONE', #52472, .T. ) ;
#1132 = EDGE_LOOP ( 'NONE', ( #9244, #75305, #95750, #21316 ) ) ;
#1133 = CARTESIAN_POINT ( 'NONE',  ( 16.00000000000000000, 2.681976490132703452E-15, -21.89999999999999858 ) ) ;
#1134 = ORIENTED_EDGE ( 'NONE', *, *, #56098, .T. ) ;
#1135 = CARTESIAN_POINT ( 'NONE',  ( -70.27422298781921484, -25.31465149953924865, 4.851635142449610250 ) ) ;
#1136 = PLANE ( 'NONE',  #35654 ) ;
#1137 = ORIENTED_EDGE ( 'NONE', *, *, #28367, .F. ) ;
#1138 = ORIENTED_EDGE ( 'NONE', *, *, #17846, .F. ) ;
#1139 = EDGE_LOOP ( 'NONE', ( #55624, #82005, #26037, #95401 ) ) ;
#1140 = CARTESIAN_POINT ( 'NONE',  ( -112.6228709571500701, -23.48783264082479150, -1.443836473390060160 ) ) ;
#1141 = CARTESIAN_POINT ( 'NONE',  ( -55.55620429048339304, -24.99156044556202261, 7.747789690856174971 ) ) ;
#1142 = CARTESIAN_POINT ( 'NONE',  ( -0.001774553997815280816, -6.376774720514413630, 19.59623724171353487 ) ) ;
#1143 = CARTESIAN_POINT ( 'NONE',  ( -20.61657899823519813, -2.091364977790679980, -1.500000000000002220 ) ) ;
#1144 = EDGE_CURVE ( 'NONE', #79651, #57540, #99254, .T. ) ;
#1145 = CARTESIAN_POINT ( 'NONE',  ( -17.90551237062050305, -12.20792721910736667, 11.49999999999999645 ) ) ;
#1146 = ORIENTED_EDGE ( 'NONE', *, *, #3873, .T. ) ;
#1147 = CARTESIAN_POINT ( 'NONE',  ( -42.52287095715005449, -23.47596703998600631, 11.44779298504229281 ) ) ;
#1148 = VECTOR ( 'NONE', #51324, 1000.000000000000114 ) ;
#1149 = PLANE ( 'NONE',  #75563 ) ;
#1150 = CARTESIAN_POINT ( 'NONE',  ( -17.59303920844588376, -13.82112144285918731, 11.49999999999998934 ) ) ;
#1151 = CARTESIAN_POINT ( 'NONE',  ( -47.49414261739990195, -24.35071581493542325, 9.817618358456030592 ) ) ;
#1152 = CARTESIAN_POINT ( 'NONE',  ( -74.62287095715005592, -23.47596703998600631, 11.44779298504227860 ) ) ;
#1154 = ORIENTED_EDGE ( 'NONE', *, *, #72807, .T. ) ;
#1153 = ADVANCED_FACE ( 'NONE', ( #47777 ), #93426, .T. ) ;
#1155 = CARTESIAN_POINT ( 'NONE',  ( -119.4728709572981984, -25.40561137786259138, 5.197919763437823804 ) ) ;
#1156 = CARTESIAN_POINT ( 'NONE',  ( -35.58880974400002373, -24.52399227489126687, 9.353111116836519301 ) ) ;
#1157 = AXIS2_PLACEMENT_3D ( 'NONE', #37386, #99268, #29766 ) ;
#1158 = VERTEX_POINT ( 'NONE', #78691 ) ;
#1159 = ADVANCED_FACE ( 'NONE', ( #70104 ), #60998, .T. ) ;
#1160 = CARTESIAN_POINT ( 'NONE',  ( -27.96875734969026084, 3.316774720514426456, 24.50402280011861933 ) ) ;
#1161 = ORIENTED_EDGE ( 'NONE', *, *, #66445, .T. ) ;
#1162 = EDGE_CURVE ( 'NONE', #13059, #68694, #93933, .T. ) ;
#1163 = CARTESIAN_POINT ( 'NONE',  ( -57.62287095715004881, -23.47596703998600276, 11.44779298504227683 ) ) ;
#1164 = CARTESIAN_POINT ( 'NONE',  ( -9.521469661382619520, 18.92286876745961166, -1.500000000000002220 ) ) ;
#1165 = VERTEX_POINT ( 'NONE', #9197 ) ;
#1166 = CARTESIAN_POINT ( 'NONE',  ( -117.5162854265894623, -24.65952944569305316, 1.056160979905706343 ) ) ;
#1167 = CARTESIAN_POINT ( 'NONE',  ( -21.44618410820073606, 4.064364382921047181, 11.49999999999998934 ) ) ;
#1168 = FACE_OUTER_BOUND ( 'NONE', #5300, .T. ) ;
#1169 = DIRECTION ( 'NONE',  ( 0.000000000000000000, 0.9999999999976377785, 2.173523156925979975E-06 ) ) ;
#1170 = DIRECTION ( 'NONE',  ( 4.251773225433346808E-15, 0.000000000000000000, -1.000000000000000000 ) ) ;
#1171 = CARTESIAN_POINT ( 'NONE',  ( -21.80608713477256089, -0.9339522974687717305, -1.500000000000002220 ) ) ;
#1172 = CARTESIAN_POINT ( 'NONE',  ( -95.52287095715011844, -23.48783264082477373, -1.443836473390086139 ) ) ;
#1173 = ORIENTED_EDGE ( 'NONE', *, *, #95629, .F. ) ;
#1174 = CARTESIAN_POINT ( 'NONE',  ( -41.62287095715006302, -23.94994826722565762, -0.6494450866342744710 ) ) ;
#1175 = CARTESIAN_POINT ( 'NONE',  ( 27.86270917940689174, -5.965225279485572685, 29.49402280011862487 ) ) ;
#1176 = VERTEX_POINT ( 'NONE', #38141 ) ;
#1177 = CARTESIAN_POINT ( 'NONE',  ( -51.62287095715005592, -23.48786465467241413, 11.44779295918254824 ) ) ;
#1178 = AXIS2_PLACEMENT_3D ( 'NONE', #59730, #45004, #75923 ) ;
#1179 = ORIENTED_EDGE ( 'NONE', *, *, #4696, .T. ) ;
#1180 = ORIENTED_EDGE ( 'NONE', *, *, #59638, .F. ) ;
#1181 = PLANE ( 'NONE',  #19985 ) ;
#1182 = CARTESIAN_POINT ( 'NONE',  ( -119.9228709571500531, -23.47593901973090524, -1.443836447538996426 ) ) ;
#1183 = CARTESIAN_POINT ( 'NONE',  ( -18.66175431467001999, 10.11895122522205526, 11.49999999999998934 ) ) ;
#1184 = FACE_OUTER_BOUND ( 'NONE', #87782, .T. ) ;
#1185 = CARTESIAN_POINT ( 'NONE',  ( -130.5728709571501156, -25.56688301298834531, 3.825958421598583570 ) ) ;
#1186 = DIRECTION ( 'NONE',  ( 0.000000000000000000, 0.9999999999976377785, 2.173523156925979128E-06 ) ) ;
#1187 = CIRCLE ( 'NONE', #28779, 8.452410033082761842 ) ;
#1188 = DIRECTION ( 'NONE',  ( -3.773278334453079030E-23, 0.9999999999976377785, 2.173523156925979128E-06 ) ) ;
#1189 = EDGE_CURVE ( 'NONE', #54238, #76045, #40157, .T. ) ;
#1190 = CARTESIAN_POINT ( 'NONE',  ( -0.1161231997828221785, -19.40653004597026410, -1.500000000000002220 ) ) ;
#1192 = CARTESIAN_POINT ( 'NONE',  ( -39.03507040974603370, -25.03707806782366418, 7.590868867492675420 ) ) ;
#1191 = B_SPLINE_CURVE_WITH_KNOTS ( 'NONE', 3,
 ( #16673, #17174, #1969, #47141 ),
 .UNSPECIFIED., .F., .F.,
 ( 4, 4 ),
 ( 0.000000000000000000, 9.999999999997510880E-05 ),
 .UNSPECIFIED. ) ;
#1193 = EDGE_LOOP ( 'NONE', ( #61323, #11249, #53370, #4307, #94744 ) ) ;
#1194 = CARTESIAN_POINT ( 'NONE',  ( 6.171429453590791425, 18.48145409631445446, 11.49999999999999645 ) ) ;
#1195 = CARTESIAN_POINT ( 'NONE',  ( -42.52287095715005449, -23.72773821059535848, 11.05748984161097503 ) ) ;
#1196 = EDGE_CURVE ( 'NONE', #1265, #86370, #80724, .T. ) ;
#1197 = VECTOR ( 'NONE', #14138, 1000.000000000000114 ) ;
#1198 = B_SPLINE_CURVE_WITH_KNOTS ( 'NONE', 3,
 ( #25871, #97383, #34985, #27867 ),
 .UNSPECIFIED., .F., .F.,
 ( 4, 4 ),
 ( 2.775557561562891043E-17, 9.999999999998898659E-05 ),
 .UNSPECIFIED. ) ;
#1199 = CARTESIAN_POINT ( 'NONE',  ( -68.52287095715010423, -23.94994826722564696, -0.6494450866342724726 ) ) ;
#1200 = ORIENTED_EDGE ( 'NONE', *, *, #18607, .F. ) ;
#1201 = CARTESIAN_POINT ( 'NONE',  ( 4.966987340572156739, -5.876774720514417183, 20.16530235339958210 ) ) ;
#1202 = EDGE_CURVE ( 'NONE', #34031, #27877, #13339, .T. ) ;
#1203 = DIRECTION ( 'NONE',  ( -3.773278334444167608E-23, 1.000000000000000000, 0.000000000000000000 ) ) ;
#1204 = EDGE_CURVE ( 'NONE', #7479, #61485, #73937, .T. ) ;
#1205 = CARTESIAN_POINT ( 'NONE',  ( -50.38822539166533687, -25.30267106383720943, 4.736250553104468075 ) ) ;
#1206 = CARTESIAN_POINT ( 'NONE',  ( -93.52216986576536328, -23.48786465467241058, 11.44779295918254469 ) ) ;
#1207 = CARTESIAN_POINT ( 'NONE',  ( -8.025172913017740939, -17.94849717234452768, 11.49999999999998934 ) ) ;
#1208 = VERTEX_POINT ( 'NONE', #17822 ) ;
#1209 = CARTESIAN_POINT ( 'NONE',  ( 21.52761780497506905, -1.784033869580059939, -1.500000000000002220 ) ) ;
#1210 = CARTESIAN_POINT ( 'NONE',  ( -40.49855218390116818, -24.15503026093912453, -0.2815557561904605821 ) ) ;
#1211 = CARTESIAN_POINT ( 'NONE',  ( 3.138110291115776995, 11.54688212118755075, -3.549999999999999822 ) ) ;
#1212 = CARTESIAN_POINT ( 'NONE',  ( 5.194767643164344584, 22.50260600399833422, -1.500000000000002220 ) ) ;
#1213 = CALENDAR_DATE ( 2026, 9, 10 ) ;
#1214 = CARTESIAN_POINT ( 'NONE',  ( -93.50527755429412480, -24.65952944569305316, 1.056160979905699904 ) ) ;
#1215 = PLANE ( 'NONE',  #21468 ) ;
#1216 = CARTESIAN_POINT ( 'NONE',  ( 6.546094359317672584, -6.376774720514411854, 19.73546617144828375 ) ) ;
#1217 = DIRECTION ( 'NONE',  ( 0.000000000000000000, -0.000000000000000000, -1.000000000000000000 ) ) ;
#1219 = B_SPLINE_CURVE_WITH_KNOTS ( 'NONE', 3,
 ( #9722, #63526, #40677, #41177 ),
 .UNSPECIFIED., .F., .F.,
 ( 4, 4 ),
 ( 1.387778780781445676E-17, 9.999999999996123101E-05 ),
 .UNSPECIFIED. ) ;
#1218 = CARTESIAN_POINT ( 'NONE',  ( -111.2413225215033634, -25.29823881010014475, 3.153768976815904956 ) ) ;
#1220 = CARTESIAN_POINT ( 'NONE',  ( -124.5562042904834072, -23.48786465467241769, 11.44779295918253759 ) ) ;
#1221 = CARTESIAN_POINT ( 'NONE',  ( -114.6266390397259869, -24.15620529776629155, 10.23563542870659404 ) ) ;
#1223 = EDGE_CURVE ( 'NONE', #98531, #71754, #51619, .T. ) ;
#1222 = CARTESIAN_POINT ( 'NONE',  ( -4.359361796094493258, -19.42695174060331809, 11.49999999999998934 ) ) ;
#1224 = CARTESIAN_POINT ( 'NONE',  ( -75.50249853208187290, -24.40133493613049964, 9.663955038902805939 ) ) ;
#1225 = CARTESIAN_POINT ( 'NONE',  ( -18.99895575154661742, -5.639348582513488140, -1.500000000000002220 ) ) ;
#1226 = ORIENTED_EDGE ( 'NONE', *, *, #78966, .F. ) ;
#1227 = AXIS2_PLACEMENT_3D ( 'NONE', #5527, #58831, #28368 ) ;
#1228 = CARTESIAN_POINT ( 'NONE',  ( -56.59864057370428014, -23.96119346886880663, -0.6495511937832126881 ) ) ;
#1229 = CARTESIAN_POINT ( 'NONE',  ( 8.071512145086526147, -7.528487854913508137, -6.499999999999999112 ) ) ;
#1230 = CARTESIAN_POINT ( 'NONE',  ( -95.62287095715005592, -24.99132157543084531, 2.256160258750667502 ) ) ;
#1231 = CARTESIAN_POINT ( 'NONE',  ( -15.76495264167062160, -13.51897010167481739, 11.49999999999999645 ) ) ;
#1232 = AXIS2_PLACEMENT_3D ( 'NONE', #93901, #55360, #86291 ) ;
#1233 = CARTESIAN_POINT ( 'NONE',  ( -110.6228709571500559, -29.50250243563736774, 8.947779886222136270 ) ) ;
#1234 = B_SPLINE_CURVE_WITH_KNOTS ( 'NONE', 3,
 ( #27033, #90425, #29019, #82803, #35152, #50878, #35649, #97041, #43758, #51874, #83302, #89928, #28519, #66124 ),
 .UNSPECIFIED., .F., .F.,
 ( 4, 2, 2, 2, 2, 2, 4 ),
 ( 1.398578778534940505E-17, 0.0002750759563669337307, 0.0005501519127338534753, 0.001100303825467730586, 0.001650455738201607805, 0.001925531694568536874, 0.002200607650935465943 ),
 .UNSPECIFIED. ) ;
#1235 = ADVANCED_FACE ( 'NONE', ( #95443 ), #65029, .F. ) ;
#1236 = CARTESIAN_POINT ( 'NONE',  ( -120.5228709571500616, -29.50249982740957577, 7.747779886224967605 ) ) ;
#1237 = CARTESIAN_POINT ( 'NONE',  ( -19.53289989604362376, -11.71160353944097920, 11.49999999999999645 ) ) ;
#1238 = ORIENTED_EDGE ( 'NONE', *, *, #52855, .T. ) ;
#1239 = B_SPLINE_SURFACE_WITH_KNOTS ( 'NONE', 3, 3, ( 
 ( #18580, #86599, #70890, #19081 ),
 ( #39927, #95717, #40930, #87609 ),
 ( #17591, #87099, #94204, #25699 ),
 ( #63287, #71892, #48049, #79985 ),
 ( #2886, #78979, #55673, #26707 ),
 ( #10474, #24689, #49057, #1872 ),
 ( #41432, #32314, #9476, #72391 ) ),
 .UNSPECIFIED., .F., .F., .F.,
 ( 4, 3, 4 ),
 ( 4, 4 ),
 ( 0.7945040050992242531, 0.8970133687736503436, 0.9995227324480764342 ),
 ( 0.6696641681890944664, 0.6709860541624589336 ),
 .UNSPECIFIED. ) ;
#1240 = CARTESIAN_POINT ( 'NONE',  ( -83.62287095715002749, -24.51387760970723306, 9.387446482453402297 ) ) ;
#1241 = EDGE_CURVE ( 'NONE', #19777, #34658, #46760, .T. ) ;
#1242 = CARTESIAN_POINT ( 'NONE',  ( 32.16024265030974050, 5.965225279485572685, 16.27760796525321751 ) ) ;
#1243 = ORIENTED_EDGE ( 'NONE', *, *, #92389, .F. ) ;
#1244 = CARTESIAN_POINT ( 'NONE',  ( 7.037473118728134303, -18.94123407977296480, 11.49999999999998934 ) ) ;
#1245 = DIRECTION ( 'NONE',  ( 0.000000000000000000, 0.9999999999976377785, 2.173523156925979975E-06 ) ) ;
#1246 = EDGE_CURVE ( 'NONE', #44958, #35328, #87838, .T. ) ;
#1247 = CARTESIAN_POINT ( 'NONE',  ( -40.41683116089613748, -25.30532407203700984, 5.082404393492757855 ) ) ;
#1248 = EDGE_CURVE ( 'NONE', #92355, #38340, #26668, .T. ) ;
#1249 = ORIENTED_EDGE ( 'NONE', *, *, #89542, .F. ) ;
#1250 = CARTESIAN_POINT ( 'NONE',  ( -40.52287095715006870, -23.48786465467241058, 11.44779295918255180 ) ) ;
#1251 = CARTESIAN_POINT ( 'NONE',  ( -9.675568039816649701, -20.77828039667204862, -1.500000000000002220 ) ) ;
#1253 = EDGE_CURVE ( 'NONE', #19743, #19988, #14617, .T. ) ;
#1252 = CARTESIAN_POINT ( 'NONE',  ( -29.47549908493335735, -24.57252240364413609, 1.056161296257513094 ) ) ;
#1254 = CARTESIAN_POINT ( 'NONE',  ( -15.89961544564849305, 12.09337254111102844, -1.500000000000002220 ) ) ;
#1255 = CARTESIAN_POINT ( 'NONE',  ( -102.6228709571500559, -29.50248528299804818, 1.056150453629042030 ) ) ;
#1256 = CARTESIAN_POINT ( 'NONE',  ( -5.413507703253908510, 20.27406835261982465, 11.49999999999999645 ) ) ;
#1257 = CARTESIAN_POINT ( 'NONE',  ( -86.62287095715008434, -24.33927499327854704, 9.819080762295811837 ) ) ;
#1258 = DIRECTION ( 'NONE',  ( 0.000000000000000000, -1.000000000000000000, 0.000000000000000000 ) ) ;
#1259 = CARTESIAN_POINT ( 'NONE',  ( -5.411813039392390223, -21.34095290059367755, 11.49999999999998934 ) ) ;
#1260 = AXIS2_PLACEMENT_3D ( 'NONE', #64575, #57454, #18864 ) ;
#1261 = DIRECTION ( 'NONE',  ( -0.000000000000000000, -1.000000000000000000, 8.393823270855534040E-16 ) ) ;
#1262 = ORIENTED_EDGE ( 'NONE', *, *, #73493, .T. ) ;
#1263 = CARTESIAN_POINT ( 'NONE',  ( -49.93954932203694597, -25.27344777607457260, 3.376895343913014713 ) ) ;
#1264 = PLANE ( 'NONE',  #77022 ) ;
#1265 = VERTEX_POINT ( 'NONE', #57408 ) ;
#1266 = CARTESIAN_POINT ( 'NONE',  ( 3.769940963823357638, -6.376774720514402972, 18.16074422543206879 ) ) ;
#1267 = ORIENTED_EDGE ( 'NONE', *, *, #93453, .F. ) ;
#1268 = VECTOR ( 'NONE', #59346, 1000.000000000000114 ) ;
#1269 = VERTEX_POINT ( 'NONE', #10209 ) ;
#1270 = DIRECTION ( 'NONE',  ( 7.994117400814786717E-16, 0.000000000000000000, -1.000000000000000000 ) ) ;
#1271 = PLANE ( 'NONE',  #61 ) ;
#1272 = CARTESIAN_POINT ( 'NONE',  ( -4.194375271223358403, -6.376774720514417183, 20.09898898868106087 ) ) ;
#1273 = CARTESIAN_POINT ( 'NONE',  ( -17.80769721941407369, -10.09151516499986734, -1.500000000000002220 ) ) ;
#1274 = ORIENTED_EDGE ( 'NONE', *, *, #9439, .F. ) ;
#1275 = FACE_OUTER_BOUND ( 'NONE', #69418, .T. ) ;
#1276 = B_SPLINE_CURVE_WITH_KNOTS ( 'NONE', 3,
 ( #3253, #3745, #71753, #24557 ),
 .UNSPECIFIED., .F., .F.,
 ( 4, 4 ),
 ( 0.3907790457512309579, 0.3997854770233464916 ),
 .UNSPECIFIED. ) ;
#1277 = CARTESIAN_POINT ( 'NONE',  ( -44.57673861720984831, -24.65952944569304606, 1.056160979905693909 ) ) ;
#1278 = DIRECTION ( 'NONE',  ( -3.773278334453079618E-23, 0.9999999999976377785, 2.173523156925979975E-06 ) ) ;
#1279 = CARTESIAN_POINT ( 'NONE',  ( 21.63714550250683644, -5.416328558471028565, -1.500000000000002220 ) ) ;
#1280 = LINE ( 'NONE', #40333, #30253 ) ;
#1281 = CARTESIAN_POINT ( 'NONE',  ( -90.62287095715004170, -24.99156045073392818, 7.747789690856161648 ) ) ;
#1282 = VERTEX_POINT ( 'NONE', #49790 ) ;
#1283 = CARTESIAN_POINT ( 'NONE',  ( -29.52587214738113275, -25.05018694314834349, 2.947979682295396753 ) ) ;
#1284 = DIRECTION ( 'NONE',  ( -0.2488812114211667037, 0.000000000000000000, -0.9685340172660599212 ) ) ;
#1285 = CARTESIAN_POINT ( 'NONE',  ( 9.770152518076534065, 18.40777400073588410, -1.500000000000002220 ) ) ;
#1286 = ORIENTED_EDGE ( 'NONE', *, *, #25325, .T. ) ;
#1288 = EDGE_LOOP ( 'NONE', ( #1431, #4389, #68582, #86609 ) ) ;
#1287 = DIRECTION ( 'NONE',  ( 0.6599726524652350657, 0.000000000000000000, -0.7512896232465892110 ) ) ;
#1289 = EDGE_LOOP ( 'NONE', ( #77277, #33087, #83521, #33162, #33804, #78860, #58280, #20417, #73763, #77798, #100157, #5747, #24089, #27868, #8227, #81213 ) ) ;
#1290 = CARTESIAN_POINT ( 'NONE',  ( -51.45055690290539019, -25.25854447648429257, 6.541366898730298196 ) ) ;
#1291 = CARTESIAN_POINT ( 'NONE',  ( 20.48634023128459347, 4.603634630958829632, -1.500000000000002220 ) ) ;
#1292 = ORIENTED_EDGE ( 'NONE', *, *, #53692, .T. ) ;
#1293 = CARTESIAN_POINT ( 'NONE',  ( -93.62287095715005592, -24.66019654487199730, 8.947790411086124607 ) ) ;
#1294 = CARTESIAN_POINT ( 'NONE',  ( -105.6228709571500559, -29.50247984919015209, -1.443849546365048253 ) ) ;
#1295 = CARTESIAN_POINT ( 'NONE',  ( -5.891025641025637860, -6.376774720514427841, 21.75000000000000711 ) ) ;
#1296 = CARTESIAN_POINT ( 'NONE',  ( -86.59169610958005592, -24.15620529776628445, 10.23563542870660292 ) ) ;
#1297 = CARTESIAN_POINT ( 'NONE',  ( -59.54289001521522096, -24.34968618360933235, 0.1864209137778795600 ) ) ;
#1298 = CARTESIAN_POINT ( 'NONE',  ( 2.246611357655419638, -0.1632191352058106892, -0.1632191352058112721 ) ) ;
#1300 = ORIENTED_EDGE ( 'NONE', *, *, #97309, .F. ) ;
#1299 = CARTESIAN_POINT ( 'NONE',  ( 21.63176498729014341, 4.993826359924048219, 11.49999999999999645 ) ) ;
#1301 = CARTESIAN_POINT ( 'NONE',  ( 10.34999999999999254, 4.999999999999998224, 2.100000000000000089 ) ) ;
#1302 = DIRECTION ( 'NONE',  ( 0.000000000000000000, 1.064096645546785541E-13, -1.000000000000000000 ) ) ;
#1303 = ORIENTED_EDGE ( 'NONE', *, *, #28565, .F. ) ;
#1304 = CARTESIAN_POINT ( 'NONE',  ( -18.74212433040710479, 12.77821124017617649, 11.49999999999998934 ) ) ;
#1305 = AXIS2_PLACEMENT_3D ( 'NONE', #64858, #9533, #88669 ) ;
#1307 = VERTEX_POINT ( 'NONE', #33546 ) ;
#1306 = DIRECTION ( 'NONE',  ( -0.000000000000000000, -1.000000000000000000, -0.000000000000000000 ) ) ;
#1308 = EDGE_LOOP ( 'NONE', ( #60717, #42717, #64099, #6541, #66658 ) ) ;
#1309 = FACE_OUTER_BOUND ( 'NONE', #15010, .T. ) ;
#1310 = EDGE_CURVE ( 'NONE', #58916, #71424, #75858, .T. ) ;
#1311 = CARTESIAN_POINT ( 'NONE',  ( 19.08902475966321788, 6.433202353099247262, -1.500000000000002220 ) ) ;
#1312 = CARTESIAN_POINT ( 'NONE',  ( -80.62287095715004170, -23.48783264082478439, -1.443836473390065489 ) ) ;
#1313 = ORIENTED_EDGE ( 'NONE', *, *, #36693, .T. ) ;
#1314 = CARTESIAN_POINT ( 'NONE',  ( 14.56569730433575138, -3.366897624368339059, -28.38594530802194882 ) ) ;
#1315 = CARTESIAN_POINT ( 'NONE',  ( -19.61019785865472542, -10.87575402790796453, -1.500000000000002220 ) ) ;
#1316 = ORIENTED_EDGE ( 'NONE', *, *, #313, .T. ) ;
#1317 = ORIENTED_EDGE ( 'NONE', *, *, #68324, .T. ) ;
#1318 = DIRECTION ( 'NONE',  ( 0.000000000000000000, 0.000000000000000000, 1.000000000000000000 ) ) ;
#1319 = CARTESIAN_POINT ( 'NONE',  ( -4.223504350552545361, -5.876774720514411854, 19.52341893546492813 ) ) ;
#1320 = FACE_OUTER_BOUND ( 'NONE', #98470, .T. ) ;
#1321 = EDGE_CURVE ( 'NONE', #27358, #38179, #32770, .T. ) ;
#1322 = EDGE_CURVE ( 'NONE', #98063, #56695, #34552, .T. ) ;
#1323 = CARTESIAN_POINT ( 'NONE',  ( -116.5228709571500332, -24.33927499327855415, 9.819080762295804732 ) ) ;
#1324 = VECTOR ( 'NONE', #23142, 999.9999999999998863 ) ;
#1325 = EDGE_CURVE ( 'NONE', #86005, #27949, #1355, .T. ) ;
#1326 = CARTESIAN_POINT ( 'NONE',  ( -63.92778996623335530, -24.47827083238275847, 0.5637492489085984548 ) ) ;
#1327 = CARTESIAN_POINT ( 'NONE',  ( 3.528372621398383924, 19.26332229581237598, 11.49999999999998934 ) ) ;
#1328 = CARTESIAN_POINT ( 'NONE',  ( -38.52287095715006870, -29.50250243563736774, 8.947779886222148704 ) ) ;
#1330 = EDGE_CURVE ( 'NONE', #34031, #100041, #19461, .T. ) ;
#1329 = ORIENTED_EDGE ( 'NONE', *, *, #76008, .F. ) ;
#1331 = CARTESIAN_POINT ( 'NONE',  ( 14.19067371521932230, 16.14321034643037578, -1.500000000000002220 ) ) ;
#1332 = CARTESIAN_POINT ( 'NONE',  ( -102.5562042904833930, -23.48786465467241058, 11.44779295918254114 ) ) ;
#1333 = DIRECTION ( 'NONE',  ( 0.1478094111296165969, -0.9890158633619159367, 0.000000000000000000 ) ) ;
#1334 = CARTESIAN_POINT ( 'NONE',  ( -113.5228709571500616, -24.35013146730205236, 9.818937971375095941 ) ) ;
#1335 = CARTESIAN_POINT ( 'NONE',  ( -111.6228709571500559, -24.65952944569304606, 1.056160979905703901 ) ) ;
#1336 = CARTESIAN_POINT ( 'NONE',  ( -2.941484630304247450, -22.72858670154147376, -1.500000000000002220 ) ) ;
#1337 = VECTOR ( 'NONE', #93193, 1000.000000000000114 ) ;
#1338 = CALENDAR_DATE ( 2026, 9, 10 ) ;
#1339 = DIRECTION ( 'NONE',  ( -0.000000000000000000, 2.173523156925979552E-06, -0.9999999999976378895 ) ) ;
#1340 = CARTESIAN_POINT ( 'NONE',  ( -42.52287095715005449, -23.96127896942123670, -0.6493128930941061139 ) ) ;
#1341 = CARTESIAN_POINT ( 'NONE',  ( 19.36564117097816862, 5.170944958934900804, 11.49999999999999645 ) ) ;
#1342 = DIRECTION ( 'NONE',  ( 0.000000000000000000, -0.9999999999976377785, -2.173523156925979128E-06 ) ) ;
#1343 = DIRECTION ( 'NONE',  ( 0.000000000000000000, 0.000000000000000000, 1.000000000000000000 ) ) ;
#1344 = AXIS2_PLACEMENT_3D ( 'NONE', #12698, #49296, #4109 ) ;
#1345 = CARTESIAN_POINT ( 'NONE',  ( -10.54059822343757880, -5.876774720514426953, 22.82308057603841078 ) ) ;
#1346 = CARTESIAN_POINT ( 'NONE',  ( -71.62287095715005592, -29.50250243563736774, 8.947779886222143375 ) ) ;
#1347 = VERTEX_POINT ( 'NONE', #1602 ) ;
#1348 = CARTESIAN_POINT ( 'NONE',  ( -50.62287095715008434, -24.52323809116984421, 9.355190652339420154 ) ) ;
#1349 = ADVANCED_FACE ( 'NONE', ( #17313 ), #48278, .T. ) ;
#1350 = CARTESIAN_POINT ( 'NONE',  ( -16.08361747308824263, -14.67194924222005170, 11.49999999999998934 ) ) ;
#1351 = CARTESIAN_POINT ( 'NONE',  ( -65.62287095715005592, -23.47596703998600631, 11.44779298504227683 ) ) ;
#1352 = CARTESIAN_POINT ( 'NONE',  ( 18.74904333037421011, -5.873301551693434597, -1.500000000000002220 ) ) ;
#1353 = CARTESIAN_POINT ( 'NONE',  ( 13.60020833695035947, 0.000000000000000000, 0.000000000000000000 ) ) ;
#1354 = ADVANCED_FACE ( 'NONE', ( #67013 ), #82212, .T. ) ;
#1355 = CIRCLE ( 'NONE', #96950, 0.8160000000000007248 ) ;
#1356 = CARTESIAN_POINT ( 'NONE',  ( -2.749999999999999112, 26.59999999999999432, 2.100000000000000089 ) ) ;
#1357 = CALENDAR_DATE ( 2026, 9, 10 ) ;
#1358 = CARTESIAN_POINT ( 'NONE',  ( -91.59781932095023649, -23.73791477778911840, 11.05961554403170410 ) ) ;
#1359 = CARTESIAN_POINT ( 'NONE',  ( 2.589743589743596086, -6.376774720514415407, 20.00140224358974095 ) ) ;
#1360 = CARTESIAN_POINT ( 'NONE',  ( -18.11865614447288664, 9.752654332028551920, 11.49999999999999645 ) ) ;
#1361 = FACE_OUTER_BOUND ( 'NONE', #49208, .T. ) ;
#1362 = EDGE_CURVE ( 'NONE', #22913, #18521, #44812, .T. ) ;
#1363 = CARTESIAN_POINT ( 'NONE',  ( -120.5888113947464291, -24.73486907724918638, 1.287355809206965684 ) ) ;
#1364 = CARTESIAN_POINT ( 'NONE',  ( 15.43685675143394498, -16.52047792065556564, 11.49999999999999645 ) ) ;
#1365 = ORIENTED_EDGE ( 'NONE', *, *, #57930, .F. ) ;
#1366 =( LENGTH_UNIT ( ) NAMED_UNIT ( * ) SI_UNIT ( .MILLI., .METRE. ) );
#1367 = CARTESIAN_POINT ( 'NONE',  ( -99.59758909298055585, -25.31296351044734649, 4.277504013324993970 ) ) ;
#1368 = CARTESIAN_POINT ( 'NONE',  ( 0.4325450954222598288, 0.000000000000000000, 0.000000000000000000 ) ) ;
#1369 = DIRECTION ( 'NONE',  ( -0.000000000000000000, 1.000000000000000000, -0.000000000000000000 ) ) ;
#1370 = CARTESIAN_POINT ( 'NONE',  ( 15.00914443175702573, -3.504414796833706713, -27.32709449451501982 ) ) ;
#1371 = CARTESIAN_POINT ( 'NONE',  ( -26.05468383228075169, -24.61459909436555549, 7.311465941504138755 ) ) ;
#1372 = ADVANCED_FACE ( 'NONE', ( #20299 ), #97442, .T. ) ;
#1373 = CARTESIAN_POINT ( 'NONE',  ( 8.160000000000000142, -9.652339641703484574, 1.628518864987183790 ) ) ;
#1374 = EDGE_CURVE ( 'NONE', #83628, #62593, #21786, .T. ) ;
#1375 = ORIENTED_EDGE ( 'NONE', *, *, #44564, .F. ) ;
#1376 = CARTESIAN_POINT ( 'NONE',  ( -23.29179552176161749, -5.965225279485594001, -17.29637630388738501 ) ) ;
#1377 = CARTESIAN_POINT ( 'NONE',  ( 21.82588152991271713, 6.770963248321698380, 11.49999999999998934 ) ) ;
#1378 = CARTESIAN_POINT ( 'NONE',  ( -125.5895376238167245, -25.00158670708909625, 2.256160236439167299 ) ) ;
#1379 = B_SPLINE_SURFACE_WITH_KNOTS ( 'NONE', 3, 1, ( 
 ( #63782, #7957 ),
 ( #94190, #86585 ),
 ( #55659, #38913 ),
 ( #9463, #24182 ),
 ( #55158, #48037 ),
 ( #71378, #1860 ),
 ( #48547, #32804 ),
 ( #94698, #42438 ),
 ( #50044, #10969 ),
 ( #96211, #80474 ),
 ( #79974, #2873 ),
 ( #34309, #73372 ),
 ( #49545, #25688 ),
 ( #33295, #64281 ),
 ( #18077, #19570 ),
 ( #72877, #49045 ),
 ( #41934, #2364 ),
 ( #95205, #65287 ),
 ( #56658, #72378 ) ),
 .UNSPECIFIED., .F., .F., .F.,
 ( 4, 1, 1, 1, 1, 1, 1, 1, 1, 1, 1, 1, 1, 1, 1, 1, 4 ),
 ( 2, 2 ),
 ( 0.000000000000000000, 0.06796237149444751824, 0.1332834028675206339, 0.1978352977570501381, 0.2608919865309831110, 0.3233765044831737323, 0.3863500754690828431, 0.4496377310517088999, 0.5147953269783526187, 0.5792399132410260831, 0.6418141777582863083, 0.7013585647860591799, 0.7607267659857173125, 0.8192220679243865655, 0.8787161693846299304, 0.9381473540533079580, 1.000000000000000000 ),
 ( 0.000000000000000000, 1.000000000000000000 ),
 .UNSPECIFIED. ) ;
#1380 = CARTESIAN_POINT ( 'NONE',  ( -96.62764832958193040, -24.34968618360933945, 0.1864209137778869152 ) ) ;
#1381 = DIRECTION ( 'NONE',  ( -1.526034937513432889E-15, 7.121496375062686157E-15, -1.000000000000000000 ) ) ;
#1382 = CARTESIAN_POINT ( 'NONE',  ( -3.368041826647835357, -22.21310627845187824, 11.49999999999999645 ) ) ;
#1383 = ORIENTED_EDGE ( 'NONE', *, *, #3275, .F. ) ;
#1384 = CARTESIAN_POINT ( 'NONE',  ( -43.64731547651398813, -23.96119346886880663, -0.6495511937831988103 ) ) ;
#1385 = CARTESIAN_POINT ( 'NONE',  ( -3.149188516569510377, 21.71089317892358395, 11.49999999999998934 ) ) ;
#1386 = CARTESIAN_POINT ( 'NONE',  ( -5.530932042872791499, -6.376774720514410077, 19.30497968945844534 ) ) ;
#1387 = CARTESIAN_POINT ( 'NONE',  ( -44.49312653990953237, -24.35071581493543036, 9.817618358456025263 ) ) ;
#1388 = DIRECTION ( 'NONE',  ( 1.000000000000000000, 3.773278334444167608E-23, 8.201307833595939069E-29 ) ) ;
#1389 = VERTEX_POINT ( 'NONE', #97924 ) ;
#1390 = CARTESIAN_POINT ( 'NONE',  ( -48.51405841811074993, -23.73791477778911840, 11.05961554403170766 ) ) ;
#1391 = DIRECTION ( 'NONE',  ( -0.000000000000000000, -1.000000000000000000, -0.000000000000000000 ) ) ;
#1392 = ORIENTED_EDGE ( 'NONE', *, *, #60505, .F. ) ;
#1393 = CARTESIAN_POINT ( 'NONE',  ( -3.437008290023895185, 20.19323497536227663, -1.500000000000002220 ) ) ;
#1394 = EDGE_LOOP ( 'NONE', ( #50435, #9530, #4530, #16937 ) ) ;
#1395 = ORIENTED_EDGE ( 'NONE', *, *, #76896, .F. ) ;
#1396 = ORIENTED_EDGE ( 'NONE', *, *, #6681, .T. ) ;
#1397 = ORIENTED_EDGE ( 'NONE', *, *, #93110, .F. ) ;
#1398 = CARTESIAN_POINT ( 'NONE',  ( -5.126879528927636542, -22.49243673399587351, -1.500000000000002220 ) ) ;
#1399 = CARTESIAN_POINT ( 'NONE',  ( -82.52287095715007581, -24.33832256527049154, 0.1851278514138627596 ) ) ;
#1400 = CARTESIAN_POINT ( 'NONE',  ( -15.67655817637044890, 12.86142704545212290, -1.500000000000002220 ) ) ;
#1401 = ORIENTED_EDGE ( 'NONE', *, *, #73281, .T. ) ;
#1402 = CARTESIAN_POINT ( 'NONE',  ( 29.72843915439144524, 4.948038888671026037, 27.41656699113896067 ) ) ;
#1403 = AXIS2_PLACEMENT_3D ( 'NONE', #43039, #41540, #73479 ) ;
#1404 = CARTESIAN_POINT ( 'NONE',  ( -92.59430350763778961, -23.96119346886881374, -0.6495511937831873750 ) ) ;
#1405 = DIRECTION ( 'NONE',  ( 0.000000000000000000, -0.000000000000000000, -1.000000000000000000 ) ) ;
#1406 = CARTESIAN_POINT ( 'NONE',  ( 4.413617546364139166, -6.376774720514406525, 18.86076033669171181 ) ) ;
#1408 = EDGE_LOOP ( 'NONE', ( #69793, #49827, #66585, #25732 ) ) ;
#1407 = CARTESIAN_POINT ( 'NONE',  ( 19.88731969966643476, 8.162773808193900749, 11.49999999999999645 ) ) ;
#1409 = CARTESIAN_POINT ( 'NONE',  ( -75.56671859597047103, -23.48783264082477018, -1.443836473390089914 ) ) ;
#1410 = CARTESIAN_POINT ( 'NONE',  ( -104.6228709571500985, -23.94994826722515668, -0.6494450866351708651 ) ) ;
#1411 = ORIENTED_EDGE ( 'NONE', *, *, #16821, .T. ) ;
#1412 = CARTESIAN_POINT ( 'NONE',  ( 18.78520451414993531, -8.817701518030307994, 11.49999999999998934 ) ) ;
#1413 = ORIENTED_EDGE ( 'NONE', *, *, #87246, .T. ) ;
#1415 = ORIENTED_EDGE ( 'NONE', *, *, #31004, .T. ) ;
#1414 = CARTESIAN_POINT ( 'NONE',  ( -125.5890728391331521, -24.83618233451450763, 1.606449574219537046 ) ) ;
#1416 = CARTESIAN_POINT ( 'NONE',  ( -111.5955154881536799, -23.48786465467241769, 11.44779295918254114 ) ) ;
#1417 = DIRECTION ( 'NONE',  ( -3.773278334444167608E-23, 1.000000000000000000, 0.000000000000000000 ) ) ;
#1418 = VERTEX_POINT ( 'NONE', #67501 ) ;
#1419 = ORIENTED_EDGE ( 'NONE', *, *, #34775, .T. ) ;
#1420 = DIRECTION ( 'NONE',  ( -3.773278334444167608E-23, 1.000000000000000000, 0.000000000000000000 ) ) ;
#1421 = VECTOR ( 'NONE', #80102, 1000.000000000000114 ) ;
#1422 = CARTESIAN_POINT ( 'NONE',  ( -22.05275734969026047, -5.965225279485572685, 31.02402280011862246 ) ) ;
#1423 = CARTESIAN_POINT ( 'NONE',  ( -27.79921587522528625, -24.62298669958403252, 1.630323915293501624 ) ) ;
#1424 = CARTESIAN_POINT ( 'NONE',  ( -20.26759042640731323, -8.618136523154847239, 11.49999999999999645 ) ) ;
#1425 = CARTESIAN_POINT ( 'NONE',  ( -89.54580542116907793, -24.51419770103157703, 9.386484678747176957 ) ) ;
#1426 = CARTESIAN_POINT ( 'NONE',  ( -8.633696204196466439, -20.85254729778420923, 11.49999999999998934 ) ) ;
#1427 = CARTESIAN_POINT ( 'NONE',  ( 14.09988904737591575, 15.55221489148801872, 11.49999999999998934 ) ) ;
#1429 = ORIENTED_EDGE ( 'NONE', *, *, #54413, .F. ) ;
#1428 = DIRECTION ( 'NONE',  ( 0.000000000000000000, 0.000000000000000000, -1.000000000000000000 ) ) ;
#1430 = AXIS2_PLACEMENT_3D ( 'NONE', #10725, #87335, #58409 ) ;
#1431 = ORIENTED_EDGE ( 'NONE', *, *, #95584, .T. ) ;
#1432 = DIRECTION ( 'NONE',  ( -1.000000000000000000, -3.773278334444166432E-23, -8.201307841325785021E-29 ) ) ;
#1433 = B_SPLINE_CURVE_WITH_KNOTS ( 'NONE', 3,
 ( #60116, #98643, #43878, #4817, #91040, #67729 ),
 .UNSPECIFIED., .F., .F.,
 ( 4, 2, 4 ),
 ( 1.570755371633974110E-05, 0.001396183895866087103, 0.002776660238015834711 ),
 .UNSPECIFIED. ) ;
#1434 = CYLINDRICAL_SURFACE ( 'NONE', #78097, 1.149999999999998135 ) ;
#1435 = EDGE_LOOP ( 'NONE', ( #98396, #57347, #37572, #98327 ) ) ;
#1436 = CARTESIAN_POINT ( 'NONE',  ( -8.144517828999388698, 19.50133175306300970, 11.49999999999998934 ) ) ;
#1437 = CARTESIAN_POINT ( 'NONE',  ( -117.6228709571500559, -23.47593901973091235, -1.443836447538997536 ) ) ;
#1438 = EDGE_CURVE ( 'NONE', #65965, #61548, #13186, .T. ) ;
#1439 = CARTESIAN_POINT ( 'NONE',  ( -51.78109907783319699, -25.03148574646757396, 6.793045521090960825 ) ) ;
#1440 = CARTESIAN_POINT ( 'NONE',  ( -49.50841769935764347, -25.26288593538659910, 3.984447754961206734 ) ) ;
#1441 = CARTESIAN_POINT ( 'NONE',  ( -109.5895376238167245, -24.66019654487200441, 8.947790411086117501 ) ) ;
#1442 = CARTESIAN_POINT ( 'NONE',  ( -111.9545732713065291, -25.06732945298220372, 7.447791367849804445 ) ) ;
#1443 = CARTESIAN_POINT ( 'NONE',  ( 18.30470771955606679, 12.64531542519679697, -1.500000000000002220 ) ) ;
#1444 = EDGE_CURVE ( 'NONE', #81452, #60342, #47333, .T. ) ;
#1445 = CARTESIAN_POINT ( 'NONE',  ( -74.62287095715005592, -24.50321055353806443, 9.387540953477538253 ) ) ;
#1446 = EDGE_CURVE ( 'NONE', #62104, #68431, #6168, .T. ) ;
#1447 = ORIENTED_EDGE ( 'NONE', *, *, #39669, .T. ) ;
#1448 = CARTESIAN_POINT ( 'NONE',  ( -29.49875734969026198, 5.965225279485572685, 10.11402280011862587 ) ) ;
#1449 = CARTESIAN_POINT ( 'NONE',  ( -58.62287095715007013, -23.47596703998600276, 11.44779298504227683 ) ) ;
#1450 = CARTESIAN_POINT ( 'NONE',  ( 13.10664265030973930, -5.965225279485574461, -28.64597719988137570 ) ) ;
#1451 = ADVANCED_FACE ( 'NONE', ( #44158 ), #51271, .T. ) ;
#1452 = CARTESIAN_POINT ( 'NONE',  ( 5.717289507243528135, 5.356774720514425603, -25.39219853617310818 ) ) ;
#1453 = DIRECTION ( 'NONE',  ( 0.000000000000000000, 1.000000000000000000, 0.000000000000000000 ) ) ;
#1454 = CARTESIAN_POINT ( 'NONE',  ( -4.154358412494840280, 19.03220294597612039, -1.500000000000002220 ) ) ;
#1455 = CARTESIAN_POINT ( 'NONE',  ( -17.32345979880200204, -12.59856583755568415, -1.500000000000002220 ) ) ;
#1456 = CARTESIAN_POINT ( 'NONE',  ( -28.98875734969026041, 0.3587747205144262708, 23.37402280011862743 ) ) ;
#1457 = CARTESIAN_POINT ( 'NONE',  ( -60.63095941313405746, -24.73531770709804078, 8.716586749031112191 ) ) ;
#1458 = CARTESIAN_POINT ( 'NONE',  ( -51.59327120193346872, -24.15543982623907127, -0.2315651400026664530 ) ) ;
#1459 = CARTESIAN_POINT ( 'NONE',  ( -101.2457357660222641, -25.18440107031529251, 3.734961042421667710 ) ) ;
#1460 = CARTESIAN_POINT ( 'NONE',  ( -9.471985145535571249, 20.67137392225973258, -1.500000000000002220 ) ) ;
#1461 = CARTESIAN_POINT ( 'NONE',  ( -98.92287095715008149, -23.47596703998600631, 11.44779298504227860 ) ) ;
#1462 = FACE_OUTER_BOUND ( 'NONE', #27362, .T. ) ;
#1463 = CARTESIAN_POINT ( 'NONE',  ( 11.68167410197319001, -16.05257874518773065, 11.49999999999999645 ) ) ;
#1464 = CARTESIAN_POINT ( 'NONE',  ( -84.52287095715004739, -24.34917612406836795, 0.1852690917426538242 ) ) ;
#1465 = VECTOR ( 'NONE', #98941, 1000.000000000000000 ) ;
#1466 = CIRCLE ( 'NONE', #58180, 3.349999999999998757 ) ;
#1467 = CARTESIAN_POINT ( 'NONE',  ( 24.50000000000000000, -0.9000000000000000222, 1.103411337323757735 ) ) ;
#1468 = CARTESIAN_POINT ( 'NONE',  ( 8.160000000000000142, -10.15233964170348457, 0.003711184059992174607 ) ) ;
#1469 = ORIENTED_EDGE ( 'NONE', *, *, #69482, .T. ) ;
#1470 = CARTESIAN_POINT ( 'NONE',  ( -49.28481975526113956, -25.23807781832389807, 6.283675252660968269 ) ) ;
#1471 = CARTESIAN_POINT ( 'NONE',  ( -80.52287095715007581, -24.82576562948888821, 8.398263436605416743 ) ) ;
#1472 = CARTESIAN_POINT ( 'NONE',  ( -71.52287095715009002, -23.72773821059536559, 11.05748984161097326 ) ) ;
#1473 = CARTESIAN_POINT ( 'NONE',  ( -11.49108604648090548, 18.38894055434275643, -1.500000000000002220 ) ) ;
#1474 = CARTESIAN_POINT ( 'NONE',  ( -32.62287095715005592, -24.66019654487199020, 8.947790411086137041 ) ) ;
#1475 = VECTOR ( 'NONE', #35471, 1000.000000000000000 ) ;
#1476 = CARTESIAN_POINT ( 'NONE',  ( 1.133552453683672745, -19.47370032599940615, -1.500000000000002220 ) ) ;
#1477 = CARTESIAN_POINT ( 'NONE',  ( -55.53716315595536912, -24.63419186844611986, 9.035850630976923981 ) ) ;
#1478 = ADVANCED_FACE ( 'NONE', ( #28924 ), #21793, .T. ) ;
#1479 = ORIENTED_EDGE ( 'NONE', *, *, #26398, .F. ) ;
#1480 = B_SPLINE_CURVE_WITH_KNOTS ( 'NONE', 3,
 ( #52244, #61362, #37009, #85177 ),
 .UNSPECIFIED., .F., .F.,
 ( 4, 4 ),
 ( 0.000000000000000000, 9.999999999998900014E-05 ),
 .UNSPECIFIED. ) ;
#1481 = VECTOR ( 'NONE', #77699, 1000.000000000000114 ) ;
#1482 = CARTESIAN_POINT ( 'NONE',  ( 20.11976772532220181, -3.360927329567881205, 11.49999999999999645 ) ) ;
#1483 = CARTESIAN_POINT ( 'NONE',  ( -93.52287095715006160, -24.65952944569304606, 1.056160979905700570 ) ) ;
#1484 = DIRECTION ( 'NONE',  ( 0.000000000000000000, 2.173523156925980399E-06, -0.9999999999976378895 ) ) ;
#1485 = ORIENTED_EDGE ( 'NONE', *, *, #77012, .T. ) ;
#1486 = CARTESIAN_POINT ( 'NONE',  ( -78.94303308397306296, -25.26642230834568537, 5.977536689587218177 ) ) ;
#1487 = CARTESIAN_POINT ( 'NONE',  ( 33.62145766639996936, 4.037870770857261427, -12.08356088300365094 ) ) ;
#1488 = CARTESIAN_POINT ( 'NONE',  ( -114.2228709571500787, -23.47593901973090524, -1.443836447538996426 ) ) ;
#1489 = VECTOR ( 'NONE', #85606, 1000.000000000000114 ) ;
#1490 = LINE ( 'NONE', #39036, #63525 ) ;
#1491 = CARTESIAN_POINT ( 'NONE',  ( -129.5562042904833504, -23.48783264082478794, -1.443836473390056385 ) ) ;
#1492 = CARTESIAN_POINT ( 'NONE',  ( 15.17442925503088169, 13.16703847180013831, 11.49999999999998934 ) ) ;
#1493 = CYLINDRICAL_SURFACE ( 'NONE', #93750, 2.000000000000001776 ) ;
#1494 = ORIENTED_EDGE ( 'NONE', *, *, #83961, .F. ) ;
#1495 = DIRECTION ( 'NONE',  ( -1.000000000000000000, 0.000000000000000000, -0.000000000000000000 ) ) ;
#1496 = ADVANCED_FACE ( 'NONE', ( #91321 ), #60400, .F. ) ;
#1497 = CARTESIAN_POINT ( 'NONE',  ( 21.44032754495887261, 8.191337786432022483, 11.49999999999999645 ) ) ;
#1498 = CARTESIAN_POINT ( 'NONE',  ( -18.45961786539058380, -13.25243217869837231, 11.49999999999998934 ) ) ;
#1499 = VERTEX_POINT ( 'NONE', #44658 ) ;
#1500 = DIRECTION ( 'NONE',  ( 0.000000000000000000, -1.000000000000000000, 0.000000000000000000 ) ) ;
#1501 = CARTESIAN_POINT ( 'NONE',  ( -75.62287095715009855, -24.92604778743018556, 8.074972756849360778 ) ) ;
#1502 = CARTESIAN_POINT ( 'NONE',  ( -38.48524076036703434, -24.51419770103157347, 9.386484678747176957 ) ) ;
#1503 = CARTESIAN_POINT ( 'NONE',  ( -30.57287095715006231, -25.30570897125571861, 4.442708032791744088 ) ) ;
#1504 = EDGE_CURVE ( 'NONE', #11582, #65087, #6086, .T. ) ;
#1505 = CARTESIAN_POINT ( 'NONE',  ( -8.160000000000000142, -10.65233964170348635, -1.621096496867198589 ) ) ;
#1506 = CLOSED_SHELL ( 'NONE', ( #10304, #65184, #24838, #77619, #76239, #98548, #93754, #19318, #8575, #41539, #53116, #38460, #95025, #44284, #21171, #57020, #74206, #28690, #45159, #28308, #38824, #28481 ) ) ;
#1507 = CARTESIAN_POINT ( 'NONE',  ( -49.46084499080052410, -25.31520542434502730, 5.106140872684356680 ) ) ;
#1508 = CARTESIAN_POINT ( 'NONE',  ( -54.52287095715006870, -24.64898659630367916, 1.056161002820821038 ) ) ;
#1509 = CARTESIAN_POINT ( 'NONE',  ( -81.62287095715005592, -23.47593901973091235, -1.443836447539004642 ) ) ;
#1510 = EDGE_LOOP ( 'NONE', ( #95220, #92982, #52992, #14192 ) ) ;
#1511 = CARTESIAN_POINT ( 'NONE',  ( -17.41452279269062586, 10.58001483151439004, -1.500000000000002220 ) ) ;
#1512 = VERTEX_POINT ( 'NONE', #37038 ) ;
#1513 = CARTESIAN_POINT ( 'NONE',  ( -19.06187107478486098, -12.82570580458313003, 11.49999999999998934 ) ) ;
#1514 = CARTESIAN_POINT ( 'NONE',  ( -53.62287095715004881, -23.48786465467241058, 11.44779295918255002 ) ) ;
#1515 = ORIENTED_EDGE ( 'NONE', *, *, #56665, .F. ) ;
#1516 = LINE ( 'NONE', #93849, #47711 ) ;
#1517 = CARTESIAN_POINT ( 'NONE',  ( -99.62287095715005592, -24.64965695001468404, 8.947790433994178727 ) ) ;
#1518 = CARTESIAN_POINT ( 'NONE',  ( -96.62287095715005592, -24.64898659630368272, 1.056161002820829697 ) ) ;
#1520 = ORIENTED_EDGE ( 'NONE', *, *, #92917, .T. ) ;
#1519 = CARTESIAN_POINT ( 'NONE',  ( 21.14028111218437900, -2.610574537768086234, 11.49999999999999645 ) ) ;
#1521 = EDGE_LOOP ( 'NONE', ( #83273, #73807, #76093, #78613 ) ) ;
#1522 = CARTESIAN_POINT ( 'NONE',  ( -17.05807961832342912, 14.25954964135033265, 11.49999999999998934 ) ) ;
#1523 = B_SPLINE_CURVE_WITH_KNOTS ( 'NONE', 3,
 ( #7775, #8278, #64095, #47847, #24495, #24993, #31608, #39219, #62077, #86401, #17390, #16886, #48353, #40730, #85901, #70176, #79282, #9776, #33117, #54457, #71688, #56476, #95013, #38721, #78270, #2185 ),
 .UNSPECIFIED., .F., .F.,
 ( 4, 2, 2, 2, 2, 2, 2, 2, 2, 2, 2, 2, 4 ),
 ( 1.045815803166493187E-05, 0.001697191910848542444, 0.002540558787256983614, 0.003383925663665425000, 0.004227292540073865519, 0.005070659416482306038, 0.006757393169299188811, 0.007600760045707628462, 0.008444126922116070716, 0.01013086067493295175, 0.01097422755134139054, 0.01181759442774982932, 0.01350432818056671036 ),
 .UNSPECIFIED. ) ;
#1524 = CARTESIAN_POINT ( 'NONE',  ( 10.61356161029474521, 17.70173163822984819, 11.49999999999998934 ) ) ;
#1525 = ORIENTED_EDGE ( 'NONE', *, *, #47678, .F. ) ;
#1526 = CARTESIAN_POINT ( 'NONE',  ( -6.636054160061366503, -6.376774720514411854, 19.15289935703627933 ) ) ;
#1527 = CARTESIAN_POINT ( 'NONE',  ( -95.54445401090212897, -24.83644354573579349, 8.397322867130096569 ) ) ;
#1528 = VERTEX_POINT ( 'NONE', #98927 ) ;
#1529 = CARTESIAN_POINT ( 'NONE',  ( -95.52287095715004739, -24.51163499207179797, 0.6490370598555494919 ) ) ;
#1530 = CIRCLE ( 'NONE', #50136, 129.7684398600581517 ) ;
#1531 = ORIENTED_EDGE ( 'NONE', *, *, #27283, .F. ) ;
#1532 = CARTESIAN_POINT ( 'NONE',  ( -58.59839921736052304, -23.96169478059713143, 10.65365249895718058 ) ) ;
#1533 = CARTESIAN_POINT ( 'NONE',  ( 0.000000000000000000, 0.000000000000000000, 0.000000000000000000 ) ) ;
#1534 = CARTESIAN_POINT ( 'NONE',  ( -20.60679684081203789, -3.318877370925724879, -1.500000000000002220 ) ) ;
#1535 = CARTESIAN_POINT ( 'NONE',  ( -21.01659442711627790, -5.882202039844940167, 11.49999999999999645 ) ) ;
#1536 = CARTESIAN_POINT ( 'NONE',  ( 25.90238399655805424, -5.165317243602335573, -7.576880152980976391 ) ) ;
#1537 = DIRECTION ( 'NONE',  ( 0.000000000000000000, 1.000000000000000000, 0.000000000000000000 ) ) ;
#1538 = CARTESIAN_POINT ( 'NONE',  ( -17.89120377161202313, 13.61666483413312712, -1.500000000000002220 ) ) ;
#1539 = AXIS2_PLACEMENT_3D ( 'NONE', #3296, #82877, #51450 ) ;
#1540 = CARTESIAN_POINT ( 'NONE',  ( -44.52287095715006160, -24.64898659630367916, 1.056161002820819261 ) ) ;
#1541 = CARTESIAN_POINT ( 'NONE',  ( -53.62287095715005592, -24.64898659630528499, 1.056161002820821038 ) ) ;
#1542 = FACE_OUTER_BOUND ( 'NONE', #9586, .T. ) ;
#1543 = ORIENTED_EDGE ( 'NONE', *, *, #40430, .T. ) ;
#1544 = VECTOR ( 'NONE', #59527, 1000.000000000000114 ) ;
#1545 = EDGE_LOOP ( 'NONE', ( #3931, #75255, #37132, #55953 ) ) ;
#1546 = AXIS2_PLACEMENT_3D ( 'NONE', #67638, #58037, #97074 ) ;
#1547 = VERTEX_POINT ( 'NONE', #52769 ) ;
#1548 = CARTESIAN_POINT ( 'NONE',  ( 30.76755528059980804, -5.112846897994270279, -0.3209731499739113536 ) ) ;
#1549 = VERTEX_POINT ( 'NONE', #83706 ) ;
#1550 = AXIS2_PLACEMENT_3D ( 'NONE', #4421, #21116, #66832 ) ;
#1551 = CARTESIAN_POINT ( 'NONE',  ( 10.55508701655855575, -18.62573008410804221, -1.500000000000002220 ) ) ;
#1552 = CARTESIAN_POINT ( 'NONE',  ( 5.437191932089902480, -21.69250089042843754, 11.49999999999999645 ) ) ;
#1553 = VERTEX_POINT ( 'NONE', #35052 ) ;
#1554 = CARTESIAN_POINT ( 'NONE',  ( -43.62287095715004881, -24.64898659630367206, 1.056161002820819261 ) ) ;
#1555 = CARTESIAN_POINT ( 'NONE',  ( 16.02493003730957000, -13.65669227992738577, -1.500000000000002220 ) ) ;
#1556 = CARTESIAN_POINT ( 'NONE',  ( -30.43720465287918131, -24.37652013707292298, 9.702671485061733492 ) ) ;
#1557 = EDGE_CURVE ( 'NONE', #49884, #2918, #50780, .T. ) ;
#1558 = CARTESIAN_POINT ( 'NONE',  ( -19.24466553037914807, -5.328869878250761971, -1.500000000000002220 ) ) ;
#1559 = CARTESIAN_POINT ( 'NONE',  ( 7.160000000000000142, -9.123836073446797812, -2.666350264951732552 ) ) ;
#1560 = CARTESIAN_POINT ( 'NONE',  ( 2.935461252226840401, -5.876774720514419847, 20.47627681611744777 ) ) ;
#1561 = CARTESIAN_POINT ( 'NONE',  ( -19.65368394218270254, -10.04821906498216499, -1.500000000000002220 ) ) ;
#1562 = DIRECTION ( 'NONE',  ( -3.773278334444166432E-23, 1.000000000000000000, 0.000000000000000000 ) ) ;
#1563 = ORIENTED_EDGE ( 'NONE', *, *, #34195, .F. ) ;
#1564 = CARTESIAN_POINT ( 'NONE',  ( -65.65276306346875401, -23.85049219812685806, 10.88485053497527311 ) ) ;
#1565 = EDGE_CURVE ( 'NONE', #12606, #15278, #66525, .T. ) ;
#1566 = LINE ( 'NONE', #8166, #98361 ) ;
#1567 = CARTESIAN_POINT ( 'NONE',  ( 8.688630223215852766, -18.96179456382524364, 11.49999999999999645 ) ) ;
#1568 = EDGE_CURVE ( 'NONE', #47577, #88761, #77083, .T. ) ;
#1569 = CARTESIAN_POINT ( 'NONE',  ( 29.60459817610514932, -4.854569207680477838, 28.81138945959710185 ) ) ;
#1570 = ADVANCED_FACE ( 'NONE', ( #53272 ), #23893, .T. ) ;
#1571 = PLANE ( 'NONE',  #92693 ) ;
#1572 = CARTESIAN_POINT ( 'NONE',  ( -38.62287095715007013, -23.73934037231757088, 11.05740245334329863 ) ) ;
#1573 = CARTESIAN_POINT ( 'NONE',  ( -9.236746577462426444, 19.23066362772381055, 11.49999999999998934 ) ) ;
#1574 = PLANE ( 'NONE',  #33711 ) ;
#1575 = EDGE_CURVE ( 'NONE', #63086, #27656, #38036, .T. ) ;
#1576 = CARTESIAN_POINT ( 'NONE',  ( -80.52287095715004739, -25.00182538069145366, 7.747789668545104647 ) ) ;
#1577 = CARTESIAN_POINT ( 'NONE',  ( -96.52287095715001897, -24.51387760970724727, 9.387446482453407626 ) ) ;
#1578 = DIRECTION ( 'NONE',  ( -0.9952638024365005887, 0.000000000000000000, -0.09721092304694052555 ) ) ;
#1579 = CARTESIAN_POINT ( 'NONE',  ( -10.06026007034034464, -20.14757889648583244, -1.500000000000002220 ) ) ;
#1580 = CARTESIAN_POINT ( 'NONE',  ( 3.750000000000001332, 25.69999999999999574, 2.100000000000000089 ) ) ;
#1581 = ORIENTED_EDGE ( 'NONE', *, *, #99852, .F. ) ;
#1582 = LINE ( 'NONE', #71593, #74186 ) ;
#1583 = CARTESIAN_POINT ( 'NONE',  ( -31.56131522125139810, -23.73791477778911130, 11.05961554403171299 ) ) ;
#1584 = CARTESIAN_POINT ( 'NONE',  ( 15.21843288076463629, 12.49332292251147614, 11.49999999999999645 ) ) ;
#1585 = DIRECTION ( 'NONE',  ( 1.000000000000000000, -4.088963247170718308E-15, 0.000000000000000000 ) ) ;
#1586 = DIRECTION ( 'NONE',  ( -3.773278334453079618E-23, 0.9999999999976377785, 2.173523156925979975E-06 ) ) ;
#1587 = EDGE_CURVE ( 'NONE', #11601, #66619, #27923, .T. ) ;
#1588 = VERTEX_POINT ( 'NONE', #99909 ) ;
#1589 = DIRECTION ( 'NONE',  ( 1.000000000000000000, 0.000000000000000000, 0.000000000000000000 ) ) ;
#1590 = DIRECTION ( 'NONE',  ( -0.6599726524652352877, 0.000000000000000000, 0.7512896232465892110 ) ) ;
#1591 = CARTESIAN_POINT ( 'NONE',  ( -61.52287095715006160, -24.66019654487199730, 8.947790411086121054 ) ) ;
#1592 = DIRECTION ( 'NONE',  ( -0.000000000000000000, 0.000000000000000000, 1.000000000000000000 ) ) ;
#1593 = CARTESIAN_POINT ( 'NONE',  ( -5.448126336921106372, -18.99418723138115084, 11.49999999999998934 ) ) ;
#1594 = ORIENTED_EDGE ( 'NONE', *, *, #48663, .F. ) ;
#1595 = CARTESIAN_POINT ( 'NONE',  ( 9.409760114191467295, 17.86087837679851020, 11.49999999999999645 ) ) ;
#1596 = CARTESIAN_POINT ( 'NONE',  ( 12.30588647384254841, 6.376774720514765349, -28.11066263748569227 ) ) ;
#1597 = VECTOR ( 'NONE', #80561, 1000.000000000000114 ) ;
#1598 = VERTEX_POINT ( 'NONE', #24310 ) ;
#1599 = CARTESIAN_POINT ( 'NONE',  ( -48.62287095715006302, -24.33927499327853994, 9.819080762295820719 ) ) ;
#1600 = CARTESIAN_POINT ( 'NONE',  ( -69.86951118291817409, -25.29879079004132336, 5.410841093910524258 ) ) ;
#1601 = CARTESIAN_POINT ( 'NONE',  ( -50.72512992191887804, -25.30333624419147043, 5.237440092667283054 ) ) ;
#1602 = CARTESIAN_POINT ( 'NONE',  ( -71.20541289166536103, -25.30502758240210071, 4.885889971059796721 ) ) ;
#1603 = AXIS2_PLACEMENT_3D ( 'NONE', #38165, #53914, #84847 ) ;
#1604 = CARTESIAN_POINT ( 'NONE',  ( -41.62287095715006302, -24.66019654487199020, 8.947790411086135265 ) ) ;
#1605 = CARTESIAN_POINT ( 'NONE',  ( -127.5228709571500616, -24.65952944569304606, 1.056160979905707675 ) ) ;
#1606 = CARTESIAN_POINT ( 'NONE',  ( -20.00956492049148494, -0.6725752471728385640, -1.500000000000002220 ) ) ;
#1607 = EDGE_CURVE ( 'NONE', #3816, #73248, #16945, .T. ) ;
#1608 = CARTESIAN_POINT ( 'NONE',  ( -117.5562042904833788, -24.64898659630529210, 1.056161002820830142 ) ) ;
#1609 = CARTESIAN_POINT ( 'NONE',  ( -116.5892947015510259, -24.35071581493544102, 9.817618358456021710 ) ) ;
#1610 = ORIENTED_EDGE ( 'NONE', *, *, #18664, .F. ) ;
#1611 = CIRCLE ( 'NONE', #19412, 2.499999999999995115 ) ;
#1612 = AXIS2_PLACEMENT_3D ( 'NONE', #15470, #91600, #22078 ) ;
#1613 = CARTESIAN_POINT ( 'NONE',  ( 10.86929179853872007, -4.313324117933219348, -26.78630334068696683 ) ) ;
#1614 = CARTESIAN_POINT ( 'NONE',  ( -109.4679719608024300, -25.18430259236162172, 3.778970299867911109 ) ) ;
#1615 = CARTESIAN_POINT ( 'NONE',  ( -35.52469202473817234, -24.83618233451450052, 1.606449574219543708 ) ) ;
#1616 = CARTESIAN_POINT ( 'NONE',  ( -28.62287095715004881, -23.80673410051091921, 10.65359467416498163 ) ) ;
#1617 = AXIS2_PLACEMENT_3D ( 'NONE', #35698, #42821, #90475 ) ;
#1618 = PLANE ( 'NONE',  #35085 ) ;
#1619 = PLANE ( 'NONE',  #50199 ) ;
#1620 = B_SPLINE_CURVE_WITH_KNOTS ( 'NONE', 3,
 ( #19979, #10879, #50948, #54321, #30467, #23846, #8139, #76622, #7124, #20471, #59558, #99956, #31467, #51442, #98090, #54820 ),
 .UNSPECIFIED., .F., .F.,
 ( 4, 2, 2, 2, 2, 2, 2, 4 ),
 ( 0.000000000000000000, 0.0002054542984747955402, 0.0004109085969495910803, 0.0008218171938991786912, 0.001027271492373979002, 0.001232725790848779313, 0.001438180089323579623, 0.001643634387798379934 ),
 .UNSPECIFIED. ) ;
#1621 = AXIS2_PLACEMENT_3D ( 'NONE', #78289, #62588, #52980 ) ;
#1622 = DIRECTION ( 'NONE',  ( -0.000000000000000000, 1.000000000000000000, -0.000000000000000000 ) ) ;
#1623 = EDGE_CURVE ( 'NONE', #49734, #5271, #54777, .T. ) ;
#1624 = CARTESIAN_POINT ( 'NONE',  ( -50.29888690743871393, -25.18523929458199007, 3.296129346514034442 ) ) ;
#1625 = ORIENTED_EDGE ( 'NONE', *, *, #62565, .T. ) ;
#1626 = CARTESIAN_POINT ( 'NONE',  ( 9.679018533540549640, -17.85022214266596308, 11.49999999999998934 ) ) ;
#1627 = EDGE_CURVE ( 'NONE', #80644, #84008, #23034, .T. ) ;
#1628 = CARTESIAN_POINT ( 'NONE',  ( -28.52287095715005805, -24.49893655963190042, 1.056161680022248195 ) ) ;
#1629 = PLANE ( 'NONE',  #59842 ) ;
#1630 = CARTESIAN_POINT ( 'NONE',  ( -59.59827874889279542, -23.96169478059713143, 10.65365249895718769 ) ) ;
#1631 = ORIENTED_EDGE ( 'NONE', *, *, #13267, .T. ) ;
#1632 = CARTESIAN_POINT ( 'NONE',  ( -81.62287095715008434, -24.51283580621364777, 0.6167428607019832532 ) ) ;
#1633 = CARTESIAN_POINT ( 'NONE',  ( -10.68008619461380704, -17.10268970254769982, -1.500000000000002220 ) ) ;
#1634 = CARTESIAN_POINT ( 'NONE',  ( 12.34367313097222763, -17.18290682204727915, 11.49999999999999645 ) ) ;
#1635 = CARTESIAN_POINT ( 'NONE',  ( 4.116201370682176730, 21.75534844777131838, 11.49999999999998934 ) ) ;
#1636 = CARTESIAN_POINT ( 'NONE',  ( -9.016818060619870678, -18.48156098877705844, 11.49999999999998934 ) ) ;
#1637 = CARTESIAN_POINT ( 'NONE',  ( 6.944081373883786767, -5.876774720514424288, 21.27829155525578031 ) ) ;
#1638 = ORIENTED_EDGE ( 'NONE', *, *, #39342, .F. ) ;
#1639 = DIRECTION ( 'NONE',  ( -1.000000000000000000, -0.000000000000000000, -0.000000000000000000 ) ) ;
#1640 = ORIENTED_EDGE ( 'NONE', *, *, #69436, .T. ) ;
#1641 = CARTESIAN_POINT ( 'NONE',  ( -125.6228709571500559, -29.50249982740957577, 7.747779886224967605 ) ) ;
#1642 = CARTESIAN_POINT ( 'NONE',  ( -129.6228709571500417, -23.47593901973091235, -1.443836447538995760 ) ) ;
#1643 = VERTEX_POINT ( 'NONE', #40549 ) ;
#1644 = ORIENTED_EDGE ( 'NONE', *, *, #20223, .T. ) ;
#1645 = VERTEX_POINT ( 'NONE', #32930 ) ;
#1646 = CARTESIAN_POINT ( 'NONE',  ( -111.2197402010974656, -25.17156514485315455, 3.135139282531213656 ) ) ;
#1647 = CARTESIAN_POINT ( 'NONE',  ( 7.087697398486194622, -5.876774720514418071, 20.45710073441444621 ) ) ;
#1648 = CARTESIAN_POINT ( 'NONE',  ( 29.73860345376319003, 1.477225279485574028, 19.84760796525321425 ) ) ;
#1649 = CARTESIAN_POINT ( 'NONE',  ( -19.90621922972506397, 5.769413876575915978, -1.500000000000002220 ) ) ;
#1650 = CARTESIAN_POINT ( 'NONE',  ( -10.61912389536305490, -18.88692380039396213, 11.49999999999999645 ) ) ;
#1651 = ORIENTED_EDGE ( 'NONE', *, *, #34205, .T. ) ;
#1652 = CARTESIAN_POINT ( 'NONE',  ( -99.01182976505512556, -25.29312185475552965, 5.556534405804150367 ) ) ;
#1653 = CARTESIAN_POINT ( 'NONE',  ( 2.710830299132254595, -5.876774720514410966, 19.05039662921485544 ) ) ;
#1654 = CARTESIAN_POINT ( 'NONE',  ( 18.93296920960566965, -11.98514031388154599, -1.500000000000002220 ) ) ;
#1655 = CARTESIAN_POINT ( 'NONE',  ( -47.63994631694639281, -24.15620529776627379, 10.23563542870660825 ) ) ;
#1656 = CARTESIAN_POINT ( 'NONE',  ( -90.62287095715004170, -29.50248528299804818, 1.056150453629040253 ) ) ;
#1657 = VERTEX_POINT ( 'NONE', #88224 ) ;
#1658 = CARTESIAN_POINT ( 'NONE',  ( 29.60442047479375205, 4.849628492681046232, 28.81422082199668466 ) ) ;
#1659 = CARTESIAN_POINT ( 'NONE',  ( -35.58102505592412257, -24.73531770709095667, 8.716586749053508498 ) ) ;
#1660 = B_SPLINE_CURVE_WITH_KNOTS ( 'NONE', 3,
 ( #20022, #35264, #58593, #60106 ),
 .UNSPECIFIED., .F., .F.,
 ( 4, 4 ),
 ( 0.000000000000000000, 9.999999999998897304E-05 ),
 .UNSPECIFIED. ) ;
#1661 = ORIENTED_EDGE ( 'NONE', *, *, #46484, .T. ) ;
#1662 = ORIENTED_EDGE ( 'NONE', *, *, #54377, .T. ) ;
#1663 = CIRCLE ( 'NONE', #43810, 28.96799999999999287 ) ;
#1664 = CARTESIAN_POINT ( 'NONE',  ( -43.52287095715006160, -23.47596703998600631, 11.44779298504229281 ) ) ;
#1665 = ORIENTED_EDGE ( 'NONE', *, *, #86622, .F. ) ;
#1666 = DIRECTION ( 'NONE',  ( 0.000000000000000000, -2.173523156925980399E-06, 0.9999999999976378895 ) ) ;
#1667 = CARTESIAN_POINT ( 'NONE',  ( -14.68016216564755894, -15.32010671487267572, -1.500000000000002220 ) ) ;
#1668 = ORIENTED_EDGE ( 'NONE', *, *, #36947, .T. ) ;
#1669 = CARTESIAN_POINT ( 'NONE',  ( -50.54317153895161141, -24.40034930558990922, 0.3402023900116070698 ) ) ;
#1670 = CARTESIAN_POINT ( 'NONE',  ( -21.69466673205137752, 2.402554924997643226, 11.49999999999998934 ) ) ;
#1671 = CARTESIAN_POINT ( 'NONE',  ( -103.5909352260227934, -24.15620529776628445, 10.23563542870660292 ) ) ;
#1672 = AXIS2_PLACEMENT_3D ( 'NONE', #11370, #57563, #88500 ) ;
#1673 = CARTESIAN_POINT ( 'NONE',  ( -43.62287095715004881, -24.64965695001467694, 8.947790433994187609 ) ) ;
#1674 = DIRECTION ( 'NONE',  ( 0.06916465693916189206, 0.000000000000000000, -0.9976052577199502336 ) ) ;
#1675 = CARTESIAN_POINT ( 'NONE',  ( 21.67628855941699939, -2.339797445609365756, -1.500000000000002220 ) ) ;
#1676 = CARTESIAN_POINT ( 'NONE',  ( -95.62287095715005592, -25.00158670708909625, 2.256160236439165967 ) ) ;
#1677 = ORIENTED_EDGE ( 'NONE', *, *, #1568, .T. ) ;
#1678 = CARTESIAN_POINT ( 'NONE',  ( 26.73860345374794534, 5.058662225110310828, -7.113848178280766099 ) ) ;
#1679 = CARTESIAN_POINT ( 'NONE',  ( -85.60107928363679264, -23.85049219812685450, 10.88485053497527133 ) ) ;
#1680 = VERTEX_POINT ( 'NONE', #79596 ) ;
#1681 = EDGE_LOOP ( 'NONE', ( #38410, #9651, #53587, #76774 ) ) ;
#1682 = AXIS2_PLACEMENT_3D ( 'NONE', #43986, #21135, #36874 ) ;
#1683 = EDGE_LOOP ( 'NONE', ( #83248, #93624, #3389, #39960, #41208, #59557 ) ) ;
#1684 = EDGE_CURVE ( 'NONE', #89148, #95501, #12089, .T. ) ;
#1685 = DIRECTION ( 'NONE',  ( 0.000000000000000000, 2.173523156925980399E-06, -0.9999999999976378895 ) ) ;
#1686 = CIRCLE ( 'NONE', #87586, 2.399999999999999911 ) ;
#1687 = CARTESIAN_POINT ( 'NONE',  ( -31.24388727629347784, -24.87219037989215309, 1.747789950310770779 ) ) ;
#1688 = CARTESIAN_POINT ( 'NONE',  ( 20.00388196354723291, 7.160935007556333609, 11.49999999999998934 ) ) ;
#1689 = CARTESIAN_POINT ( 'NONE',  ( 7.480769230769231726, -6.376774720514420736, 20.77403846153845635 ) ) ;
#1690 = EDGE_CURVE ( 'NONE', #80236, #95482, #59378, .T. ) ;
#1691 = DIRECTION ( 'NONE',  ( -0.000000000000000000, 1.000000000000000000, -0.000000000000000000 ) ) ;
#1692 = CARTESIAN_POINT ( 'NONE',  ( -44.62287095715004881, -23.48786465467240347, 11.44779295918255180 ) ) ;
#1693 = FACE_OUTER_BOUND ( 'NONE', #83972, .T. ) ;
#1694 = VECTOR ( 'NONE', #11060, 1000.000000000000114 ) ;
#1695 = CARTESIAN_POINT ( 'NONE',  ( -4.539579955115475407, -18.87035741768621122, -1.500000000000002220 ) ) ;
#1696 = B_SPLINE_CURVE_WITH_KNOTS ( 'NONE', 3,
 ( #29358, #69428, #100346, #60335, #30862, #91258 ),
 .UNSPECIFIED., .F., .F.,
 ( 4, 2, 4 ),
 ( 0.000000000000000000, 0.001380764517854765399, 0.002761529035709530365 ),
 .UNSPECIFIED. ) ;
#1697 = CARTESIAN_POINT ( 'NONE',  ( -45.65169983139999488, -24.15503026093915651, -0.2815557561904415418 ) ) ;
#1698 = ORIENTED_EDGE ( 'NONE', *, *, #40048, .F. ) ;
#1699 = AXIS2_PLACEMENT_3D ( 'NONE', #77975, #1388, #877 ) ;
#1700 = CARTESIAN_POINT ( 'NONE',  ( 3.395600993332231532, 19.23619202488179525, 11.49999999999999645 ) ) ;
#1701 = CARTESIAN_POINT ( 'NONE',  ( 31.63207147031214106, -3.934018429836814601, 27.19231918963763661 ) ) ;
#1702 = CARTESIAN_POINT ( 'NONE',  ( 17.51792015816173986, 0.3587747205144265483, 29.01255224319336889 ) ) ;
#1703 = EDGE_CURVE ( 'NONE', #93093, #13092, #31505, .T. ) ;
#1704 = ORIENTED_EDGE ( 'NONE', *, *, #4133, .T. ) ;
#1705 = CARTESIAN_POINT ( 'NONE',  ( 4.910384361841649614, -5.876774720514419847, 20.73924463800384643 ) ) ;
#1706 = CARTESIAN_POINT ( 'NONE',  ( -89.62590769665170853, -24.51314013834317151, 0.6176544820404251679 ) ) ;
#1707 = CARTESIAN_POINT ( 'NONE',  ( 11.62916340711181284, -0.3587747205144265483, 28.75961759920349792 ) ) ;
#1708 = CARTESIAN_POINT ( 'NONE',  ( -20.27875734969026311, -6.143225279485574397, 24.00402280011862288 ) ) ;
#1709 = CARTESIAN_POINT ( 'NONE',  ( 18.74904333037421011, -5.873301551693434597, 11.49999999999998934 ) ) ;
#1710 = ORIENTED_EDGE ( 'NONE', *, *, #76950, .F. ) ;
#1711 = LINE ( 'NONE', #94044, #69902 ) ;
#1712 = CARTESIAN_POINT ( 'NONE',  ( 20.31487730549432413, -11.01532776123576518, -1.500000000000002220 ) ) ;
#1713 = APPROVAL_STATUS ( 'not_yet_approved' ) ;
#1714 = CARTESIAN_POINT ( 'NONE',  ( -125.5228709571500048, -24.63345952396256067, 9.038047939301506517 ) ) ;
#1715 = CARTESIAN_POINT ( 'NONE',  ( 4.487249349319938574, -6.376774720514420736, 21.01618089687719504 ) ) ;
#1716 = CARTESIAN_POINT ( 'NONE',  ( -97.51896304891869249, -23.73791477778912196, 11.05961554403170410 ) ) ;
#1717 = LINE ( 'NONE', #9820, #11057 ) ;
#1718 = CARTESIAN_POINT ( 'NONE',  ( 5.727631217150810805, -6.376774720514422512, 21.11407618546790133 ) ) ;
#1719 = CARTESIAN_POINT ( 'NONE',  ( -129.5897716341975467, -24.15543982623907837, -0.2315651400026527140 ) ) ;
#1720 = CARTESIAN_POINT ( 'NONE',  ( -114.6292354253845929, -23.73791477778912551, 11.05961554403169878 ) ) ;
#1721 = CARTESIAN_POINT ( 'NONE',  ( 10.08953278062578462, 17.19620541797624824, 11.49999999999998934 ) ) ;
#1722 = CARTESIAN_POINT ( 'NONE',  ( -75.58061766105404899, -24.92592662359561473, 8.075495903018000021 ) ) ;
#1723 = CARTESIAN_POINT ( 'NONE',  ( 0.4224338394261131779, -19.80333402765648998, -1.500000000000002220 ) ) ;
#1724 = ORIENTED_EDGE ( 'NONE', *, *, #96724, .T. ) ;
#1725 = CARTESIAN_POINT ( 'NONE',  ( -32.50560602629348494, -24.87219037988797865, 1.747789950295646877 ) ) ;
#1726 = EDGE_CURVE ( 'NONE', #35033, #10968, #71419, .T. ) ;
#1727 = CARTESIAN_POINT ( 'NONE',  ( -51.51937581801175270, -25.24378128350642925, 6.324045589363499253 ) ) ;
#1728 = CARTESIAN_POINT ( 'NONE',  ( -12.26507114386991226, -16.75673120704366426, 11.49999999999999645 ) ) ;
#1729 = LINE ( 'NONE', #32669, #69431 ) ;
#1730 = B_SPLINE_CURVE_WITH_KNOTS ( 'NONE', 3,
 ( #83994, #99211, #14477, #76368 ),
 .UNSPECIFIED., .F., .F.,
 ( 4, 4 ),
 ( 0.000000000000000000, 1.000000000000000000 ),
 .UNSPECIFIED. ) ;
#1731 = VECTOR ( 'NONE', #34361, 1000.000000000000000 ) ;
#1732 = ADVANCED_FACE ( 'NONE', ( #25814 ), #16617, .T. ) ;
#1733 = CARTESIAN_POINT ( 'NONE',  ( -78.52287095715006160, -24.50321055353803956, 9.387540953477513384 ) ) ;
#1734 = CARTESIAN_POINT ( 'NONE',  ( 0.8422786845129024424, 22.77647355728978340, 11.49999999999999645 ) ) ;
#1735 = ORIENTED_EDGE ( 'NONE', *, *, #33658, .T. ) ;
#1736 = CARTESIAN_POINT ( 'NONE',  ( -69.51616565026102990, -23.73766607897669445, -1.055555164236460008 ) ) ;
#1737 = CARTESIAN_POINT ( 'NONE',  ( -89.52287095715006160, -23.47596703998600631, 11.44779298504228393 ) ) ;
#1738 = ORIENTED_EDGE ( 'NONE', *, *, #3191, .F. ) ;
#1739 = CARTESIAN_POINT ( 'NONE',  ( -13.29518446780263119, -15.22762515321373478, -1.500000000000002220 ) ) ;
#1740 = DIRECTION ( 'NONE',  ( 0.000000000000000000, -1.478457507934778393E-16, -1.000000000000000000 ) ) ;
#1741 = CARTESIAN_POINT ( 'NONE',  ( -110.5228709571500616, -23.48786465467242479, 11.44779295918253936 ) ) ;
#1742 = ORIENTED_EDGE ( 'NONE', *, *, #17484, .T. ) ;
#1743 = CARTESIAN_POINT ( 'NONE',  ( -70.62287095715008434, -24.62285846362215835, 9.038163152653524435 ) ) ;
#1744 = CARTESIAN_POINT ( 'NONE',  ( -21.95939045666098366, -6.591442671832903777, 11.49999999999998934 ) ) ;
#1745 = CARTESIAN_POINT ( 'NONE',  ( -10.27747606359964117, 6.067502657846070235, 28.80925224784997596 ) ) ;
#1746 = VECTOR ( 'NONE', #69, 1000.000000000000114 ) ;
#1747 = CARTESIAN_POINT ( 'NONE',  ( 19.86680303116296287, 2.261939200664708327, -1.500000000000002220 ) ) ;
#1748 = CARTESIAN_POINT ( 'NONE',  ( -41.16195530322320195, -25.06433851276720048, 7.413582136084253094 ) ) ;
#1749 = CARTESIAN_POINT ( 'NONE',  ( 14.09988904737591575, 15.55221489148801872, 11.49999999999999645 ) ) ;
#1750 = VECTOR ( 'NONE', #88379, 1000.000000000000114 ) ;
#1751 = CARTESIAN_POINT ( 'NONE',  ( -29.25979817829156815, -24.97066910737833112, 7.423742159896792536 ) ) ;
#1752 = CARTESIAN_POINT ( 'NONE',  ( -124.5541598730913933, -24.65952944569305316, 1.056160979905707009 ) ) ;
#1753 = CARTESIAN_POINT ( 'NONE',  ( -5.561696574893697509, -21.35426480686918538, -1.500000000000002220 ) ) ;
#1754 = EDGE_CURVE ( 'NONE', #77182, #33349, #89562, .T. ) ;
#1755 = DIRECTION ( 'NONE',  ( 0.000000000000000000, 0.000000000000000000, 1.000000000000000000 ) ) ;
#1756 = VERTEX_POINT ( 'NONE', #82951 ) ;
#1757 = CARTESIAN_POINT ( 'NONE',  ( -87.62287095715004170, -29.50250243563736774, 8.947779886222139822 ) ) ;
#1758 = CYLINDRICAL_SURFACE ( 'NONE', #23351, 2.499999999999995115 ) ;
#1759 = CARTESIAN_POINT ( 'NONE',  ( 5.271800844963591359, -6.376774720514426953, -28.56638892015329034 ) ) ;
#1760 = ORIENTED_EDGE ( 'NONE', *, *, #45425, .T. ) ;
#1761 = CARTESIAN_POINT ( 'NONE',  ( -55.52287095715005449, -24.99156044556119483, 7.747789690856173195 ) ) ;
#1762 = VERTEX_POINT ( 'NONE', #83454 ) ;
#1763 = VERTEX_POINT ( 'NONE', #13444 ) ;
#1764 = DIRECTION ( 'NONE',  ( -0.000000000000000000, 1.000000000000000000, -0.000000000000000000 ) ) ;
#1765 = CARTESIAN_POINT ( 'NONE',  ( -47.62287095715004881, -29.50248528299804818, 1.056150453629033370 ) ) ;
#1766 = DIRECTION ( 'NONE',  ( -0.000000000000000000, 0.000000000000000000, -1.000000000000000000 ) ) ;
#1767 = CARTESIAN_POINT ( 'NONE',  ( 7.805751503010069037, -19.01748540344778959, -1.500000000000002220 ) ) ;
#1768 = ORIENTED_EDGE ( 'NONE', *, *, #85282, .T. ) ;
#1769 = CARTESIAN_POINT ( 'NONE',  ( -11.16000000000000014, -10.65233964170348635, -1.621096496867199033 ) ) ;
#1770 = EDGE_CURVE ( 'NONE', #62104, #35157, #76825, .T. ) ;
#1771 = CARTESIAN_POINT ( 'NONE',  ( -33.62287095715004170, -24.51387760970722596, 9.387446482453418284 ) ) ;
#1772 = DIRECTION ( 'NONE',  ( 0.000000000000000000, -1.000000000000000000, 0.000000000000000000 ) ) ;
#1773 = CARTESIAN_POINT ( 'NONE',  ( -5.617636847906702258, 21.56867655435222630, 11.49999999999998934 ) ) ;
#1774 = CARTESIAN_POINT ( 'NONE',  ( -0.07952141725841589681, -22.02053276243675484, 9.703205396196686650 ) ) ;
#1775 = CARTESIAN_POINT ( 'NONE',  ( -26.97150317964156585, -24.62069184369231678, 8.115489842150878985 ) ) ;
#1776 = VERTEX_POINT ( 'NONE', #37298 ) ;
#1777 = PLANE ( 'NONE',  #19270 ) ;
#1778 = B_SPLINE_CURVE_WITH_KNOTS ( 'NONE', 3,
 ( #96398, #43119, #74068, #4562 ),
 .UNSPECIFIED., .F., .F.,
 ( 4, 4 ),
 ( 0.000000000000000000, 0.0001000000000000028644 ),
 .UNSPECIFIED. ) ;
#1779 = CARTESIAN_POINT ( 'NONE',  ( -4.926336369345164279, -5.965225279485592225, -28.61095484066304451 ) ) ;
#1780 = CARTESIAN_POINT ( 'NONE',  ( -8.730572200882948053, 18.91488879456464289, 11.49999999999998934 ) ) ;
#1781 = VERTEX_POINT ( 'NONE', #13943 ) ;
#1783 = EDGE_LOOP ( 'NONE', ( #71632, #89413, #23011, #37714 ) ) ;
#1782 = LINE ( 'NONE', #47960, #73331 ) ;
#1785 = ORIENTED_EDGE ( 'NONE', *, *, #5898, .F. ) ;
#1784 = B_SPLINE_CURVE_WITH_KNOTS ( 'NONE', 3,
 ( #86990, #80886, #56567, #41327, #71278, #48446 ),
 .UNSPECIFIED., .F., .F.,
 ( 4, 2, 4 ),
 ( 0.000000000000000000, 0.001380901958385388545, 0.002761803916770777089 ),
 .UNSPECIFIED. ) ;
#1786 = CARTESIAN_POINT ( 'NONE',  ( -69.11592688286732766, -25.03149225412030177, 6.884840797962249681 ) ) ;
#1787 = CARTESIAN_POINT ( 'NONE',  ( 8.294003578737715543, -19.35633765900385939, -1.500000000000002220 ) ) ;
#1788 = ORIENTED_EDGE ( 'NONE', *, *, #96771, .F. ) ;
#1789 = CARTESIAN_POINT ( 'NONE',  ( 5.251006604497604258, -6.376774720514426953, -25.47015536487705489 ) ) ;
#1790 = CARTESIAN_POINT ( 'NONE',  ( 5.097264368844747651, -3.299463065352477908, -27.56135813788838718 ) ) ;
#1791 = CARTESIAN_POINT ( 'NONE',  ( -97.52287095715006160, -23.47596703998600631, 11.44779298504228215 ) ) ;
#1792 = CARTESIAN_POINT ( 'NONE',  ( -101.9195342205254775, -25.25419299847218468, 6.392810396799463390 ) ) ;
#1793 = EDGE_CURVE ( 'NONE', #6687, #64842, #68245, .T. ) ;
#1794 = B_SPLINE_CURVE_WITH_KNOTS ( 'NONE', 3,
 ( #82211, #21299, #66026, #13185 ),
 .UNSPECIFIED., .F., .F.,
 ( 4, 4 ),
 ( 0.000000000000000000, 9.999999999997510880E-05 ),
 .UNSPECIFIED. ) ;
#1795 = CARTESIAN_POINT ( 'NONE',  ( -59.48968306854239074, -24.65952944569304961, 1.056160979905697905 ) ) ;
#1796 = CARTESIAN_POINT ( 'NONE',  ( -109.3416230908480031, -25.31488395161200700, 5.187544736971523740 ) ) ;
#1797 = CARTESIAN_POINT ( 'NONE',  ( -118.2228709571500787, -23.47596703998600631, 11.44779298504227860 ) ) ;
#1798 = EDGE_CURVE ( 'NONE', #95755, #60161, #33850, .T. ) ;
#1800 = ORIENTED_EDGE ( 'NONE', *, *, #82331, .F. ) ;
#1799 = CARTESIAN_POINT ( 'NONE',  ( -19.06252244145942498, 11.34236556261432405, 11.49999999999999645 ) ) ;
#1801 = CARTESIAN_POINT ( 'NONE',  ( 29.80070917940689768, -3.316774720514426456, 27.39560796525317343 ) ) ;
#1802 = CARTESIAN_POINT ( 'NONE',  ( -87.52287095715006160, -23.96127896942116564, -0.6493128930942591026 ) ) ;
#1803 = ORIENTED_EDGE ( 'NONE', *, *, #95268, .T. ) ;
#1804 = CARTESIAN_POINT ( 'NONE',  ( 4.697487806458584991, -22.17256498326293013, -1.500000000000002220 ) ) ;
#1806 = ORIENTED_EDGE ( 'NONE', *, *, #54260, .T. ) ;
#1805 = CARTESIAN_POINT ( 'NONE',  ( -0.02075734969026423599, 5.866774720514426278, -0.08597719988137648983 ) ) ;
#1807 = ORIENTED_EDGE ( 'NONE', *, *, #90904, .F. ) ;
#1808 = CARTESIAN_POINT ( 'NONE',  ( 10.24059822343757808, -5.876774720514426953, 22.08128695274315945 ) ) ;
#1809 = AXIS2_PLACEMENT_3D ( 'NONE', #23005, #15407, #46368 ) ;
#1810 = ADVANCED_FACE ( 'NONE', ( #100153 ), #60151, .T. ) ;
#1811 = CARTESIAN_POINT ( 'NONE',  ( 17.50376878386636292, -9.983289808088789741, -1.500000000000002220 ) ) ;
#1812 = EDGE_CURVE ( 'NONE', #21561, #1208, #61144, .T. ) ;
#1813 = CARTESIAN_POINT ( 'NONE',  ( -84.22287095715007865, -23.47596703998600276, 11.44779298504227683 ) ) ;
#1814 = ORIENTED_EDGE ( 'NONE', *, *, #51149, .F. ) ;
#1815 = CARTESIAN_POINT ( 'NONE',  ( -8.160000000000000142, -10.15233964170348457, 1.310587897985993955 ) ) ;
#1816 = CARTESIAN_POINT ( 'NONE',  ( 10.13505985054399083, -19.98934331558005439, -1.500000000000002220 ) ) ;
#1817 = B_SPLINE_CURVE_WITH_KNOTS ( 'NONE', 3,
 ( #51353, #72200, #35632, #11288, #82294, #26521, #33631, #97517, #12273, #80806, #18893, #95526, #73688, #12772 ),
 .UNSPECIFIED., .F., .F.,
 ( 4, 2, 2, 2, 2, 2, 4 ),
 ( 0.000000000000000000, 0.002392375077555367480, 0.003588562616333051004, 0.004784750155110734093, 0.005980937693888416749, 0.007177125232666099405, 0.009569500310221466452 ),
 .UNSPECIFIED. ) ;
#1818 = EDGE_CURVE ( 'NONE', #79871, #5385, #1129, .T. ) ;
#1819 = ORIENTED_EDGE ( 'NONE', *, *, #48420, .T. ) ;
#1820 = ORIENTED_EDGE ( 'NONE', *, *, #75680, .F. ) ;
#1821 = CARTESIAN_POINT ( 'NONE',  ( -112.6235203626142862, -24.66019654487200086, 8.947790411086112172 ) ) ;
#1822 = CARTESIAN_POINT ( 'NONE',  ( -71.62287095715005592, -29.50248528299804818, 1.056150453629036701 ) ) ;
#1823 = CARTESIAN_POINT ( 'NONE',  ( 4.784292611721462585, 5.356774720514426491, -25.54547254883130947 ) ) ;
#1824 = CARTESIAN_POINT ( 'NONE',  ( -41.52287095715006870, -24.51283580621450753, 0.6167428607045382094 ) ) ;
#1825 = ADVANCED_FACE ( 'NONE', ( #84455 ), #91566, .F. ) ;
#1826 = CARTESIAN_POINT ( 'NONE',  ( -63.94589839887400728, -23.78062553189672101, -0.9709657327914295033 ) ) ;
#1827 = AXIS2_PLACEMENT_3D ( 'NONE', #19543, #97175, #40888 ) ;
#1828 = CARTESIAN_POINT ( 'NONE',  ( -1.979602623192304955, -19.45764201480039901, 11.49999999999998934 ) ) ;
#1829 = CARTESIAN_POINT ( 'NONE',  ( -5.053929855541893446, -5.876774720514408301, 19.14848118821636547 ) ) ;
#1830 = ORIENTED_EDGE ( 'NONE', *, *, #16822, .F. ) ;
#1831 = CARTESIAN_POINT ( 'NONE',  ( -5.607854029519995898, -20.77141283803394955, 11.49999999999998934 ) ) ;
#1832 = CARTESIAN_POINT ( 'NONE',  ( -36.52287095715006870, -23.96127896941631263, -0.6493128931038070206 ) ) ;
#1833 = CARTESIAN_POINT ( 'NONE',  ( -6.660000000000001030, 0.000000000000000000, 0.000000000000000000 ) ) ;
#1834 = DIRECTION ( 'NONE',  ( -3.773278334453079618E-23, 0.9999999999976377785, 2.173523156925978705E-06 ) ) ;
#1835 = DIRECTION ( 'NONE',  ( 0.000000000000000000, -0.9999999999976377785, -2.173523156925979128E-06 ) ) ;
#1836 = CARTESIAN_POINT ( 'NONE',  ( 21.44032754495887261, 8.191337786432022483, -1.500000000000002220 ) ) ;
#1837 = B_SPLINE_CURVE_WITH_KNOTS ( 'NONE', 3,
 ( #8469, #93696, #857, #55662, #15571, #30806, #61275, #92196 ),
 .UNSPECIFIED., .F., .F.,
 ( 4, 2, 2, 4 ),
 ( -0.001224873891641422609, -0.0002244903592271080620, 0.0007758931731872060512, 0.002776660238015839048 ),
 .UNSPECIFIED. ) ;
#1838 = PERSON_AND_ORGANIZATION ( #70597, #27821 ) ;
#1839 = CARTESIAN_POINT ( 'NONE',  ( 7.089543269230769162, -6.376774720514413630, 19.75741185897435415 ) ) ;
#1840 = CARTESIAN_POINT ( 'NONE',  ( -42.52287095715005449, -24.51283580621449687, 0.6167428607045715161 ) ) ;
#1841 = CARTESIAN_POINT ( 'NONE',  ( -18.22994410263883225, 8.285605901428201747, 11.49999999999999645 ) ) ;
#1842 = CARTESIAN_POINT ( 'NONE',  ( -78.96619831399281964, -25.31594569180612098, 5.670632933995499059 ) ) ;
#1843 = CARTESIAN_POINT ( 'NONE',  ( -57.62287095715004881, -29.50250786944525672, 11.44777988621623876 ) ) ;
#1844 = DIRECTION ( 'NONE',  ( 0.000000000000000000, 0.9999999999976377785, 2.173523156925979128E-06 ) ) ;
#1845 = DIRECTION ( 'NONE',  ( 0.000000000000000000, 0.000000000000000000, -1.000000000000000000 ) ) ;
#1846 = CARTESIAN_POINT ( 'NONE',  ( -72.62287095715005592, -24.65952944569304606, 1.056160979905698794 ) ) ;
#1847 = CARTESIAN_POINT ( 'NONE',  ( -9.430186865587145917, -19.61854929170128869, -1.500000000000002220 ) ) ;
#1848 = CARTESIAN_POINT ( 'NONE',  ( -4.495793269230770939, -6.376774720514410077, 19.27714342948718595 ) ) ;
#1849 = CARTESIAN_POINT ( 'NONE',  ( -8.122062702759739850, 17.86989387945112995, -1.500000000000002220 ) ) ;
#1850 = FACE_OUTER_BOUND ( 'NONE', #89253, .T. ) ;
#1851 = CARTESIAN_POINT ( 'NONE',  ( -41.62287095715007723, -24.35013146730203815, 9.818937971375117257 ) ) ;
#1852 = CARTESIAN_POINT ( 'NONE',  ( -107.5228709571501042, -23.48783264083360578, -1.443836473376361118 ) ) ;
#1853 = CARTESIAN_POINT ( 'NONE',  ( -67.52287095715006160, -29.50248528299804818, 1.056150453629036701 ) ) ;
#1854 = CARTESIAN_POINT ( 'NONE',  ( 14.24201292913401140, 14.87178044790754328, 11.49999999999999645 ) ) ;
#1855 = DIRECTION ( 'NONE',  ( 0.000000000000000000, 0.000000000000000000, 1.000000000000000000 ) ) ;
#1856 = CARTESIAN_POINT ( 'NONE',  ( -120.5565315140265739, -23.85016227208581441, -0.8807180028928250914 ) ) ;
#1858 = EDGE_CURVE ( 'NONE', #24383, #30940, #20532, .T. ) ;
#1857 = CARTESIAN_POINT ( 'NONE',  ( -19.94007547503736788, -10.58355046294204094, 11.49999999999999645 ) ) ;
#1859 = ORIENTED_EDGE ( 'NONE', *, *, #2198, .T. ) ;
#1860 = CARTESIAN_POINT ( 'NONE',  ( -69.94684934828960365, -25.12219130708524517, 7.037048346111795638 ) ) ;
#1862 = EDGE_CURVE ( 'NONE', #51996, #1269, #53030, .T. ) ;
#1861 = DIRECTION ( 'NONE',  ( 1.000000000000000000, 0.000000000000000000, 0.000000000000000000 ) ) ;
#1863 = CARTESIAN_POINT ( 'NONE',  ( 0.1645010273463760886, 1.417169167140627906, 0.3687607960183699740 ) ) ;
#1864 = CARTESIAN_POINT ( 'NONE',  ( -27.33104310173779083, -24.76554706090742997, 2.324039223911030572 ) ) ;
#1865 = CARTESIAN_POINT ( 'NONE',  ( -33.62287095715005592, -24.64898659630367206, 1.056161002820817485 ) ) ;
#1866 = DIRECTION ( 'NONE',  ( -0.4009304992412300317, 0.000000000000000000, -0.9161084732596779245 ) ) ;
#1867 = ORIENTED_EDGE ( 'NONE', *, *, #39150, .F. ) ;
#1868 = CARTESIAN_POINT ( 'NONE',  ( 8.651921485055520833, -21.43433228965458781, 11.49999999999999645 ) ) ;
#1869 = CARTESIAN_POINT ( 'NONE',  ( -16.39533425382319720, 15.89506036719111037, 11.49999999999998934 ) ) ;
#1870 = CARTESIAN_POINT ( 'NONE',  ( 22.02124265030973760, 3.456774720514426136, 16.20402280011862217 ) ) ;
#1871 = PLANE ( 'NONE',  #62529 ) ;
#1872 = CARTESIAN_POINT ( 'NONE',  ( -63.51555983570501951, -23.73791477778911840, 11.05961554403170766 ) ) ;
#1873 = CARTESIAN_POINT ( 'NONE',  ( 8.413247042826936806, 20.86129769029627923, 11.49999999999999645 ) ) ;
#1874 = ORIENTED_EDGE ( 'NONE', *, *, #12483, .F. ) ;
#1875 = DIRECTION ( 'NONE',  ( 1.000000000000000000, 0.000000000000000000, 0.000000000000000000 ) ) ;
#1876 = VECTOR ( 'NONE', #78946, 1000.000000000000227 ) ;
#1877 = CARTESIAN_POINT ( 'NONE',  ( -6.887433846447126307, -20.85920400149894149, 11.49999999999998934 ) ) ;
#1878 = CARTESIAN_POINT ( 'NONE',  ( -124.5120803120196058, -25.40057329153380650, 4.607783471004946563 ) ) ;
#1879 = EDGE_CURVE ( 'NONE', #45924, #50012, #83431, .T. ) ;
#1880 = DIRECTION ( 'NONE',  ( -3.773278334453079618E-23, 0.9999999999976377785, 2.173523156925979975E-06 ) ) ;
#1881 = DIRECTION ( 'NONE',  ( -0.000000000000000000, -1.000000000000000000, -0.000000000000000000 ) ) ;
#1882 = ORIENTED_EDGE ( 'NONE', *, *, #49450, .F. ) ;
#1883 = DIRECTION ( 'NONE',  ( 0.000000000000000000, 0.000000000000000000, -1.000000000000000000 ) ) ;
#1884 = FACE_OUTER_BOUND ( 'NONE', #6110, .T. ) ;
#1885 = ORIENTED_EDGE ( 'NONE', *, *, #82355, .T. ) ;
#1886 = B_SPLINE_CURVE_WITH_KNOTS ( 'NONE', 3,
 ( #69587, #16788, #46242, #9683, #85807, #7678, #40642, #55876, #93910, #31512, #24401, #63494, #62475, #47754, #16287, #78174, #79187, #78668 ),
 .UNSPECIFIED., .F., .F.,
 ( 4, 2, 2, 2, 2, 2, 2, 2, 4 ),
 ( 1.411962612463446054E-17, 0.0002845812759709316587, 0.0005691625519418492228, 0.0008537438279127667869, 0.001138325103883684351, 0.001422906379854601807, 0.001707487655825519479, 0.001992068931796437369, 0.002276650207767354824 ),
 .UNSPECIFIED. ) ;
#1887 = CARTESIAN_POINT ( 'NONE',  ( -19.82921842031888104, 5.099586017421429140, -1.500000000000002220 ) ) ;
#1888 = VERTEX_POINT ( 'NONE', #28682 ) ;
#1889 = EDGE_CURVE ( 'NONE', #42461, #81255, #61718, .T. ) ;
#1890 = ORIENTED_EDGE ( 'NONE', *, *, #23545, .T. ) ;
#1891 = VERTEX_POINT ( 'NONE', #45910 ) ;
#1892 = ORIENTED_EDGE ( 'NONE', *, *, #6915, .T. ) ;
#1893 = CARTESIAN_POINT ( 'NONE',  ( 17.26854690438276307, -15.35948741044508559, 11.49999999999998934 ) ) ;
#1894 = LINE ( 'NONE', #93724, #94085 ) ;
#1895 = CARTESIAN_POINT ( 'NONE',  ( 19.83649001621966335, 4.521578618930774951, -1.500000000000002220 ) ) ;
#1896 = VERTEX_POINT ( 'NONE', #43911 ) ;
#1897 = ADVANCED_FACE ( 'NONE', ( #59646 ), #90575, .F. ) ;
#1898 = DIRECTION ( 'NONE',  ( -3.773278334444167608E-23, 1.000000000000000000, 0.000000000000000000 ) ) ;
#1899 = ADVANCED_FACE ( 'NONE', ( #77330 ), #8836, .T. ) ;
#1900 = LINE ( 'NONE', #17617, #87082 ) ;
#1901 = EDGE_CURVE ( 'NONE', #75398, #88641, #47404, .T. ) ;
#1903 = CARTESIAN_POINT ( 'NONE',  ( -39.92287095715006018, -23.47596703998600276, 11.44779298504227683 ) ) ;
#1902 = CIRCLE ( 'NONE', #11584, 2.249999999999998668 ) ;
#1904 = CARTESIAN_POINT ( 'NONE',  ( 4.653515142448186204, -6.376774720514413630, 19.86181745814487343 ) ) ;
#1906 = ORIENTED_EDGE ( 'NONE', *, *, #81067, .F. ) ;
#1905 = CARTESIAN_POINT ( 'NONE',  ( 3.930203739357332360, 21.12693704021120666, 11.49999999999999645 ) ) ;
#1907 = CARTESIAN_POINT ( 'NONE',  ( -75.52207693552151113, -23.48783264082477018, -1.443836473390089914 ) ) ;
#1908 = CARTESIAN_POINT ( 'NONE',  ( -48.52287095715006160, -24.64898659630367561, 1.056161002820821038 ) ) ;
#1910 = ADVANCED_FACE ( 'NONE', ( #40786 ), #24000, .F. ) ;
#1909 = CC_DESIGN_APPROVAL ( #48847, ( #60221 ) ) ;
#1911 = ORIENTED_EDGE ( 'NONE', *, *, #36387, .F. ) ;
#1912 = CARTESIAN_POINT ( 'NONE',  ( 8.056674255711671506, 19.11000797562349618, -1.500000000000002220 ) ) ;
#1913 = VERTEX_POINT ( 'NONE', #70740 ) ;
#1915 = VERTEX_POINT ( 'NONE', #23537 ) ;
#1914 = CARTESIAN_POINT ( 'NONE',  ( -57.52287095715005449, -23.48786465467241058, 11.44779295918254824 ) ) ;
#1916 = CARTESIAN_POINT ( 'NONE',  ( -23.59123376470063960, -6.143225279485574397, 24.50402280011862288 ) ) ;
#1917 = CARTESIAN_POINT ( 'NONE',  ( 16.36243866176394945, 0.000000000000000000, 2.399999999999999911 ) ) ;
#1918 = EDGE_LOOP ( 'NONE', ( #48605, #100308, #46695, #93169 ) ) ;
#1919 = ORIENTED_EDGE ( 'NONE', *, *, #78108, .F. ) ;
#1920 = CARTESIAN_POINT ( 'NONE',  ( -5.923037968371668072, -5.876774720514414518, 19.62288733224861303 ) ) ;
#1921 = CARTESIAN_POINT ( 'NONE',  ( -42.60032671284469785, -23.96169478059713143, 10.65365249895718947 ) ) ;
#1923 = EDGE_CURVE ( 'NONE', #53590, #63195, #70237, .T. ) ;
#1922 = CARTESIAN_POINT ( 'NONE',  ( -29.58730922106722261, -25.09253774316045238, 3.113369324251616277 ) ) ;
#1924 = EDGE_CURVE ( 'NONE', #24545, #91623, #5979, .T. ) ;
#1926 = ORIENTED_EDGE ( 'NONE', *, *, #65751, .F. ) ;
#1925 = CARTESIAN_POINT ( 'NONE',  ( 20.91424602935089894, 6.983905699820807556, 11.49999999999999645 ) ) ;
#1927 = CARTESIAN_POINT ( 'NONE',  ( -8.499999999999987566, 18.74999999999999645, 2.100000000000000089 ) ) ;
#1928 = CARTESIAN_POINT ( 'NONE',  ( -21.70561270324154179, 6.225854807558039994, 11.49999999999998934 ) ) ;
#1929 = CARTESIAN_POINT ( 'NONE',  ( 19.54352652498339182, 7.673529024697476331, 11.49999999999998934 ) ) ;
#1931 = ORIENTED_EDGE ( 'NONE', *, *, #33555, .F. ) ;
#1930 = CARTESIAN_POINT ( 'NONE',  ( 0.4923289614720766649, -7.060444313164428998, -9.000000000000000000 ) ) ;
#1932 = ORIENTED_EDGE ( 'NONE', *, *, #1575, .F. ) ;
#1933 = LINE ( 'NONE', #72445, #9402 ) ;
#1934 = ADVANCED_FACE ( 'NONE', ( #9327 ), #55020, .F. ) ;
#1935 = AXIS2_PLACEMENT_3D ( 'NONE', #45851, #76770, #7779 ) ;
#1936 = EDGE_CURVE ( 'NONE', #35496, #42575, #20808, .T. ) ;
#1937 = DIRECTION ( 'NONE',  ( -1.000000000000000000, -0.000000000000000000, -0.000000000000000000 ) ) ;
#1938 = ORIENTED_EDGE ( 'NONE', *, *, #59876, .F. ) ;
#1939 = CARTESIAN_POINT ( 'NONE',  ( 1.363997202867437863, 21.09336101032836908, 11.49999999999998934 ) ) ;
#1940 = CARTESIAN_POINT ( 'NONE',  ( -117.5562042904833930, -23.47593901973091235, -1.443836447538997536 ) ) ;
#1941 = CARTESIAN_POINT ( 'NONE',  ( -60.72703938549737046, -25.27183489919806192, 3.712349809207165841 ) ) ;
#1942 = CARTESIAN_POINT ( 'NONE',  ( -75.62287095715012697, -24.51163499207175533, 0.6490370598554298098 ) ) ;
#1943 = CARTESIAN_POINT ( 'NONE',  ( -7.312991930324885814, -5.876774720514413630, 20.02088365235844947 ) ) ;
#1944 = DIRECTION ( 'NONE',  ( -0.000000000000000000, 1.000000000000000000, -0.000000000000000000 ) ) ;
#1945 = CARTESIAN_POINT ( 'NONE',  ( 21.95989154999629278, -3.605859658025859282, -1.500000000000002220 ) ) ;
#1946 = CARTESIAN_POINT ( 'NONE',  ( -114.5206660350143721, -23.73766607897672287, -1.055555164236428700 ) ) ;
#1947 = ADVANCED_FACE ( 'NONE', ( #24049 ), #78826, .T. ) ;
#1948 = ORIENTED_EDGE ( 'NONE', *, *, #29490, .T. ) ;
#1949 = CARTESIAN_POINT ( 'NONE',  ( -5.533628790199073499, -6.376774720514417183, 19.87297243748313491 ) ) ;
#1950 = CARTESIAN_POINT ( 'NONE',  ( -58.58953762381673869, -23.47596703998600276, 11.44779298504227505 ) ) ;
#1951 = CARTESIAN_POINT ( 'NONE',  ( -9.383883476483159569, 17.86611652351680846, 2.100000000000000089 ) ) ;
#1952 = EDGE_CURVE ( 'NONE', #32503, #21619, #46399, .T. ) ;
#1953 = LINE ( 'NONE', #92528, #99744 ) ;
#1954 = CARTESIAN_POINT ( 'NONE',  ( -33.62287095715005592, -24.50321055353805377, 9.387540953477536476 ) ) ;
#1955 = EDGE_CURVE ( 'NONE', #57577, #79844, #92562, .T. ) ;
#1956 = CARTESIAN_POINT ( 'NONE',  ( -7.007757480239389380, 18.17491015770016816, -1.500000000000002220 ) ) ;
#1957 = CARTESIAN_POINT ( 'NONE',  ( -5.333777546869826303, -20.73983961313815172, -1.500000000000002220 ) ) ;
#1958 = FACE_OUTER_BOUND ( 'NONE', #29896, .T. ) ;
#1959 = CARTESIAN_POINT ( 'NONE',  ( -60.48802560456093147, -24.73531770709804078, 8.716586749031112191 ) ) ;
#1960 = VECTOR ( 'NONE', #62384, 1000.000000000000114 ) ;
#1961 = CARTESIAN_POINT ( 'NONE',  ( -51.56792531176364491, -23.48783264082476308, -1.443836473390094133 ) ) ;
#1962 = CARTESIAN_POINT ( 'NONE',  ( -52.52287095715008292, -24.66019654487198665, 8.947790411086131712 ) ) ;
#1963 = CARTESIAN_POINT ( 'NONE',  ( 15.01325480956343483, 17.08929600257393489, -1.500000000000002220 ) ) ;
#1964 = EDGE_CURVE ( 'NONE', #96941, #43106, #43511, .T. ) ;
#1965 = FACE_OUTER_BOUND ( 'NONE', #63215, .T. ) ;
#1966 = CARTESIAN_POINT ( 'NONE',  ( 27.53860345374808105, -4.772774720514425972, -8.321925749325261634 ) ) ;
#1967 = CARTESIAN_POINT ( 'NONE',  ( 7.713363164125232707, -18.29545692620113684, 11.49999999999999645 ) ) ;
#1968 = CARTESIAN_POINT ( 'NONE',  ( -123.5190355150976416, -24.66019654487200441, 8.947790411086106843 ) ) ;
#1969 = CARTESIAN_POINT ( 'NONE',  ( -108.5562042904834072, -23.48786465467241769, 11.44779295918254292 ) ) ;
#1970 = CARTESIAN_POINT ( 'NONE',  ( -64.92287095715006728, -23.47593901973090169, -1.443836447538997536 ) ) ;
#1971 = ORIENTED_EDGE ( 'NONE', *, *, #86242, .F. ) ;
#1972 = FACE_OUTER_BOUND ( 'NONE', #25331, .T. ) ;
#1973 = CARTESIAN_POINT ( 'NONE',  ( -80.52287095715009002, -24.62285846331441874, 9.038163153548151030 ) ) ;
#1974 = CARTESIAN_POINT ( 'NONE',  ( -51.52876458270549165, -25.27412355576682046, 3.420678484884101422 ) ) ;
#1975 = CARTESIAN_POINT ( 'NONE',  ( -2.129050106866105185, 21.58297100922832357, -1.500000000000002220 ) ) ;
#1976 = CARTESIAN_POINT ( 'NONE',  ( -56.63815877224512718, -24.15620529776628445, 10.23563542870660648 ) ) ;
#1977 = CARTESIAN_POINT ( 'NONE',  ( 1.255614643274026276, -19.41590359075080841, -1.500000000000002220 ) ) ;
#1978 = DIRECTION ( 'NONE',  ( 0.000000000000000000, 0.9999999999976377785, 2.173523156925979128E-06 ) ) ;
#1979 = TOROIDAL_SURFACE ( 'NONE', #39249, 25.90800000000000125, 3.060000000000000053 ) ;
#1980 = EDGE_LOOP ( 'NONE', ( #35560, #60896, #54666, #76639 ) ) ;
#1981 = CC_DESIGN_APPROVAL ( #28322, ( #34420 ) ) ;
#1982 = CARTESIAN_POINT ( 'NONE',  ( 9.511415417357532931, -18.05363124325620205, 11.49999999999999645 ) ) ;
#1983 = DIRECTION ( 'NONE',  ( -3.773278334444167608E-23, 1.000000000000000000, 0.000000000000000000 ) ) ;
#1984 = DIRECTION ( 'NONE',  ( 0.000000000000000000, 1.000000000000000000, -6.307606751056558338E-17 ) ) ;
#1985 = ORIENTED_EDGE ( 'NONE', *, *, #91939, .F. ) ;
#1986 = CARTESIAN_POINT ( 'NONE',  ( -79.70293883480100305, -25.07319016999186090, 7.368904005479246955 ) ) ;
#1987 = CARTESIAN_POINT ( 'NONE',  ( 33.60604063885286052, 3.409250796720436405, -11.91850954671862617 ) ) ;
#1988 = CARTESIAN_POINT ( 'NONE',  ( 30.56715118582953750, -3.660718435927268199, 25.08875473125879196 ) ) ;
#1989 = CARTESIAN_POINT ( 'NONE',  ( -49.35642674012009223, -25.25138802042284780, 5.792946750273627821 ) ) ;
#1990 = DIRECTION ( 'NONE',  ( -0.000000000000000000, 1.000000000000000000, -0.000000000000000000 ) ) ;
#1991 = CARTESIAN_POINT ( 'NONE',  ( -109.6330755333671334, -23.48783264082476663, -1.443836473390089470 ) ) ;
#1992 = ORIENTED_EDGE ( 'NONE', *, *, #54926, .F. ) ;
#1993 = CARTESIAN_POINT ( 'NONE',  ( -66.54416241931652110, -24.35071581493543036, 9.817618358456028815 ) ) ;
#1994 = CARTESIAN_POINT ( 'NONE',  ( -22.40196285382242536, -4.882868457752029379, 11.49999999999999645 ) ) ;
#1995 = CARTESIAN_POINT ( 'NONE',  ( 2.440706796964721370, 22.61111150098722788, 11.49999999999998934 ) ) ;
#1996 = ORIENTED_EDGE ( 'NONE', *, *, #78456, .T. ) ;
#1997 = CARTESIAN_POINT ( 'NONE',  ( -81.42380231474228935, -25.31401921878147832, 5.197788989978542773 ) ) ;
#1998 = CARTESIAN_POINT ( 'NONE',  ( -98.52287095715000476, -23.96127896941632329, -0.6493128931038036900 ) ) ;
#1999 = CARTESIAN_POINT ( 'NONE',  ( -123.6228709571500559, -24.66019654487200086, 8.947790411086117501 ) ) ;
#2000 = FACE_OUTER_BOUND ( 'NONE', #25505, .T. ) ;
#2001 = B_SPLINE_CURVE_WITH_KNOTS ( 'NONE', 3,
 ( #20370, #51344, #57973, #34125, #88912, #50350 ),
 .UNSPECIFIED., .F., .F.,
 ( 4, 2, 4 ),
 ( 6.391158118959990520E-06, 0.001387004593080774003, 0.002767618028042588118 ),
 .UNSPECIFIED. ) ;
#2002 = CARTESIAN_POINT ( 'NONE',  ( -69.55927315202205818, -23.73791477778911485, 11.05961554403170766 ) ) ;
#2003 = VECTOR ( 'NONE', #55101, 1000.000000000000000 ) ;
#2004 = ADVANCED_FACE ( 'NONE', ( #2239 ), #61642, .T. ) ;
#2005 = DIRECTION ( 'NONE',  ( 0.000000000000000000, 0.9513357669802769978, -0.3081562241202474572 ) ) ;
#2006 = FACE_OUTER_BOUND ( 'NONE', #59724, .T. ) ;
#2007 = CARTESIAN_POINT ( 'NONE',  ( -58.59839962558949367, -23.96119346886880308, -0.6495511937832116889 ) ) ;
#2008 = ORIENTED_EDGE ( 'NONE', *, *, #79429, .T. ) ;
#2009 = EDGE_CURVE ( 'NONE', #47693, #93719, #1729, .T. ) ;
#2010 = CARTESIAN_POINT ( 'NONE',  ( 7.100489274569507181, 19.11111018586187527, -1.500000000000002220 ) ) ;
#2012 = ADVANCED_FACE ( 'NONE', ( #69741 ), #30347, .T. ) ;
#2011 = ORIENTED_EDGE ( 'NONE', *, *, #39501, .T. ) ;
#2013 = ORIENTED_EDGE ( 'NONE', *, *, #40219, .T. ) ;
#2014 = B_SPLINE_CURVE_WITH_KNOTS ( 'NONE', 3,
 ( #18320, #31531, #70602, #1094, #50778, #81719, #42675, #96441, #57406, #12191, #65027, #3114, #81219, #35050, #27438, #74595 ),
 .UNSPECIFIED., .F., .F.,
 ( 4, 2, 2, 2, 2, 2, 2, 4 ),
 ( 1.939467588463157335E-15, 0.0001875988099759247666, 0.0003751976199499100582, 0.0007503952398979218952, 0.001125592859845933732, 0.001313191669819952770, 0.001406991074806955566, 0.001500790479793958363 ),
 .UNSPECIFIED. ) ;
#2015 = CARTESIAN_POINT ( 'NONE',  ( 17.37538969058663696, -15.08583811485692117, -1.500000000000002220 ) ) ;
#2016 = CARTESIAN_POINT ( 'NONE',  ( -117.5228709571500758, -29.50250243563736774, 8.947779886222134493 ) ) ;
#2017 = ADVANCED_FACE ( 'NONE', ( #10842 ), #88969, .T. ) ;
#2018 = ORIENTED_EDGE ( 'NONE', *, *, #67379, .F. ) ;
#2019 = CARTESIAN_POINT ( 'NONE',  ( 13.10664265030973930, 5.965225279485574461, -28.18129937516157568 ) ) ;
#2020 = EDGE_CURVE ( 'NONE', #58811, #25123, #52001, .T. ) ;
#2021 = CYLINDRICAL_SURFACE ( 'NONE', #83816, 3.349999999999998757 ) ;
#2022 = EDGE_CURVE ( 'NONE', #46703, #34658, #11339, .T. ) ;
#2023 = CARTESIAN_POINT ( 'NONE',  ( -95.63508492949864603, -24.15503026093913874, -0.2815557561904519224 ) ) ;
#2024 = CARTESIAN_POINT ( 'NONE',  ( -116.7734655731286182, -25.27149756095137434, 5.922859442452534928 ) ) ;
#2026 = ORIENTED_EDGE ( 'NONE', *, *, #14356, .T. ) ;
#2025 = CARTESIAN_POINT ( 'NONE',  ( 17.78463046036513617, -11.72987588014745342, 11.49999999999999645 ) ) ;
#2027 = VECTOR ( 'NONE', #28920, 1000.000000000000114 ) ;
#2028 = EDGE_CURVE ( 'NONE', #40347, #89809, #11829, .T. ) ;
#2029 = ORIENTED_EDGE ( 'NONE', *, *, #23760, .F. ) ;
#2030 = CARTESIAN_POINT ( 'NONE',  ( -15.91109736606077441, 15.52988587838853540, -1.500000000000002220 ) ) ;
#2031 = VECTOR ( 'NONE', #33172, 1000.000000000000114 ) ;
#2032 = CARTESIAN_POINT ( 'NONE',  ( 10.45329875151443488, -17.81600612866554556, -1.500000000000002220 ) ) ;
#2033 = EDGE_LOOP ( 'NONE', ( #7120, #78790, #20221, #31481 ) ) ;
#2034 = CARTESIAN_POINT ( 'NONE',  ( 0.1309051665272248643, -6.376774720514413630, 19.34190049657482291 ) ) ;
#2035 = CARTESIAN_POINT ( 'NONE',  ( -95.50800993025161745, -24.52399227489127398, 9.353111116836524630 ) ) ;
#2036 = ORIENTED_EDGE ( 'NONE', *, *, #31919, .T. ) ;
#2037 = CARTESIAN_POINT ( 'NONE',  ( 7.150000000000004796, -2.000000000000001776, 24.00000000000000000 ) ) ;
#2038 = ORIENTED_EDGE ( 'NONE', *, *, #68252, .T. ) ;
#2039 = CARTESIAN_POINT ( 'NONE',  ( -58.57884717839115751, -24.66019654487199730, 8.947790411086117501 ) ) ;
#2040 = CARTESIAN_POINT ( 'NONE',  ( 13.10664265030973930, 0.3587747205144256601, -28.18129937523770678 ) ) ;
#2041 = CARTESIAN_POINT ( 'NONE',  ( 7.204507412156021751, -19.57454612608841771, -1.500000000000002220 ) ) ;
#2042 = ADVANCED_FACE ( 'NONE', ( #34182 ), #49922, .T. ) ;
#2043 = CARTESIAN_POINT ( 'NONE',  ( -21.44618410820073606, 4.064364382921047181, 11.49999999999999645 ) ) ;
#2044 = CARTESIAN_POINT ( 'NONE',  ( -73.49932069601484841, -24.51419770103157347, 9.386484678747175181 ) ) ;
#2045 = DIRECTION ( 'NONE',  ( -0.000000000000000000, 0.000000000000000000, -1.000000000000000000 ) ) ;
#2046 = CARTESIAN_POINT ( 'NONE',  ( 22.08653571170524543, -4.319401766784854324, -1.500000000000002220 ) ) ;
#2047 = CARTESIAN_POINT ( 'NONE',  ( -50.41800648699645393, -25.31296764934565857, 4.735575929649717963 ) ) ;
#2048 = FACE_OUTER_BOUND ( 'NONE', #90624, .T. ) ;
#2049 = VECTOR ( 'NONE', #70329, 1000.000000000000114 ) ;
#2050 = CARTESIAN_POINT ( 'NONE',  ( -54.58953762381672448, -24.65952944569304606, 1.056160979905695463 ) ) ;
#2052 = ORIENTED_EDGE ( 'NONE', *, *, #7371, .T. ) ;
#2051 = EDGE_CURVE ( 'NONE', #38938, #45450, #65158, .T. ) ;
#2053 = CC_DESIGN_APPROVAL ( #59956, ( #92779 ) ) ;
#2054 = ORIENTED_EDGE ( 'NONE', *, *, #72940, .T. ) ;
#2055 = ORIENTED_EDGE ( 'NONE', *, *, #92519, .T. ) ;
#2056 = CARTESIAN_POINT ( 'NONE',  ( -99.31542661674430406, -25.26221151531081333, 6.334584452247769448 ) ) ;
#2057 = ORIENTED_EDGE ( 'NONE', *, *, #13555, .T. ) ;
#2058 = CARTESIAN_POINT ( 'NONE',  ( -9.924231251898440576, -18.97836718215353713, -1.500000000000002220 ) ) ;
#2059 = AXIS2_PLACEMENT_3D ( 'NONE', #61741, #84552, #69841 ) ;
#2060 = CARTESIAN_POINT ( 'NONE',  ( -21.16225983376422448, 7.283793490815352989, 11.49999999999999645 ) ) ;
#2061 = ORIENTED_EDGE ( 'NONE', *, *, #19177, .F. ) ;
#2062 = CARTESIAN_POINT ( 'NONE',  ( 32.74409430444596580, -4.661791533294295853, -3.688467650546950249 ) ) ;
#2063 = CARTESIAN_POINT ( 'NONE',  ( -13.06023916655064276, -16.53025015627232719, 11.49999999999998934 ) ) ;
#2064 = CARTESIAN_POINT ( 'NONE',  ( -30.46620467572866886, -25.14197234194089603, 7.291421475381016926 ) ) ;
#2065 = CARTESIAN_POINT ( 'NONE',  ( -14.97016004668225264, 13.15154794113874637, -1.500000000000002220 ) ) ;
#2066 = CARTESIAN_POINT ( 'NONE',  ( -50.58239890853555210, -24.73531770709094602, 8.716586749053508498 ) ) ;
#2067 = CARTESIAN_POINT ( 'NONE',  ( -80.74930246458728789, -25.30877083504385183, 4.554285748811262025 ) ) ;
#2068 = CARTESIAN_POINT ( 'NONE',  ( 22.04941498731238525, 0.3350016526185666255, -1.500000000000002220 ) ) ;
#2069 = AXIS2_PLACEMENT_3D ( 'NONE', #60460, #20864, #13748 ) ;
#2070 = ORIENTED_EDGE ( 'NONE', *, *, #93615, .T. ) ;
#2071 = CARTESIAN_POINT ( 'NONE',  ( -111.5228709571500616, -29.50248528299804818, 1.056150453629043584 ) ) ;
#2072 = LINE ( 'NONE', #73081, #78951 ) ;
#2073 = CARTESIAN_POINT ( 'NONE',  ( -20.60679684081203789, -3.318877370925724879, 11.49999999999999645 ) ) ;
#2074 = EDGE_CURVE ( 'NONE', #46475, #7077, #22846, .T. ) ;
#2075 = CARTESIAN_POINT ( 'NONE',  ( 29.62673903083957683, -5.344535611318891988, 28.45872576146958011 ) ) ;
#2076 = LINE ( 'NONE', #92893, #55418 ) ;
#2077 = CARTESIAN_POINT ( 'NONE',  ( -63.52287095715003318, -23.48783264082477018, -1.443836473390091690 ) ) ;
#2078 = CARTESIAN_POINT ( 'NONE',  ( -16.05942832139214360, -14.02155611864158402, 11.49999999999998934 ) ) ;
#2079 = CARTESIAN_POINT ( 'NONE',  ( -121.6228709571500417, -24.64965695001469115, 8.947790433994175174 ) ) ;
#2080 = CARTESIAN_POINT ( 'NONE',  ( -124.5228709571500616, -24.64898659630368627, 1.056161002820833028 ) ) ;
#2081 = EDGE_CURVE ( 'NONE', #7066, #1588, #98605, .T. ) ;
#2082 = CARTESIAN_POINT ( 'NONE',  ( -71.52287095715007581, -24.65952944569304606, 1.056160979905697239 ) ) ;
#2083 = CARTESIAN_POINT ( 'NONE',  ( 10.75273025779354263, -5.876774720514426953, 16.96478738960562893 ) ) ;
#2084 = CARTESIAN_POINT ( 'NONE',  ( 22.24477432615492134, 4.004077059304647968, -1.500000000000002220 ) ) ;
#2085 = AXIS2_PLACEMENT_3D ( 'NONE', #21015, #98633, #60607 ) ;
#2086 = B_SPLINE_SURFACE_WITH_KNOTS ( 'NONE', 3, 3, ( 
 ( #86519, #88033, #79906, #48478 ),
 ( #78895, #72308, #17005, #64723 ),
 ( #64213, #18507, #47970, #9393 ),
 ( #86021, #10396, #56088, #39347 ),
 ( #70306, #40354, #1297, #17511 ),
 ( #95640, #71308, #71812, #79404 ),
 ( #31738, #62706, #93621, #1795 ) ),
 .UNSPECIFIED., .F., .F., .F.,
 ( 4, 3, 4 ),
 ( 4, 4 ),
 ( 0.0004766839783814567867, 0.1029713700210892341, 0.2054660560637970035 ),
 ( 0.7096745263232591139, 0.7110146934017589349 ),
 .UNSPECIFIED. ) ;
#2087 = CARTESIAN_POINT ( 'NONE',  ( -83.52287095715001897, -24.66019654487199375, 8.947790411086122830 ) ) ;
#2088 = ORIENTED_EDGE ( 'NONE', *, *, #16133, .F. ) ;
#2089 = CARTESIAN_POINT ( 'NONE',  ( 30.93860345374796594, 0.000000000000000000, 0.000000000000000000 ) ) ;
#2090 = CARTESIAN_POINT ( 'NONE',  ( -122.6228709571500417, -23.72747288104442021, -1.053458166803660667 ) ) ;
#2091 = CARTESIAN_POINT ( 'NONE',  ( -3.719764837209879271, -19.30396570740023421, 11.49999999999999645 ) ) ;
#2092 = DIRECTION ( 'NONE',  ( 1.000000000000000000, 0.000000000000000000, -0.000000000000000000 ) ) ;
#2093 = B_SPLINE_CURVE_WITH_KNOTS ( 'NONE', 3,
 ( #83373, #29589, #14357, #29091 ),
 .UNSPECIFIED., .F., .F.,
 ( 4, 4 ),
 ( 0.000000000000000000, 9.999999999998897304E-05 ),
 .UNSPECIFIED. ) ;
#2094 = B_SPLINE_CURVE_WITH_KNOTS ( 'NONE', 3,
 ( #35128, #89408, #80801, #73193 ),
 .UNSPECIFIED., .F., .F.,
 ( 4, 4 ),
 ( 2.775557561562891351E-17, 0.0001000000000000167286 ),
 .UNSPECIFIED. ) ;
#2095 = DIRECTION ( 'NONE',  ( -1.000000000000000000, 0.000000000000000000, -1.334402673828313586E-16 ) ) ;
#2096 = ORIENTED_EDGE ( 'NONE', *, *, #31922, .F. ) ;
#2097 = CARTESIAN_POINT ( 'NONE',  ( -99.55261637441094535, -24.15543982623907837, -0.2315651400026449425 ) ) ;
#2098 = LINE ( 'NONE', #48263, #99884 ) ;
#2099 = AXIS2_PLACEMENT_3D ( 'NONE', #91241, #21714, #52688 ) ;
#2100 = DIRECTION ( 'NONE',  ( 0.9872275723272648795, 0.000000000000000000, 0.1593164160933056017 ) ) ;
#2101 = LINE ( 'NONE', #31144, #77086 ) ;
#2102 = PLANE ( 'NONE',  #22159 ) ;
#2103 = CARTESIAN_POINT ( 'NONE',  ( 17.76913753361954562, 8.601950719843506121, 11.49999999999998934 ) ) ;
#2104 = ORIENTED_EDGE ( 'NONE', *, *, #39676, .F. ) ;
#2105 = AXIS2_PLACEMENT_3D ( 'NONE', #47774, #55896, #84814 ) ;
#2106 = CARTESIAN_POINT ( 'NONE',  ( -17.27845874757997535, -10.49745931960568335, 11.49999999999999645 ) ) ;
#2107 = CARTESIAN_POINT ( 'NONE',  ( 5.697397333356354565, -5.876774720514418959, 20.51730809691671809 ) ) ;
#2108 = EDGE_LOOP ( 'NONE', ( #76754, #92993, #30196, #47183, #19230 ) ) ;
#2109 = DIRECTION ( 'NONE',  ( 0.000000000000000000, 0.9999999999976377785, 2.173523156925979128E-06 ) ) ;
#2110 = CARTESIAN_POINT ( 'NONE',  ( -80.43221577628075636, -25.30553498687082481, 4.967019777649441359 ) ) ;
#2111 = CARTESIAN_POINT ( 'NONE',  ( -100.2380303841250395, -25.03145177541831856, 7.557071270405856467 ) ) ;
#2112 = CARTESIAN_POINT ( 'NONE',  ( -82.62287095715002749, -24.33832256527049154, 0.1851278514138593179 ) ) ;
#2113 = LINE ( 'NONE', #33048, #79722 ) ;
#2114 = CARTESIAN_POINT ( 'NONE',  ( -120.6228709571500559, -23.48786465467241769, 11.44779295918253759 ) ) ;
#2115 = CARTESIAN_POINT ( 'NONE',  ( 16.76344175524385705, -10.90933549886441156, -1.500000000000002220 ) ) ;
#2116 = CARTESIAN_POINT ( 'NONE',  ( -99.21726371882367346, -25.10935196860294383, 3.564825239790214706 ) ) ;
#2117 = FACE_OUTER_BOUND ( 'NONE', #39200, .T. ) ;
#2118 = ORIENTED_EDGE ( 'NONE', *, *, #28634, .T. ) ;
#2119 = AXIS2_PLACEMENT_3D ( 'NONE', #53883, #84815, #46262 ) ;
#2121 = CARTESIAN_POINT ( 'NONE',  ( 11.22434917415779054, -4.132774715458839232, -26.87660878605755599 ) ) ;
#2120 = SECURITY_CLASSIFICATION ( '', '', #14562 ) ;
#2122 = CARTESIAN_POINT ( 'NONE',  ( -78.62287095715007013, -24.66019654487199375, 8.947790411086124607 ) ) ;
#2123 = CARTESIAN_POINT ( 'NONE',  ( -92.62287095715005592, -23.47596703998600631, 11.44779298504227860 ) ) ;
#2124 = B_SPLINE_CURVE_WITH_KNOTS ( 'NONE', 3,
 ( #69059, #546, #93896, #53350 ),
 .UNSPECIFIED., .F., .F.,
 ( 4, 4 ),
 ( 0.000000000000000000, 1.000000000000000000 ),
 .UNSPECIFIED. ) ;
#2125 = CARTESIAN_POINT ( 'NONE',  ( -116.5120803120195916, -25.40057329153378518, 4.607783471004933240 ) ) ;
#2126 = CARTESIAN_POINT ( 'NONE',  ( -51.69903695958453227, -25.26279909962675774, 4.034228678170331150 ) ) ;
#2127 = CARTESIAN_POINT ( 'NONE',  ( -63.62287095715007723, -24.35013146730203459, 9.818937971375108376 ) ) ;
#2128 = CIRCLE ( 'NONE', #34497, 1.249999999999997558 ) ;
#2129 = ADVANCED_FACE ( 'NONE', ( #41290 ), #84634, .T. ) ;
#2130 = DIRECTION ( 'NONE',  ( 0.000000000000000000, 0.3081562241202472907, 0.9513357669802769978 ) ) ;
#2131 = VERTEX_POINT ( 'NONE', #99540 ) ;
#2132 = EDGE_CURVE ( 'NONE', #23327, #77908, #32568, .T. ) ;
#2133 = CARTESIAN_POINT ( 'NONE',  ( 18.82434097252966154, -7.598309640217090433, 11.49999999999998934 ) ) ;
#2134 = AXIS2_PLACEMENT_3D ( 'NONE', #26644, #27643, #20016 ) ;
#2135 = CARTESIAN_POINT ( 'NONE',  ( 31.63443928675788186, 3.712996582965905290, 27.28441363938236464 ) ) ;
#2136 = ADVANCED_FACE ( 'NONE', ( #68618 ), #35678, .T. ) ;
#2137 = CARTESIAN_POINT ( 'NONE',  ( -114.6228709571500417, -23.94994826722566117, -0.6494450866342732498 ) ) ;
#2138 = CARTESIAN_POINT ( 'NONE',  ( -59.58753039450819955, -24.35071581493543746, 9.817618358456035921 ) ) ;
#2139 = ADVANCED_FACE ( 'NONE', ( #51401 ), #92739, .T. ) ;
#2140 = VERTEX_POINT ( 'NONE', #45779 ) ;
#2141 = CARTESIAN_POINT ( 'NONE',  ( 32.16024265030974050, 0.3587747205144265483, 14.03360796525321774 ) ) ;
#2142 = EDGE_CURVE ( 'NONE', #14697, #92497, #66653, .T. ) ;
#2143 = CARTESIAN_POINT ( 'NONE',  ( -7.596101150008887082, -19.70107428960382734, 11.49999999999999645 ) ) ;
#2144 = CARTESIAN_POINT ( 'NONE',  ( 13.35222405703702186, 17.66689192352044913, -1.500000000000002220 ) ) ;
#2145 = EDGE_CURVE ( 'NONE', #18949, #85237, #56873, .T. ) ;
#2146 = CARTESIAN_POINT ( 'NONE',  ( -14.18348626307465743, -14.89297910716571849, 11.49999999999998934 ) ) ;
#2147 = ORIENTED_EDGE ( 'NONE', *, *, #88168, .F. ) ;
#2148 = CARTESIAN_POINT ( 'NONE',  ( -66.52287095715006160, -23.47596703998600631, 11.44779298504228748 ) ) ;
#2149 = VERTEX_POINT ( 'NONE', #30546 ) ;
#2150 = CARTESIAN_POINT ( 'NONE',  ( -54.50804670033233634, -23.96119346886879953, -0.6495511937832153526 ) ) ;
#2151 = CARTESIAN_POINT ( 'NONE',  ( -85.62287095715005592, -23.47593901973091235, -1.443836447539002865 ) ) ;
#2152 = ORIENTED_EDGE ( 'NONE', *, *, #37751, .F. ) ;
#2153 = ORIENTED_EDGE ( 'NONE', *, *, #85977, .F. ) ;
#2154 = ORIENTED_EDGE ( 'NONE', *, *, #72761, .T. ) ;
#2155 = CARTESIAN_POINT ( 'NONE',  ( -100.5228709571500758, -24.14321612903116687, -0.2833117244521499156 ) ) ;
#2156 = LINE ( 'NONE', #54931, #58393 ) ;
#2157 = CARTESIAN_POINT ( 'NONE',  ( -91.62287095715004170, -23.48783264082478794, -1.443836473390063713 ) ) ;
#2158 = CARTESIAN_POINT ( 'NONE',  ( 20.67342648114324533, -1.018679444107209342, -1.500000000000002220 ) ) ;
#2159 = CARTESIAN_POINT ( 'NONE',  ( -2.787017431591729988, -21.48445716988565835, 11.49999999999999645 ) ) ;
#2160 = ORIENTED_EDGE ( 'NONE', *, *, #9653, .T. ) ;
#2161 = VECTOR ( 'NONE', #73780, 1000.000000000000227 ) ;
#2162 = CARTESIAN_POINT ( 'NONE',  ( -60.52287095715005449, -24.15516710230758690, 10.28746687062794152 ) ) ;
#2163 = CARTESIAN_POINT ( 'NONE',  ( 2.628295812946869425, -5.876774720514411854, 19.40849182188139110 ) ) ;
#2164 = CARTESIAN_POINT ( 'NONE',  ( 11.64234319522276095, -19.14997049866658330, 11.49999999999998934 ) ) ;
#2165 = PLANE ( 'NONE',  #86966 ) ;
#2166 = CARTESIAN_POINT ( 'NONE',  ( -71.62287095715005592, -23.48786465467241413, 11.44779295918254469 ) ) ;
#2167 = ORIENTED_EDGE ( 'NONE', *, *, #54005, .F. ) ;
#2168 = CARTESIAN_POINT ( 'NONE',  ( 29.72131469344797239, 6.278265095287072661, 26.95488797742164877 ) ) ;
#2169 = CARTESIAN_POINT ( 'NONE',  ( -120.6228709571500559, -23.48786465467241769, 11.44779295918253759 ) ) ;
#2170 = VECTOR ( 'NONE', #99538, 1000.000000000000114 ) ;
#2171 = EDGE_LOOP ( 'NONE', ( #66024, #70525, #40165, #28479 ) ) ;
#2172 = ORIENTED_EDGE ( 'NONE', *, *, #30820, .F. ) ;
#2173 = FACE_BOUND ( 'NONE', #61977, .T. ) ;
#2174 = ORIENTED_EDGE ( 'NONE', *, *, #58731, .F. ) ;
#2175 = PLANE ( 'NONE',  #94065 ) ;
#2176 = B_SPLINE_CURVE_WITH_KNOTS ( 'NONE', 3,
 ( #24067, #94080, #6851, #47420, #14955, #62656, #61657, #93077, #31180, #14455, #32181, #39296, #15455, #92083, #78348, #46917 ),
 .UNSPECIFIED., .F., .F.,
 ( 4, 2, 2, 2, 2, 2, 2, 4 ),
 ( 0.000000000000000000, 0.0002756755153052838146, 0.0005513510306105676292, 0.001102702061221115526, 0.001378377576526390071, 0.001654053091831664615, 0.001929728607136938943, 0.002205404122442214572 ),
 .UNSPECIFIED. ) ;
#2177 = CARTESIAN_POINT ( 'NONE',  ( 20.85495618715548716, -4.085033163991189653, -1.500000000000002220 ) ) ;
#2178 = ORIENTED_EDGE ( 'NONE', *, *, #51492, .T. ) ;
#2179 = FACE_OUTER_BOUND ( 'NONE', #39740, .T. ) ;
#2180 = CARTESIAN_POINT ( 'NONE',  ( -21.66901994843296819, -2.608494568651300138, -1.500000000000002220 ) ) ;
#2181 = CARTESIAN_POINT ( 'NONE',  ( -52.54157490255303742, -24.35071581493542681, 9.817618358456037697 ) ) ;
#2182 = PLANE ( 'NONE',  #14498 ) ;
#2183 = CARTESIAN_POINT ( 'NONE',  ( 6.365284455128204399, -5.876774720514413630, 19.73076923076922640 ) ) ;
#2184 = CARTESIAN_POINT ( 'NONE',  ( 8.256513476402210117, 20.27555108428041208, -1.500000000000002220 ) ) ;
#2185 = CARTESIAN_POINT ( 'NONE',  ( -30.57287095715006231, -23.47596702059239604, 11.43887032355635647 ) ) ;
#2186 = ORIENTED_EDGE ( 'NONE', *, *, #84467, .F. ) ;
#2187 = FACE_OUTER_BOUND ( 'NONE', #42554, .T. ) ;
#2188 = CARTESIAN_POINT ( 'NONE',  ( -48.87479414115020404, -25.26337311648806505, 6.180417640909889876 ) ) ;
#2189 = ORIENTED_EDGE ( 'NONE', *, *, #49385, .T. ) ;
#2190 = ORIENTED_EDGE ( 'NONE', *, *, #25403, .T. ) ;
#2191 = VECTOR ( 'NONE', #64908, 1000.000000000000000 ) ;
#2192 = EDGE_LOOP ( 'NONE', ( #92417, #42503, #1396, #21494 ) ) ;
#2193 = CARTESIAN_POINT ( 'NONE',  ( -58.55620429048339304, -24.64965694238575011, 8.947790433994200043 ) ) ;
#2194 = CARTESIAN_POINT ( 'NONE',  ( -31.24388727629347784, -25.31586941165988236, 4.461292436448222709 ) ) ;
#2195 = CARTESIAN_POINT ( 'NONE',  ( 10.86157628581156764, 18.25448884030880592, -1.500000000000002220 ) ) ;
#2196 = CARTESIAN_POINT ( 'NONE',  ( -8.499999999999987566, 18.74999999999999645, 2.100000000000000089 ) ) ;
#2197 = CARTESIAN_POINT ( 'NONE',  ( -30.59367615247571592, -24.87212640336024805, 1.420893871182736579 ) ) ;
#2198 = EDGE_CURVE ( 'NONE', #34988, #6691, #85775, .T. ) ;
#2199 = PLANE ( 'NONE',  #51884 ) ;
#2200 = CARTESIAN_POINT ( 'NONE',  ( -48.62287095715004881, -23.47596703998600276, 11.44779298504227505 ) ) ;
#2202 = CARTESIAN_POINT ( 'NONE',  ( 7.305494252837257285, 17.95555029072639286, -1.500000000000002220 ) ) ;
#2201 = VECTOR ( 'NONE', #51397, 1000.000000000000114 ) ;
#2203 = EDGE_CURVE ( 'NONE', #44804, #28633, #87035, .T. ) ;
#2204 = CARTESIAN_POINT ( 'NONE',  ( -45.59298552244553093, -24.40034930558990922, 0.3402023900116019073 ) ) ;
#2205 = ORIENTED_EDGE ( 'NONE', *, *, #49340, .F. ) ;
#2206 = CARTESIAN_POINT ( 'NONE',  ( -19.34354882100874562, 2.624169249526263403, 11.49999999999999645 ) ) ;
#2207 = CARTESIAN_POINT ( 'NONE',  ( -5.486124437288584232, -6.376774720514417183, 19.74568812963598319 ) ) ;
#2208 = VECTOR ( 'NONE', #77039, 1000.000000000000114 ) ;
#2209 = DIRECTION ( 'NONE',  ( 0.000000000000000000, 0.000000000000000000, 1.000000000000000000 ) ) ;
#2210 = ORIENTED_EDGE ( 'NONE', *, *, #62270, .T. ) ;
#2211 = DIRECTION ( 'NONE',  ( -1.000000000000000000, -3.491481338843133355E-15, -2.352173255807796056E-16 ) ) ;
#2212 = CARTESIAN_POINT ( 'NONE',  ( -119.5562042904833788, -24.64965694238574656, 8.947790433994191162 ) ) ;
#2213 = CARTESIAN_POINT ( 'NONE',  ( -90.52287095715013265, -24.83602698348160231, 1.605859176311266179 ) ) ;
#2214 = CARTESIAN_POINT ( 'NONE',  ( -81.60636161561390622, -25.03155942975127246, 7.020725065118214481 ) ) ;
#2215 = CARTESIAN_POINT ( 'NONE',  ( 10.71975780190685690, -16.47196428025586812, 11.49999999999998934 ) ) ;
#2216 = ORIENTED_EDGE ( 'NONE', *, *, #83961, .T. ) ;
#2217 = LINE ( 'NONE', #80324, #78069 ) ;
#2218 = DIRECTION ( 'NONE',  ( 0.000000000000000000, -0.9999999999976377785, -2.173523156925979128E-06 ) ) ;
#2219 = EDGE_CURVE ( 'NONE', #88543, #23364, #47286, .T. ) ;
#2220 = COORDINATED_UNIVERSAL_TIME_OFFSET ( 0, 0, .AHEAD. ) ;
#2221 = CARTESIAN_POINT ( 'NONE',  ( 3.063121397228215859, -5.876774720514419847, 20.95210102656095685 ) ) ;
#2222 = CARTESIAN_POINT ( 'NONE',  ( -33.52287095715006160, -29.50250243563736774, 8.947779886222150481 ) ) ;
#2223 = CARTESIAN_POINT ( 'NONE',  ( -105.5562042904834072, -23.48786465467241769, 11.44779295918254292 ) ) ;
#2224 = CARTESIAN_POINT ( 'NONE',  ( -50.40445135320379677, -29.50249014687182836, 3.293933732389337621 ) ) ;
#2225 = FACE_OUTER_BOUND ( 'NONE', #97700, .T. ) ;
#2226 = CARTESIAN_POINT ( 'NONE',  ( -43.62287095715004881, -24.66019654487199020, 8.947790411086135265 ) ) ;
#2227 = CARTESIAN_POINT ( 'NONE',  ( -69.34512923434627396, -25.31201765456443198, 6.118189256283883104 ) ) ;
#2228 = DIRECTION ( 'NONE',  ( -0.000000000000000000, -0.000000000000000000, -1.000000000000000000 ) ) ;
#2229 = CARTESIAN_POINT ( 'NONE',  ( -11.57717615966994273, 16.22069937712612031, -1.500000000000002220 ) ) ;
#2230 = AXIS2_PLACEMENT_3D ( 'NONE', #30112, #168, #91018 ) ;
#2231 = CARTESIAN_POINT ( 'NONE',  ( -100.8449020736807711, -25.20544635972949266, 3.368783707514380499 ) ) ;
#2232 = CARTESIAN_POINT ( 'NONE',  ( 6.283368587668265448, -18.83516890145298106, -1.500000000000002220 ) ) ;
#2233 = ORIENTED_EDGE ( 'NONE', *, *, #82441, .F. ) ;
#2234 = CARTESIAN_POINT ( 'NONE',  ( -115.5228709571500616, -25.00158670708909625, 2.256160236439166411 ) ) ;
#2235 = AXIS2_PLACEMENT_3D ( 'NONE', #66799, #67286, #21087 ) ;
#2236 = CARTESIAN_POINT ( 'NONE',  ( 8.499999999999989342, 18.99999999999977973, 0.000000000000000000 ) ) ;
#2237 = CARTESIAN_POINT ( 'NONE',  ( 1.255616527394258553, 17.95615290467683778, 9.000000000000000000 ) ) ;
#2238 = CARTESIAN_POINT ( 'NONE',  ( -7.357705842588929457, 19.43699106120834230, 11.49999999999999645 ) ) ;
#2239 = FACE_OUTER_BOUND ( 'NONE', #63813, .T. ) ;
#2240 = DIRECTION ( 'NONE',  ( 1.000000000000000000, 3.773278334444167608E-23, 8.201307833595939069E-29 ) ) ;
#2241 = CARTESIAN_POINT ( 'NONE',  ( 22.67573665902413182, 1.879276792517311501, 11.49999999999999645 ) ) ;
#2242 = VERTEX_POINT ( 'NONE', #62511 ) ;
#2243 = CARTESIAN_POINT ( 'NONE',  ( -91.62287095715004170, -24.50216790748205753, 0.6166512839542586111 ) ) ;
#2244 = LINE ( 'NONE', #34189, #71142 ) ;
#2245 = ORIENTED_EDGE ( 'NONE', *, *, #13130, .F. ) ;
#2246 = CARTESIAN_POINT ( 'NONE',  ( -14.42758394406654610, -14.16023863206117994, -1.500000000000002220 ) ) ;
#2247 = DIRECTION ( 'NONE',  ( 0.000000000000000000, 0.000000000000000000, 1.000000000000000000 ) ) ;
#2248 = CARTESIAN_POINT ( 'NONE',  ( -69.52287095715009002, -23.48783264082477018, -1.443836473390092801 ) ) ;
#2249 = EDGE_CURVE ( 'NONE', #67044, #71424, #63002, .T. ) ;
#2250 = EDGE_CURVE ( 'NONE', #59253, #19418, #50745, .T. ) ;
#2251 = ORIENTED_EDGE ( 'NONE', *, *, #35979, .F. ) ;
#2252 = DIRECTION ( 'NONE',  ( -0.000000000000000000, -0.000000000000000000, 1.000000000000000000 ) ) ;
#2253 = CARTESIAN_POINT ( 'NONE',  ( -51.62287095715004881, -24.51283580621364067, 0.6167428607019803666 ) ) ;
#2254 = CARTESIAN_POINT ( 'NONE',  ( -20.00956492049148494, -0.6725752471728385640, -1.500000000000002220 ) ) ;
#2255 = DIRECTION ( 'NONE',  ( 1.000000000000000000, -0.000000000000000000, -0.000000000000000000 ) ) ;
#2256 = EDGE_CURVE ( 'NONE', #51872, #38706, #25398, .T. ) ;
#2257 = CARTESIAN_POINT ( 'NONE',  ( -19.40599490818632233, 7.965113791304038848, 11.49999999999999645 ) ) ;
#2258 = DIRECTION ( 'NONE',  ( 0.000000000000000000, -1.000000000000000000, 0.000000000000000000 ) ) ;
#2259 = DIRECTION ( 'NONE',  ( 0.000000000000000000, 0.000000000000000000, 1.000000000000000000 ) ) ;
#2260 = CARTESIAN_POINT ( 'NONE',  ( 10.81757466760856801, -19.22619917341675588, 11.49999999999998934 ) ) ;
#2261 = EDGE_CURVE ( 'NONE', #71061, #44804, #55604, .T. ) ;
#2262 = CARTESIAN_POINT ( 'NONE',  ( -127.4728709548940486, -25.40673988423724339, 2.000950539785686821 ) ) ;
#2263 = TOROIDAL_SURFACE ( 'NONE', #81645, 3.060000000000000053, 2.040000000000000036 ) ;
#2264 = VERTEX_POINT ( 'NONE', #77707 ) ;
#2265 = CARTESIAN_POINT ( 'NONE',  ( -36.62287095715005592, -29.50250243563736774, 8.947779886222148704 ) ) ;
#2266 = CARTESIAN_POINT ( 'NONE',  ( -41.62287095715006302, -23.48783264082477729, -1.443836473390071928 ) ) ;
#2267 = CARTESIAN_POINT ( 'NONE',  ( -119.5228709571500758, -29.50248528299804818, 1.056150453629045360 ) ) ;
#2268 = B_SPLINE_CURVE_WITH_KNOTS ( 'NONE', 3,
 ( #23289, #40545, #71497, #56282 ),
 .UNSPECIFIED., .F., .F.,
 ( 4, 4 ),
 ( 0.000000000000000000, 1.000000000000000000 ),
 .UNSPECIFIED. ) ;
#2269 = ORIENTED_EDGE ( 'NONE', *, *, #80574, .T. ) ;
#2270 = CARTESIAN_POINT ( 'NONE',  ( 2.993128331772667572, -6.376774720514402972, 18.53171057923899312 ) ) ;
#2271 = ORIENTED_EDGE ( 'NONE', *, *, #46204, .T. ) ;
#2272 = VECTOR ( 'NONE', #45015, 1000.000000000000000 ) ;
#2273 = B_SPLINE_CURVE_WITH_KNOTS ( 'NONE', 3,
 ( #76769, #54461, #69686, #7270, #44860, #22979 ),
 .UNSPECIFIED., .F., .F.,
 ( 4, 2, 4 ),
 ( 0.000000000000000000, 0.001380764517854766484, 0.002761529035709532967 ),
 .UNSPECIFIED. ) ;
#2274 = VERTEX_POINT ( 'NONE', #8220 ) ;
#2275 = LINE ( 'NONE', #25084, #81052 ) ;
#2276 = LINE ( 'NONE', #18481, #59977 ) ;
#2278 = EDGE_CURVE ( 'NONE', #39077, #4955, #63023, .T. ) ;
#2277 = CARTESIAN_POINT ( 'NONE',  ( -89.81226385320383088, -25.26364009184147008, 3.993462176398974162 ) ) ;
#2279 = CARTESIAN_POINT ( 'NONE',  ( 16.23509277041898358, 12.58620111108425377, -1.500000000000002220 ) ) ;
#2280 = ORIENTED_EDGE ( 'NONE', *, *, #20402, .T. ) ;
#2281 = CARTESIAN_POINT ( 'NONE',  ( 33.00535138976609062, 6.376774720514426953, -12.97242311383962310 ) ) ;
#2282 = CARTESIAN_POINT ( 'NONE',  ( 6.457852148677970305, -5.876774720514416295, 20.09052163342618158 ) ) ;
#2283 = CARTESIAN_POINT ( 'NONE',  ( -124.5228709571500616, -23.47596703998600631, 11.44779298504227860 ) ) ;
#2284 = CARTESIAN_POINT ( 'NONE',  ( -18.97848940637192428, 11.77069306843248064, 11.49999999999998934 ) ) ;
#2285 = CARTESIAN_POINT ( 'NONE',  ( -71.27197200528213727, -25.22889308749096315, 6.453605103024415257 ) ) ;
#2286 = CARTESIAN_POINT ( 'NONE',  ( -1.394533802543915124, -5.876774720514414518, 20.19722303762275573 ) ) ;
#2287 = ORIENTED_EDGE ( 'NONE', *, *, #63312, .F. ) ;
#2288 = CARTESIAN_POINT ( 'NONE',  ( -101.6228709571500275, -23.73907113216992215, -1.053371485793222373 ) ) ;
#2289 = DIRECTION ( 'NONE',  ( 0.000000000000000000, -1.000000000000000000, 4.688851412615178005E-17 ) ) ;
#2290 = CARTESIAN_POINT ( 'NONE',  ( -11.21968731015968856, -17.59241007644406096, 11.49999999999998934 ) ) ;
#2291 = ORIENTED_EDGE ( 'NONE', *, *, #85679, .F. ) ;
#2293 = ORIENTED_EDGE ( 'NONE', *, *, #35247, .T. ) ;
#2292 = PLANE ( 'NONE',  #8497 ) ;
#2294 = ORIENTED_EDGE ( 'NONE', *, *, #36548, .T. ) ;
#2295 = CARTESIAN_POINT ( 'NONE',  ( -68.98049337452070517, -25.03149153121544757, 6.552244914804028930 ) ) ;
#2296 = CARTESIAN_POINT ( 'NONE',  ( 19.40125262130244366, -8.172613994405130811, -1.500000000000002220 ) ) ;
#2297 = EDGE_LOOP ( 'NONE', ( #36569, #72728, #19210, #94236 ) ) ;
#2298 = DIRECTION ( 'NONE',  ( -0.000000000000000000, 1.000000000000000000, -0.000000000000000000 ) ) ;
#2299 = DIRECTION ( 'NONE',  ( -0.000000000000000000, 2.173523156925979552E-06, -0.9999999999976378895 ) ) ;
#2300 = CARTESIAN_POINT ( 'NONE',  ( 4.621320343559255583, 11.49999999999999645, 2.100000000000000089 ) ) ;
#2301 = CARTESIAN_POINT ( 'NONE',  ( -101.3347705957103528, -25.25419498530509443, 7.306917479324832598 ) ) ;
#2302 = CARTESIAN_POINT ( 'NONE',  ( -60.62287095715004881, -24.99156045073392463, 7.747789690856161648 ) ) ;
#2303 = CARTESIAN_POINT ( 'NONE',  ( -15.38093110518717666, 15.28219592669002402, -1.500000000000002220 ) ) ;
#2304 = CARTESIAN_POINT ( 'NONE',  ( -117.6228709571500559, -23.47596703998600631, 11.44779298504227683 ) ) ;
#2306 = ORIENTED_EDGE ( 'NONE', *, *, #10597, .T. ) ;
#2305 = CARTESIAN_POINT ( 'NONE',  ( -18.06118310651259407, 13.05043149098080058, 11.49999999999999645 ) ) ;
#2307 = CARTESIAN_POINT ( 'NONE',  ( -51.11433842476665035, -25.24728772845527303, 5.424622507049278397 ) ) ;
#2308 = CARTESIAN_POINT ( 'NONE',  ( 5.514125806255895004E-17, -29.50247984919044697, -1.443849411171584940 ) ) ;
#2309 = ORIENTED_EDGE ( 'NONE', *, *, #66338, .F. ) ;
#2310 = AXIS2_PLACEMENT_3D ( 'NONE', #44803, #89474, #59529 ) ;
#2312 = ORIENTED_EDGE ( 'NONE', *, *, #34316, .F. ) ;
#2311 = CARTESIAN_POINT ( 'NONE',  ( -6.181720432442950219, -6.376774720514410077, 19.67464842890028720 ) ) ;
#2313 = ADVANCED_FACE ( 'NONE', ( #93946 ), #86343, .F. ) ;
#2314 = VECTOR ( 'NONE', #20957, 1000.000000000000000 ) ;
#2315 = ORIENTED_EDGE ( 'NONE', *, *, #76312, .T. ) ;
#2316 = CARTESIAN_POINT ( 'NONE',  ( 31.30917625415073502, -4.464831821618584051, 0.9454093304329914682 ) ) ;
#2317 = B_SPLINE_CURVE_WITH_KNOTS ( 'NONE', 3,
 ( #25292, #95310, #86693, #63890 ),
 .UNSPECIFIED., .F., .F.,
 ( 4, 4 ),
 ( 0.000000000000000000, 9.999999999998897304E-05 ),
 .UNSPECIFIED. ) ;
#2318 = EDGE_CURVE ( 'NONE', #94960, #19028, #14417, .T. ) ;
#2319 = CARTESIAN_POINT ( 'NONE',  ( 16.68447708738676383, -11.30049470069299922, -1.500000000000002220 ) ) ;
#2320 = CARTESIAN_POINT ( 'NONE',  ( -105.5228709571500616, -25.00158670708909980, 2.256160236439166411 ) ) ;
#2321 = ORIENTED_EDGE ( 'NONE', *, *, #88448, .F. ) ;
#2322 = CARTESIAN_POINT ( 'NONE',  ( -130.5728709571500588, -25.26346845900570059, 3.135843962334224244 ) ) ;
#2323 = CARTESIAN_POINT ( 'NONE',  ( -21.57557905285345612, -6.117077608415351087, -1.500000000000002220 ) ) ;
#2324 = ORIENTED_EDGE ( 'NONE', *, *, #70695, .F. ) ;
#2325 = ORIENTED_EDGE ( 'NONE', *, *, #32578, .T. ) ;
#2326 = CARTESIAN_POINT ( 'NONE',  ( -34.62287095715004881, -23.48783264082478084, -1.443836473390074149 ) ) ;
#2327 = CARTESIAN_POINT ( 'NONE',  ( -101.6270296092226602, -24.35071581493543746, 9.817618358456027039 ) ) ;
#2328 = CARTESIAN_POINT ( 'NONE',  ( -110.5228709571500616, -25.00182538069145366, 7.747789668545101094 ) ) ;
#2329 = CARTESIAN_POINT ( 'NONE',  ( -125.5228709571500616, -24.92579138211051060, 1.929029949967010271 ) ) ;
#2330 = CARTESIAN_POINT ( 'NONE',  ( -97.24679607323146513, -24.75152770810920089, 1.363349870542269526 ) ) ;
#2331 = CARTESIAN_POINT ( 'NONE',  ( -10.41718274906430786, -16.55731393670301088, 11.49999999999998934 ) ) ;
#2332 = DIRECTION ( 'NONE',  ( -3.469446951953614189E-15, 1.000000000000000000, 0.000000000000000000 ) ) ;
#2333 = ORIENTED_EDGE ( 'NONE', *, *, #3203, .T. ) ;
#2334 = CARTESIAN_POINT ( 'NONE',  ( 19.32660459246815421, -9.429101867163046435, 11.49999999999998934 ) ) ;
#2335 = CARTESIAN_POINT ( 'NONE',  ( -128.5557745493626669, -24.15543982623908548, -0.2315651400026392803 ) ) ;
#2336 = CARTESIAN_POINT ( 'NONE',  ( -121.5228709571500758, -23.96127896941631974, -0.6493128931037975837 ) ) ;
#2337 = CARTESIAN_POINT ( 'NONE',  ( 14.43441819135929371, 3.316774720514426456, -28.36222020317710246 ) ) ;
#2338 = CARTESIAN_POINT ( 'NONE',  ( -79.62287095715005592, -29.50247984919015209, -1.443849546365053582 ) ) ;
#2339 = CARTESIAN_POINT ( 'NONE',  ( 4.748521865011817944, 22.44708532425888592, -1.500000000000002220 ) ) ;
#2340 = PRODUCT_RELATED_PRODUCT_CATEGORY ( 'detail', '', ( #42576 ) ) ;
#2341 = SHAPE_DEFINITION_REPRESENTATION ( #87067, #9419 ) ;
#2342 = CARTESIAN_POINT ( 'NONE',  ( -103.2228709571500644, -23.47596703998600631, 11.44779298504227860 ) ) ;
#2343 = CARTESIAN_POINT ( 'NONE',  ( -2.732037236150805626, -5.876774720514412742, 19.78976258633487717 ) ) ;
#2344 = CARTESIAN_POINT ( 'NONE',  ( -3.374260732160392795, -19.82512954709321562, 11.49999999999999645 ) ) ;
#2345 = DIRECTION ( 'NONE',  ( 0.000000000000000000, 1.000000000000000000, 0.000000000000000000 ) ) ;
#2346 = CARTESIAN_POINT ( 'NONE',  ( 14.76093561896379214, -3.316774720514426456, -27.37148769130089931 ) ) ;
#2347 = CYLINDRICAL_SURFACE ( 'NONE', #61988, 1.999999999999963141 ) ;
#2348 = CARTESIAN_POINT ( 'NONE',  ( -38.52287095715006870, -24.64965694238406613, 8.947790433994205372 ) ) ;
#2349 = CARTESIAN_POINT ( 'NONE',  ( -85.62287095715004170, -24.91544648472620338, 1.928969306349226143 ) ) ;
#2350 = CARTESIAN_POINT ( 'NONE',  ( 5.644138345009856117, 19.01542066204735448, -1.500000000000002220 ) ) ;
#2351 = EDGE_CURVE ( 'NONE', #53050, #83993, #31042, .T. ) ;
#2352 = CARTESIAN_POINT ( 'NONE',  ( -68.93918693012690824, -25.25799956426409665, 6.184868438663939649 ) ) ;
#2353 = CARTESIAN_POINT ( 'NONE',  ( 5.239555828037883778, -18.94419173073049478, -1.500000000000002220 ) ) ;
#2354 = CARTESIAN_POINT ( 'NONE',  ( -42.50580221595909336, -23.96119346886880663, -0.6495511937831992544 ) ) ;
#2355 = CARTESIAN_POINT ( 'NONE',  ( -58.62287095715004881, -23.48786465467241769, 11.44779295918254824 ) ) ;
#2356 = CARTESIAN_POINT ( 'NONE',  ( 15.34241074214975065, 3.824162593742471028, -28.48848699765728654 ) ) ;
#2357 = DIRECTION ( 'NONE',  ( -3.773278334453079030E-23, 0.9999999999976377785, 2.173523156925979128E-06 ) ) ;
#2358 = CARTESIAN_POINT ( 'NONE',  ( -20.42507745660439156, -2.452541965221147535, 11.49999999999999645 ) ) ;
#2359 = DIRECTION ( 'NONE',  ( 1.000000000000000000, 3.773278334444166432E-23, 8.201307841325785021E-29 ) ) ;
#2360 = AXIS2_PLACEMENT_3D ( 'NONE', #22404, #52883, #54385 ) ;
#2361 = LINE ( 'NONE', #41930, #93390 ) ;
#2362 = CARTESIAN_POINT ( 'NONE',  ( 10.27952223434480494, 20.12118371629609470, 11.49999999999999645 ) ) ;
#2363 = EDGE_LOOP ( 'NONE', ( #82334, #32170, #99242, #71654 ) ) ;
#2364 = CARTESIAN_POINT ( 'NONE',  ( -69.34542366606198982, -25.12218970343129598, 6.299235195870870108 ) ) ;
#2365 = CARTESIAN_POINT ( 'NONE',  ( -27.68651082257923690, -24.80976250947271211, 7.605672514646787619 ) ) ;
#2366 = CARTESIAN_POINT ( 'NONE',  ( -100.6814946224345846, -25.31648867911425427, 5.043962003566639041 ) ) ;
#2367 = EDGE_CURVE ( 'NONE', #51806, #6550, #9584, .T. ) ;
#2368 = CARTESIAN_POINT ( 'NONE',  ( -27.12300167417273045, -24.93063615898261887, 8.164241745431031205 ) ) ;
#2369 = AXIS2_PLACEMENT_3D ( 'NONE', #52296, #76606, #54306 ) ;
#2370 = DIRECTION ( 'NONE',  ( 1.000000000000000000, 0.000000000000000000, -2.168404344971008868E-16 ) ) ;
#2371 = ORIENTED_EDGE ( 'NONE', *, *, #12527, .F. ) ;
#2372 = CARTESIAN_POINT ( 'NONE',  ( -80.31352994281894553, -25.31596222718856737, 4.969670813418835209 ) ) ;
#2373 = CARTESIAN_POINT ( 'NONE',  ( -22.76716317511769461, -1.676022972194794791, -1.500000000000002220 ) ) ;
#2374 = CARTESIAN_POINT ( 'NONE',  ( -111.1699275071095485, -25.23443226348169333, 3.685496250201802049 ) ) ;
#2375 = CARTESIAN_POINT ( 'NONE',  ( -96.62356410278910346, -24.65952944569305316, 1.056160979905706121 ) ) ;
#2376 = CARTESIAN_POINT ( 'NONE',  ( -82.63299475421938212, -24.15620529776628089, 10.23563542870660825 ) ) ;
#2377 = EDGE_CURVE ( 'NONE', #35831, #18999, #9208, .T. ) ;
#2378 = CARTESIAN_POINT ( 'NONE',  ( 1.786768808452938950, -22.39398889530128756, 11.49999999999999645 ) ) ;
#2379 = ORIENTED_EDGE ( 'NONE', *, *, #13484, .F. ) ;
#2380 = CARTESIAN_POINT ( 'NONE',  ( -49.62287095715005592, -29.50250786944525672, 11.44777988621624054 ) ) ;
#2381 = CARTESIAN_POINT ( 'NONE',  ( -21.79611004543898289, 2.820803583321412678, -1.500000000000002220 ) ) ;
#2382 = ADVANCED_FACE ( 'NONE', ( #48290 ), #18332, .F. ) ;
#2383 = CARTESIAN_POINT ( 'NONE',  ( -126.1692003789631968, -25.31326721218303888, 3.500953664922433095 ) ) ;
#2384 = CARTESIAN_POINT ( 'NONE',  ( -34.49701390240621635, -24.15620529776627379, 10.23563542870661003 ) ) ;
#2385 = DIRECTION ( 'NONE',  ( 1.000000000000000000, 3.773278334444166432E-23, 8.201307841325785021E-29 ) ) ;
#2386 = ORIENTED_EDGE ( 'NONE', *, *, #88943, .F. ) ;
#2387 = DIRECTION ( 'NONE',  ( -0.000000000000000000, -1.000000000000000000, -0.000000000000000000 ) ) ;
#2388 = CARTESIAN_POINT ( 'NONE',  ( -112.5895376238167103, -24.66019654487199730, 8.947790411086121054 ) ) ;
#2389 = ORIENTED_EDGE ( 'NONE', *, *, #55978, .F. ) ;
#2390 = CARTESIAN_POINT ( 'NONE',  ( -17.91610926057384034, -10.00117247862695358, -1.500000000000002220 ) ) ;
#2391 = ORIENTED_EDGE ( 'NONE', *, *, #1204, .T. ) ;
#2392 = ORIENTED_EDGE ( 'NONE', *, *, #91451, .F. ) ;
#2393 = ORIENTED_EDGE ( 'NONE', *, *, #35572, .T. ) ;
#2394 = EDGE_LOOP ( 'NONE', ( #40682, #37753, #79784, #70316 ) ) ;
#2395 = CYLINDRICAL_SURFACE ( 'NONE', #80979, 28.96799999999999642 ) ;
#2396 = CARTESIAN_POINT ( 'NONE',  ( 3.535601659403828201, -22.84449096179584160, -1.500000000000002220 ) ) ;
#2398 = EDGE_CURVE ( 'NONE', #98622, #77754, #49300, .T. ) ;
#2397 = CARTESIAN_POINT ( 'NONE',  ( -41.52287095715005449, -24.66019654487198665, 8.947790411086121054 ) ) ;
#2399 = B_SPLINE_CURVE_WITH_KNOTS ( 'NONE', 3,
 ( #69574, #47740, #23882, #32508 ),
 .UNSPECIFIED., .F., .F.,
 ( 4, 4 ),
 ( 0.000000000000000000, 0.0001000000000000028644 ),
 .UNSPECIFIED. ) ;
#2400 = CARTESIAN_POINT ( 'NONE',  ( 12.22771034161782566, -16.27230226814707947, -1.500000000000002220 ) ) ;
#2401 = VERTEX_POINT ( 'NONE', #64039 ) ;
#2402 = PLANE ( 'NONE',  #20171 ) ;
#2403 = CARTESIAN_POINT ( 'NONE',  ( -88.62287095715004170, -24.65952944569304606, 1.056160979905700570 ) ) ;
#2404 = CARTESIAN_POINT ( 'NONE',  ( -46.62287095715004881, -24.65952944569304250, 1.056160979905693020 ) ) ;
#2405 = CARTESIAN_POINT ( 'NONE',  ( 4.127614219445591814, -5.876774720514409189, 18.60403502951120558 ) ) ;
#2407 = ORIENTED_EDGE ( 'NONE', *, *, #73948, .T. ) ;
#2406 = CARTESIAN_POINT ( 'NONE',  ( -21.28347836979250118, 3.227085873532868021, 11.49999999999999645 ) ) ;
#2408 = CARTESIAN_POINT ( 'NONE',  ( -29.19847332116389538, -24.76881234832665868, 4.026236479318956896 ) ) ;
#2409 = CARTESIAN_POINT ( 'NONE',  ( -49.26189073845563371, -25.31573744820669702, 4.538720682593869959 ) ) ;
#2410 = EDGE_LOOP ( 'NONE', ( #14337, #78421, #68353, #8266 ) ) ;
#2411 = B_SPLINE_CURVE_WITH_KNOTS ( 'NONE', 3,
 ( #10220, #11220, #88348, #41176 ),
 .UNSPECIFIED., .F., .F.,
 ( 4, 4 ),
 ( 0.000000000000000000, 9.999999999998897304E-05 ),
 .UNSPECIFIED. ) ;
#2412 = CARTESIAN_POINT ( 'NONE',  ( 4.358738815032396907, -20.29635662749097236, 11.49999999999998934 ) ) ;
#2413 = ORIENTED_EDGE ( 'NONE', *, *, #67881, .T. ) ;
#2415 = ORIENTED_EDGE ( 'NONE', *, *, #58727, .F. ) ;
#2414 = CARTESIAN_POINT ( 'NONE',  ( -125.5569694553999085, -23.48783264082478794, -1.443836473390061936 ) ) ;
#2416 = CARTESIAN_POINT ( 'NONE',  ( -82.62287095715005592, -24.64898659630367916, 1.056161002820826145 ) ) ;
#2417 = CARTESIAN_POINT ( 'NONE',  ( -102.6228709571501128, -23.94994826722516379, -0.6494450866351678675 ) ) ;
#2418 = ORIENTED_EDGE ( 'NONE', *, *, #96884, .T. ) ;
#2419 = ORIENTED_EDGE ( 'NONE', *, *, #37289, .T. ) ;
#2420 = CARTESIAN_POINT ( 'NONE',  ( -6.775140224358976226, -5.876774720514409189, 19.14743589743590846 ) ) ;
#2421 = CARTESIAN_POINT ( 'NONE',  ( -123.6228709571500559, -24.64965695001469115, 8.947790433994175174 ) ) ;
#2422 = CARTESIAN_POINT ( 'NONE',  ( 1.876957540558651605, -5.558144974487054135, 0.000000000000000000 ) ) ;
#2424 = VERTEX_POINT ( 'NONE', #25440 ) ;
#2423 = CARTESIAN_POINT ( 'NONE',  ( 18.76863814860013235, 11.56883167669432133, 11.49999999999999645 ) ) ;
#2425 = CARTESIAN_POINT ( 'NONE',  ( -103.6267870571919048, -24.34968618360933945, 0.1864209137778842229 ) ) ;
#2426 = CARTESIAN_POINT ( 'NONE',  ( -19.94007547503736788, -10.58355046294204094, 11.49999999999998934 ) ) ;
#2428 = ORIENTED_EDGE ( 'NONE', *, *, #23303, .T. ) ;
#2427 = CARTESIAN_POINT ( 'NONE',  ( -70.62287095715004170, -24.51163499207175889, 0.6490370598554249248 ) ) ;
#2429 = VERTEX_POINT ( 'NONE', #95953 ) ;
#2430 = CARTESIAN_POINT ( 'NONE',  ( -20.77875734969026311, -6.143225279485574397, 29.49402280011862487 ) ) ;
#2431 = VECTOR ( 'NONE', #14573, 1000.000000000000000 ) ;
#2432 = EDGE_CURVE ( 'NONE', #98613, #76732, #77309, .T. ) ;
#2433 = CARTESIAN_POINT ( 'NONE',  ( -94.52287095715006160, -24.64898659630367916, 1.056161002820827921 ) ) ;
#2434 = ORIENTED_EDGE ( 'NONE', *, *, #83260, .T. ) ;
#2435 = CARTESIAN_POINT ( 'NONE',  ( -10.94853654022341516, 18.13385389444049522, 11.49999999999998934 ) ) ;
#2436 = CARTESIAN_POINT ( 'NONE',  ( -61.52287095715006160, -29.50248528299804818, 1.056150453629034924 ) ) ;
#2437 = CARTESIAN_POINT ( 'NONE',  ( -58.85672945663861810, -25.29489609436097552, 6.057563354383566967 ) ) ;
#2438 = CARTESIAN_POINT ( 'NONE',  ( -6.720452724358975338, -5.876774720514411854, 19.46153846153846700 ) ) ;
#2439 = CARTESIAN_POINT ( 'NONE',  ( -80.62287095715004170, -24.15516710230296837, 10.28746687063728515 ) ) ;
#2440 = CARTESIAN_POINT ( 'NONE',  ( -5.994446910899359438, -21.39327697068355505, -1.500000000000002220 ) ) ;
#2441 = PLANE ( 'NONE',  #77560 ) ;
#2442 = VECTOR ( 'NONE', #3286, 1000.000000000000114 ) ;
#2443 = ORIENTED_EDGE ( 'NONE', *, *, #4451, .F. ) ;
#2444 = CARTESIAN_POINT ( 'NONE',  ( -5.514838905578028694, -6.376774720514410077, 19.81240905262003338 ) ) ;
#2445 = CARTESIAN_POINT ( 'NONE',  ( -85.62287095715005592, -29.50247984919015209, -1.443849546365051806 ) ) ;
#2446 = CARTESIAN_POINT ( 'NONE',  ( -18.32239908988104204, -6.426282940459683068, 11.49999999999999645 ) ) ;
#2448 = B_SPLINE_CURVE_WITH_KNOTS ( 'NONE', 3,
 ( #77304, #8814, #16407, #37760, #15410, #7806 ),
 .UNSPECIFIED., .F., .F.,
 ( 4, 2, 4 ),
 ( 1.570887131794795405E-05, 0.001396322306279762808, 0.002776935741241577573 ),
 .UNSPECIFIED. ) ;
#2447 = CARTESIAN_POINT ( 'NONE',  ( -40.62376381424373051, -25.11178338647325603, 2.840340238540807416 ) ) ;
#2449 = LINE ( 'NONE', #47127, #76100 ) ;
#2450 = CARTESIAN_POINT ( 'NONE',  ( 8.918240691521024388, 17.32521578647535776, 11.49999999999998934 ) ) ;
#2451 = CARTESIAN_POINT ( 'NONE',  ( -0.4629837013611828866, -21.40787533109759977, 11.49999999999998934 ) ) ;
#2452 = CARTESIAN_POINT ( 'NONE',  ( -32.58953762381671737, -24.64965694238406613, 8.947790433994661896 ) ) ;
#2453 = FACE_OUTER_BOUND ( 'NONE', #97474, .T. ) ;
#2454 = CARTESIAN_POINT ( 'NONE',  ( -51.58729945987563070, -24.34968618360933590, 0.1864209137778788938 ) ) ;
#2455 = LINE ( 'NONE', #33389, #63862 ) ;
#2456 = CARTESIAN_POINT ( 'NONE',  ( 5.860688371469950475, 21.97560254587667217, -1.500000000000002220 ) ) ;
#2457 = EDGE_CURVE ( 'NONE', #15382, #81082, #54337, .T. ) ;
#2458 = CARTESIAN_POINT ( 'NONE',  ( 22.81109547471982424, -6.477225279485574916, -18.46686179409244133 ) ) ;
#2459 = CARTESIAN_POINT ( 'NONE',  ( -106.5889851739996317, -24.35071581493544457, 9.817618358456019934 ) ) ;
#2460 = CARTESIAN_POINT ( 'NONE',  ( -80.52287095715009002, -24.14321612903115977, -0.2833117244521555222 ) ) ;
#2461 = CARTESIAN_POINT ( 'NONE',  ( -18.69216024341242743, -6.879743215651725308, 11.49999999999999645 ) ) ;
#2462 = CARTESIAN_POINT ( 'NONE',  ( -1.751198251822016161, 22.56127314141087581, 0.000000000000000000 ) ) ;
#2463 = EDGE_CURVE ( 'NONE', #68328, #44325, #13157, .T. ) ;
#2464 = CARTESIAN_POINT ( 'NONE',  ( -29.49875734969026198, 0.3587747205144265483, 10.11402280011862587 ) ) ;
#2465 = CARTESIAN_POINT ( 'NONE',  ( -8.599999999999997868, 24.84999999999999787, 0.000000000000000000 ) ) ;
#2466 = ORIENTED_EDGE ( 'NONE', *, *, #79934, .T. ) ;
#2467 = CARTESIAN_POINT ( 'NONE',  ( -96.62287095715005592, -23.47596703998600631, 11.44779298504227860 ) ) ;
#2468 = CARTESIAN_POINT ( 'NONE',  ( -31.81571590327885701, -25.16202561908117730, 2.791798636425737445 ) ) ;
#2469 = LINE ( 'NONE', #48150, #5852 ) ;
#2470 = CARTESIAN_POINT ( 'NONE',  ( -6.994818212361641585, 20.52682044044541598, 11.49999999999998934 ) ) ;
#2471 = EDGE_CURVE ( 'NONE', #44562, #991, #72134, .T. ) ;
#2472 = FACE_OUTER_BOUND ( 'NONE', #9381, .T. ) ;
#2473 = CARTESIAN_POINT ( 'NONE',  ( -7.634514033349506512, -17.95459398628807435, -1.500000000000002220 ) ) ;
#2474 = EDGE_CURVE ( 'NONE', #32256, #75656, #2411, .T. ) ;
#2475 = CARTESIAN_POINT ( 'NONE',  ( 22.81105451610979173, 2.682774720514426559, -18.46691820600746681 ) ) ;
#2476 = ORIENTED_EDGE ( 'NONE', *, *, #669, .F. ) ;
#2477 = EDGE_CURVE ( 'NONE', #44429, #47230, #81059, .T. ) ;
#2478 = AXIS2_PLACEMENT_3D ( 'NONE', #78693, #15304, #69611 ) ;
#2479 = CARTESIAN_POINT ( 'NONE',  ( -16.75749313124890350, -11.57646860041911019, 11.49999999999999645 ) ) ;
#2480 = CARTESIAN_POINT ( 'NONE',  ( -85.62287095715005592, -23.47593901973091235, -1.443836447539002865 ) ) ;
#2481 = CARTESIAN_POINT ( 'NONE',  ( 3.138110291115776995, 11.54688212118755075, -3.549999999999999822 ) ) ;
#2482 = ORIENTED_EDGE ( 'NONE', *, *, #68508, .F. ) ;
#2483 = CARTESIAN_POINT ( 'NONE',  ( 8.160000000000000142, -10.65233964170348635, 1.211157557776864291 ) ) ;
#2484 = FACE_OUTER_BOUND ( 'NONE', #4222, .T. ) ;
#2485 = CARTESIAN_POINT ( 'NONE',  ( 7.479587785762670471, -6.376774720514417183, 20.73799387832858088 ) ) ;
#2486 = CARTESIAN_POINT ( 'NONE',  ( -4.568292318365942073, 5.965225279485572685, 30.06720597538392425 ) ) ;
#2487 = B_SPLINE_CURVE_WITH_KNOTS ( 'NONE', 3,
 ( #14077, #15578, #38923, #30813, #69877, #45055 ),
 .UNSPECIFIED., .F., .F.,
 ( 4, 2, 4 ),
 ( 6.384118678613282972E-06, 0.001386860460828377370, 0.002767336802978141459 ),
 .UNSPECIFIED. ) ;
#2488 = DIRECTION ( 'NONE',  ( -3.469446951953614189E-15, 1.000000000000000000, 0.000000000000000000 ) ) ;
#2489 = EDGE_CURVE ( 'NONE', #54228, #47065, #63254, .T. ) ;
#2490 = CARTESIAN_POINT ( 'NONE',  ( -109.5495869374086766, -24.65952944569305316, 1.056160979905708786 ) ) ;
#2491 = ORIENTED_EDGE ( 'NONE', *, *, #78685, .F. ) ;
#2492 = DIRECTION ( 'NONE',  ( 0.000000000000000000, 0.000000000000000000, -1.000000000000000000 ) ) ;
#2493 = CARTESIAN_POINT ( 'NONE',  ( 9.743704349311032686, 20.77413290702584092, 11.49999999999999645 ) ) ;
#2494 = CARTESIAN_POINT ( 'NONE',  ( 15.01325480956343483, 17.08929600257393489, -1.500000000000002220 ) ) ;
#2495 = CARTESIAN_POINT ( 'NONE',  ( -71.25764098586252260, -25.11044779094143564, 7.228272730454482264 ) ) ;
#2496 = FACE_OUTER_BOUND ( 'NONE', #56686, .T. ) ;
#2497 = FACE_OUTER_BOUND ( 'NONE', #37706, .T. ) ;
#2498 = B_SPLINE_CURVE_WITH_KNOTS ( 'NONE', 3,
 ( #66699, #97610, #68167, #59568, #43343, #90500 ),
 .UNSPECIFIED., .F., .F.,
 ( 4, 2, 4 ),
 ( 6.384118678617895914E-06, 0.001386860460828379105, 0.002767336802978140591 ),
 .UNSPECIFIED. ) ;
#2499 = CARTESIAN_POINT ( 'NONE',  ( -69.74074321433934642, -25.16191154851385292, 6.930438937598965232 ) ) ;
#2500 = AXIS2_PLACEMENT_3D ( 'NONE', #91333, #28432, #51788 ) ;
#2501 = CARTESIAN_POINT ( 'NONE',  ( -15.17958814119055155, -15.74432251006154715, 11.49999999999998934 ) ) ;
#2502 = EDGE_CURVE ( 'NONE', #71172, #88549, #3619, .T. ) ;
#2503 = CARTESIAN_POINT ( 'NONE',  ( -69.60238590130140324, -23.73791477778911840, 11.05961554403170766 ) ) ;
#2504 = ADVANCED_FACE ( 'NONE', ( #96453 ), #57912, .T. ) ;
#2505 = FACE_OUTER_BOUND ( 'NONE', #74403, .T. ) ;
#2506 = CARTESIAN_POINT ( 'NONE',  ( 24.71017632900190719, -5.356774720514427379, -0.3523920347467662806 ) ) ;
#2507 = CARTESIAN_POINT ( 'NONE',  ( -58.51506555621022443, -23.73766607897670156, -1.055555164236457344 ) ) ;
#2508 = ORIENTED_EDGE ( 'NONE', *, *, #11711, .F. ) ;
#2509 = CARTESIAN_POINT ( 'NONE',  ( -17.38880980700008294, 10.71821138944157603, -1.500000000000002220 ) ) ;
#2510 = EDGE_LOOP ( 'NONE', ( #70510, #86748, #31405, #29446 ) ) ;
#2511 = ORIENTED_EDGE ( 'NONE', *, *, #21904, .F. ) ;
#2512 = CARTESIAN_POINT ( 'NONE',  ( 3.792298468851710069, -22.70151372599487871, -1.500000000000002220 ) ) ;
#2514 = EDGE_CURVE ( 'NONE', #44951, #75496, #81230, .T. ) ;
#2513 = LINE ( 'NONE', #26841, #11384 ) ;
#2515 = AXIS2_PLACEMENT_3D ( 'NONE', #86016, #16493, #16999 ) ;
#2516 = ORIENTED_EDGE ( 'NONE', *, *, #61885, .F. ) ;
#2517 = CARTESIAN_POINT ( 'NONE',  ( 22.02124265030973760, 3.456774720514426136, 17.35402280011862786 ) ) ;
#2518 = CARTESIAN_POINT ( 'NONE',  ( 23.91005183030481263, 4.132774720514426292, -14.40591128290692069 ) ) ;
#2519 = AXIS2_PLACEMENT_3D ( 'NONE', #87109, #1391, #23702 ) ;
#2520 = ADVANCED_FACE ( 'NONE', ( #4114 ), #13196, .F. ) ;
#2521 = ADVANCED_FACE ( 'NONE', ( #6600 ), #43670, .F. ) ;
#2522 = CARTESIAN_POINT ( 'NONE',  ( -78.58953762381672448, -24.64965694238407679, 8.947790433994653014 ) ) ;
#2523 = DIRECTION ( 'NONE',  ( -1.000000000000000000, 0.000000000000000000, 0.000000000000000000 ) ) ;
#2525 = VERTEX_POINT ( 'NONE', #21310 ) ;
#2524 = CARTESIAN_POINT ( 'NONE',  ( 20.09692647535021948, 7.048664716645152595, 11.49999999999999645 ) ) ;
#2526 = VERTEX_POINT ( 'NONE', #27944 ) ;
#2527 = CARTESIAN_POINT ( 'NONE',  ( -5.994446910899359438, -21.39327697068355505, 11.49999999999998934 ) ) ;
#2528 = CARTESIAN_POINT ( 'NONE',  ( 13.18972694569024640, 15.87703813876158598, -1.500000000000002220 ) ) ;
#2529 = VERTEX_POINT ( 'NONE', #52282 ) ;
#2530 = CARTESIAN_POINT ( 'NONE',  ( -6.499903988472228278, -6.376774720514408301, 19.18381548539529646 ) ) ;
#2531 = CARTESIAN_POINT ( 'NONE',  ( -93.52287095715006160, -29.50248528299804818, 1.056150453629040253 ) ) ;
#2532 = VERTEX_POINT ( 'NONE', #5100 ) ;
#2533 = CARTESIAN_POINT ( 'NONE',  ( -62.62287095715004881, -29.50250786944525672, 11.44777988621623876 ) ) ;
#2534 = ORIENTED_EDGE ( 'NONE', *, *, #59401, .F. ) ;
#2535 = CARTESIAN_POINT ( 'NONE',  ( -58.53402618834690685, -24.66019654487199730, 8.947790411086117501 ) ) ;
#2536 = CARTESIAN_POINT ( 'NONE',  ( -71.29839951630819428, -25.23282476250683004, 6.331943296452392289 ) ) ;
#2537 = CARTESIAN_POINT ( 'NONE',  ( -17.14161228048114438, 11.91956482804130601, -1.500000000000002220 ) ) ;
#2538 = CARTESIAN_POINT ( 'NONE',  ( -11.22809577558575000, 18.72649003030000259, 11.49999999999999645 ) ) ;
#2539 = CARTESIAN_POINT ( 'NONE',  ( -26.64126777428346315, -24.77993686738184209, 7.094644171777847674 ) ) ;
#2540 = CARTESIAN_POINT ( 'NONE',  ( 8.971512145086524725, -7.528487854913503696, -4.499999999999999112 ) ) ;
#2541 = CARTESIAN_POINT ( 'NONE',  ( -9.984083066403742990, 20.14924292131567185, -1.500000000000002220 ) ) ;
#2542 = CARTESIAN_POINT ( 'NONE',  ( 5.579783289733251550, -20.15082174716252794, -1.500000000000002220 ) ) ;
#2543 = CARTESIAN_POINT ( 'NONE',  ( -26.31589504439661198, -24.88149045850647312, 6.467908346933119113 ) ) ;
#2544 = CARTESIAN_POINT ( 'NONE',  ( -57.62287095715004170, -24.33832256526968862, 0.1851278514119866214 ) ) ;
#2545 = DIRECTION ( 'NONE',  ( 0.000000000000000000, 0.000000000000000000, 1.000000000000000000 ) ) ;
#2546 = ORIENTED_EDGE ( 'NONE', *, *, #49910, .F. ) ;
#2547 = AXIS2_PLACEMENT_3D ( 'NONE', #26445, #96445, #48282 ) ;
#2548 = ORIENTED_EDGE ( 'NONE', *, *, #60712, .F. ) ;
#2549 = VERTEX_POINT ( 'NONE', #89839 ) ;
#2550 = CARTESIAN_POINT ( 'NONE',  ( -52.63895471842339902, -24.15543982623907482, -0.2315651400026529916 ) ) ;
#2551 = ORIENTED_EDGE ( 'NONE', *, *, #96329, .T. ) ;
#2552 = CARTESIAN_POINT ( 'NONE',  ( 12.64048258313813733, 17.25876517447949610, -1.500000000000002220 ) ) ;
#2553 = CARTESIAN_POINT ( 'NONE',  ( -4.763361739610138201, -21.85411462188651299, 11.49999999999999645 ) ) ;
#2554 = ORIENTED_EDGE ( 'NONE', *, *, #81857, .T. ) ;
#2555 = CARTESIAN_POINT ( 'NONE',  ( -95.52287095715004739, -23.47593901973090169, -1.443836447538996648 ) ) ;
#2556 = CARTESIAN_POINT ( 'NONE',  ( 13.75562813033083742, -15.94169299924578453, -1.500000000000002220 ) ) ;
#2557 = CARTESIAN_POINT ( 'NONE',  ( -30.55797716464545744, -24.27484564323477656, 9.960304333224314632 ) ) ;
#2558 = CARTESIAN_POINT ( 'NONE',  ( -15.73602684802347440, -12.20685706852216867, -1.500000000000002220 ) ) ;
#2559 = APPLICATION_CONTEXT ( 'configuration controlled 3d designs of mechanical parts and assemblies' ) ;
#2560 =( BOUNDED_SURFACE ( )  B_SPLINE_SURFACE ( 3, 1, ( 
 ( #75581, #83704 ),
 ( #14690, #76579 ),
 ( #14185, #22786 ),
 ( #5587, #77081 ),
 ( #38532, #45162 ),
 ( #7083, #76086 ),
 ( #38034, #6084 ),
 ( #83199, #84701 ),
 ( #90824, #37539 ),
 ( #30418, #15192 ),
 ( #52269, #67499 ),
 ( #68983, #30918 ),
 ( #99907, #68489 ),
 ( #61888, #61389 ),
 ( #51773, #70491 ),
 ( #94314, #25305 ),
 ( #54278, #72001 ),
 ( #974, #31928 ),
 ( #24800, #86210 ),
 ( #469, #55780 ) ),
 .UNSPECIFIED., .F., .F., .T. ) 
 B_SPLINE_SURFACE_WITH_KNOTS ( ( 4, 3, 1, 1, 3, 3, 1, 1, 3, 4 ),
 ( 2, 2 ),
 ( 0.000000000000000000, 0.1255889732084984889, 0.1669421422606964800, 0.2082953113128944711, 0.2496484803650923512, 0.7477322152634136021, 0.7890853843156119263, 0.8304385533678104725, 0.8717917224200087967, 1.000000000000000000 ),
 ( 0.000000000000000000, 1.000000000000000000 ),
 .UNSPECIFIED. ) 
 GEOMETRIC_REPRESENTATION_ITEM ( )  RATIONAL_B_SPLINE_SURFACE ( (
 ( 0.9999602609241470264, 0.9999602609241470264),
 ( 0.9987387818499366965, 0.9987387818499366965),
 ( 0.9998573533027315108, 0.9998573533027315108),
 ( 1.003315975282531802, 1.003315975282531802),
 ( 1.003315975282531802, 1.003315975282531802),
 ( 1.003315975282531802, 1.003315975282531802),
 ( 1.003315975282531802, 1.003315975282531802),
 ( 1.003315975282531802, 1.003315975282531802),
 ( 1.003315975282531802, 1.003315975282531802),
 ( 0.9773170091682806815, 0.9773170091682806815),
 ( 0.9773170091682806815, 0.9773170091682806815),
 ( 1.003315975282531802, 1.003315975282531802),
 ( 1.003315975282531802, 1.003315975282531802),
 ( 1.003315975282531802, 1.003315975282531802),
 ( 1.003315975282531802, 1.003315975282531802),
 ( 1.003315975282531802, 1.003315975282531802),
 ( 1.003315975282531802, 1.003315975282531802),
 ( 0.9997852197113853423, 0.9997852197113853423),
 ( 0.9986931415022445302, 0.9986931415022445302),
 ( 1.000039740655109810, 1.000039740655109810) ) ) 
 REPRESENTATION_ITEM ( '' )  SURFACE ( )  );
#2561 = FACE_OUTER_BOUND ( 'NONE', #11599, .T. ) ;
#2562 = CARTESIAN_POINT ( 'NONE',  ( -35.52287095715006870, -23.48786465467240347, 11.44779295918255180 ) ) ;
#2563 = CARTESIAN_POINT ( 'NONE',  ( 3.837975233861466329, 21.70421690940786874, -1.500000000000002220 ) ) ;
#2564 = EDGE_LOOP ( 'NONE', ( #62049, #66160, #43863, #51080 ) ) ;
#2565 = CARTESIAN_POINT ( 'NONE',  ( -65.50511328601497496, -24.15602025860896518, 10.28564288303534724 ) ) ;
#2566 = DIRECTION ( 'NONE',  ( -0.000000000000000000, 1.000000000000000000, -0.000000000000000000 ) ) ;
#2567 = CARTESIAN_POINT ( 'NONE',  ( -30.64752034897746924, -23.47593901973090169, -1.443836447538997758 ) ) ;
#2568 = CARTESIAN_POINT ( 'NONE',  ( -28.39957058925135414, -24.99626215692908815, 7.214475432169975555 ) ) ;
#2569 = CARTESIAN_POINT ( 'NONE',  ( -25.78500995861852019, -24.78937058933301785, 3.117906490743990844 ) ) ;
#2570 = CARTESIAN_POINT ( 'NONE',  ( -61.58953762381672448, -24.65952944569304606, 1.056160979905703234 ) ) ;
#2571 = CARTESIAN_POINT ( 'NONE',  ( -21.20786952941880443, -2.223526401999901925, 11.49999999999998934 ) ) ;
#2572 = CARTESIAN_POINT ( 'NONE',  ( -27.96875734969026084, 3.316774720514426456, -0.08597719988137648983 ) ) ;
#2573 = CARTESIAN_POINT ( 'NONE',  ( -66.55620429048340725, -23.47596703998600276, 11.44779298504227505 ) ) ;
#2574 = CARTESIAN_POINT ( 'NONE',  ( -24.57525087998973845, 6.376774720514426953, -15.45548830044933197 ) ) ;
#2575 = CARTESIAN_POINT ( 'NONE',  ( -67.52287095715006160, -24.66019654487199730, 8.947790411086115725 ) ) ;
#2576 = CARTESIAN_POINT ( 'NONE',  ( -21.83012794225054165, -5.757306806698124113, -1.500000000000002220 ) ) ;
#2577 = B_SPLINE_CURVE_WITH_KNOTS ( 'NONE', 3,
 ( #12877, #52460, #36236, #83393 ),
 .UNSPECIFIED., .F., .F.,
 ( 4, 4 ),
 ( 6.699507672488401150E-09, 0.001652437988939160470 ),
 .UNSPECIFIED. ) ;
#2578 = EDGE_CURVE ( 'NONE', #39283, #69177, #20310, .T. ) ;
#2579 = CARTESIAN_POINT ( 'NONE',  ( -3.108974358974359475, -6.376774720514417183, 20.36458333333334281 ) ) ;
#2580 = ORIENTED_EDGE ( 'NONE', *, *, #22477, .F. ) ;
#2581 = VECTOR ( 'NONE', #13758, 1000.000000000000000 ) ;
#2583 = CARTESIAN_POINT ( 'NONE',  ( 9.069233782100962316, 3.316774720514428232, -28.07145878873749112 ) ) ;
#2582 = B_SPLINE_CURVE_WITH_KNOTS ( 'NONE', 3,
 ( #68242, #53026, #81970, #67254, #99171, #22044, #90572, #43908, #90081, #21051, #13441, #75837, #52022, #73858, #91563, #83956, #20556, #51525, #44415 ),
 .UNSPECIFIED., .F., .F.,
 ( 4, 1, 1, 1, 1, 1, 1, 1, 1, 1, 1, 1, 1, 1, 1, 1, 4 ),
 ( 0.000000000000000000, 0.08252970382206505084, 0.1587788549175693509, 0.2277380621151788020, 0.2899456527966750574, 0.3454988386981356352, 0.3938963373401225820, 0.4363737851900879039, 0.4721222744615228839, 0.5363836155048278265, 0.5990779017254967975, 0.6619482340244574603, 0.7263105423531552862, 0.7917711030502098124, 0.8586473037978579192, 0.9273053338076842067, 1.000000000000000000 ),
 .UNSPECIFIED. ) ;
#2584 = CARTESIAN_POINT ( 'NONE',  ( -31.58666371736434186, -24.35071581493542325, 9.817618358456039473 ) ) ;
#2585 = CARTESIAN_POINT ( 'NONE',  ( 19.63295818312489871, -1.572306604260808260, 11.49999999999999645 ) ) ;
#2586 = CARTESIAN_POINT ( 'NONE',  ( 33.74607884027702909, -5.965225279485572685, -4.999864028243830916 ) ) ;
#2587 = VECTOR ( 'NONE', #42779, 1000.000000000000000 ) ;
#2588 = CARTESIAN_POINT ( 'NONE',  ( -73.52287095715007581, -23.47596703998600631, 11.44779298504228748 ) ) ;
#2589 = VERTEX_POINT ( 'NONE', #97933 ) ;
#2590 = AXIS2_PLACEMENT_3D ( 'NONE', #85676, #61855, #15658 ) ;
#2591 = CARTESIAN_POINT ( 'NONE',  ( -99.62531270275181328, -24.51314013834316796, 0.6176544820404258340 ) ) ;
#2592 = CARTESIAN_POINT ( 'NONE',  ( -8.160000000000000142, -9.652339641703484574, -1.203735189656879756 ) ) ;
#2594 = EDGE_CURVE ( 'NONE', #78412, #30953, #82222, .T. ) ;
#2593 = CARTESIAN_POINT ( 'NONE',  ( -124.5222546785644511, -23.48786465467241769, 11.44779295918253581 ) ) ;
#2595 = EDGE_CURVE ( 'NONE', #47215, #35163, #75104, .T. ) ;
#2596 = DIRECTION ( 'NONE',  ( 0.000000000000000000, -0.9999999999976377785, -2.173523156925979975E-06 ) ) ;
#2598 = LINE ( 'NONE', #84931, #49603 ) ;
#2597 = AXIS2_PLACEMENT_3D ( 'NONE', #78234, #54420, #32073 ) ;
#2599 = EDGE_CURVE ( 'NONE', #35613, #51748, #90837, .T. ) ;
#2600 = CARTESIAN_POINT ( 'NONE',  ( -5.265981236333618470E-16, -2.056774720514426669, -4.299999999999999822 ) ) ;
#2601 = CARTESIAN_POINT ( 'NONE',  ( -17.60924879254659459, 8.996216891746938060, -1.500000000000002220 ) ) ;
#2602 = ORIENTED_EDGE ( 'NONE', *, *, #36144, .T. ) ;
#2603 = EDGE_CURVE ( 'NONE', #32855, #62667, #29932, .T. ) ;
#2604 = CARTESIAN_POINT ( 'NONE',  ( 6.697674113365701842, 19.09646837838083400, 11.49999999999999645 ) ) ;
#2605 = CARTESIAN_POINT ( 'NONE',  ( -7.243541020599075786, -5.876774720514409189, 19.27798293355755632 ) ) ;
#2606 = EDGE_LOOP ( 'NONE', ( #52711, #5403, #87763, #39318 ) ) ;
#2607 = DIRECTION ( 'NONE',  ( -1.000000000000000000, 0.000000000000000000, -0.000000000000000000 ) ) ;
#2608 = DIRECTION ( 'NONE',  ( -1.000000000000000000, -1.232047923278981953E-16, 0.000000000000000000 ) ) ;
#2609 = CARTESIAN_POINT ( 'NONE',  ( -51.26639007284612148, -25.29356494163747371, 5.550358426643942522 ) ) ;
#2610 = CARTESIAN_POINT ( 'NONE',  ( 29.77147767949874435, -4.540774720514427543, 26.15915692125050995 ) ) ;
#2611 = DIRECTION ( 'NONE',  ( -1.334402673828313586E-16, 0.000000000000000000, 1.000000000000000000 ) ) ;
#2612 = CARTESIAN_POINT ( 'NONE',  ( -32.38277616518237778, -25.11010177982458913, 2.831122766525575596 ) ) ;
#2613 = CARTESIAN_POINT ( 'NONE',  ( -18.22994410263883225, 8.285605901428201747, -1.500000000000002220 ) ) ;
#2614 = EDGE_CURVE ( 'NONE', #11989, #72199, #99047, .T. ) ;
#2615 = CARTESIAN_POINT ( 'NONE',  ( 13.91401389203221406, 6.475225279485573360, 27.75920385068456042 ) ) ;
#2616 = VERTEX_POINT ( 'NONE', #19813 ) ;
#2617 = EDGE_CURVE ( 'NONE', #12137, #30127, #97453, .T. ) ;
#2618 = CARTESIAN_POINT ( 'NONE',  ( -51.52287095715006160, -24.34917612406836795, 0.1852690917426518535 ) ) ;
#2619 = DIRECTION ( 'NONE',  ( 0.000000000000000000, -0.9999999999976377785, -2.173523156925979975E-06 ) ) ;
#2620 = CARTESIAN_POINT ( 'NONE',  ( -41.32836283488544638, -4.132774720514426292, 39.26872235229541985 ) ) ;
#2621 = LINE ( 'NONE', #16827, #78805 ) ;
#2622 = CARTESIAN_POINT ( 'NONE',  ( -101.6533370195574690, -25.22562951682090215, 3.608687682288769238 ) ) ;
#2623 = ADVANCED_FACE ( 'NONE', ( #90337 ), #81730, .F. ) ;
#2624 = CARTESIAN_POINT ( 'NONE',  ( 14.62889129739865446, 4.326482771706361419, -28.09837290214758099 ) ) ;
#2625 = CARTESIAN_POINT ( 'NONE',  ( -101.9685402542758510, -25.30060005375480614, 6.009289253917324380 ) ) ;
#2626 = ORIENTED_EDGE ( 'NONE', *, *, #36952, .F. ) ;
#2627 = CARTESIAN_POINT ( 'NONE',  ( 11.02309159617336221, -17.05227643984133934, -1.500000000000002220 ) ) ;
#2628 = ORIENTED_EDGE ( 'NONE', *, *, #60832, .T. ) ;
#2629 = CARTESIAN_POINT ( 'NONE',  ( 31.62551770808318707, 4.240436435409185911, 26.92952082091879973 ) ) ;
#2630 = CARTESIAN_POINT ( 'NONE',  ( -122.5228709571501042, -23.73907113216990439, -1.053371485793246132 ) ) ;
#2631 = ORIENTED_EDGE ( 'NONE', *, *, #37859, .T. ) ;
#2632 = CARTESIAN_POINT ( 'NONE',  ( -59.50896880679595569, -23.96169478059712787, 10.65365249895718769 ) ) ;
#2633 = VECTOR ( 'NONE', #87073, 1000.000000000000000 ) ;
#2634 = EDGE_CURVE ( 'NONE', #51264, #20042, #44675, .T. ) ;
#2635 = CARTESIAN_POINT ( 'NONE',  ( 31.20850673110457763, -5.144960210277549351, -4.610511713824573476 ) ) ;
#2636 = CARTESIAN_POINT ( 'NONE',  ( -99.62287095715005592, -29.50248528299804818, 1.056150453629042030 ) ) ;
#2637 = CARTESIAN_POINT ( 'NONE',  ( -16.97324839047195866, 12.58421825509937442, 11.49999999999999645 ) ) ;
#2638 = CARTESIAN_POINT ( 'NONE',  ( -9.153499762860807465, 20.15527781828815534, 11.49999999999998934 ) ) ;
#2639 = EDGE_CURVE ( 'NONE', #66840, #909, #75594, .T. ) ;
#2640 = CARTESIAN_POINT ( 'NONE',  ( -17.20787902393383462, -11.26661214947554157, -1.500000000000002220 ) ) ;
#2641 = VECTOR ( 'NONE', #96333, 1000.000000000000114 ) ;
#2642 = ORIENTED_EDGE ( 'NONE', *, *, #30266, .T. ) ;
#2643 = CARTESIAN_POINT ( 'NONE',  ( -94.52287095715010423, -24.35013146730204170, 9.818937971375104823 ) ) ;
#2644 = ORIENTED_EDGE ( 'NONE', *, *, #50963, .F. ) ;
#2645 = CARTESIAN_POINT ( 'NONE',  ( -113.6228709571500559, -29.50250786944525672, 11.44777988621622988 ) ) ;
#2646 = CARTESIAN_POINT ( 'NONE',  ( -85.62287095715005592, -23.48786465467241413, 11.44779295918254114 ) ) ;
#2647 = ORIENTED_EDGE ( 'NONE', *, *, #45047, .T. ) ;
#2648 = AXIS2_PLACEMENT_3D ( 'NONE', #42589, #12617, #73035 ) ;
#2649 = VERTEX_POINT ( 'NONE', #12703 ) ;
#2650 = AXIS2_PLACEMENT_3D ( 'NONE', #4041, #97864, #74538 ) ;
#2651 = ORIENTED_EDGE ( 'NONE', *, *, #8768, .F. ) ;
#2652 = CARTESIAN_POINT ( 'NONE',  ( -64.62287095715005592, -29.50250786944525672, 11.44777988621623876 ) ) ;
#2653 = CARTESIAN_POINT ( 'NONE',  ( -110.6228709571500559, -29.50250786944525672, 11.44777988621622988 ) ) ;
#2654 = CARTESIAN_POINT ( 'NONE',  ( 6.365284455128204399, -6.376774720514413630, 19.73076923076922640 ) ) ;
#2655 = CARTESIAN_POINT ( 'NONE',  ( -14.15296684469643118, 15.14645709676483420, -1.500000000000002220 ) ) ;
#2656 = VECTOR ( 'NONE', #76179, 1000.000000000000114 ) ;
#2657 = CARTESIAN_POINT ( 'NONE',  ( -21.58526226860004371, 1.989002153404973328, 11.49999999999999645 ) ) ;
#2658 = ORIENTED_EDGE ( 'NONE', *, *, #34891, .T. ) ;
#2659 = CARTESIAN_POINT ( 'NONE',  ( -69.75867330073758410, -25.13524716939983961, 2.913775892772168419 ) ) ;
#2660 = DIRECTION ( 'NONE',  ( -3.773278334453079030E-23, 0.9999999999976377785, 2.173523156925979128E-06 ) ) ;
#2661 = CARTESIAN_POINT ( 'NONE',  ( -4.914914792326205983, -21.87198836336805385, 11.49999999999998934 ) ) ;
#2662 = AXIS2_PLACEMENT_3D ( 'NONE', #78837, #17963, #33690 ) ;
#2663 = DIRECTION ( 'NONE',  ( -7.719682517540865740E-16, -0.4450093991605197363, 0.8955258983741304357 ) ) ;
#2664 = CARTESIAN_POINT ( 'NONE',  ( -57.92287095715004597, -23.47596703998600276, 11.44779298504227860 ) ) ;
#2665 = ORIENTED_EDGE ( 'NONE', *, *, #85089, .F. ) ;
#2666 = DIRECTION ( 'NONE',  ( -0.000000000000000000, 1.000000000000000000, -0.000000000000000000 ) ) ;
#2667 = CARTESIAN_POINT ( 'NONE',  ( 12.17309066428871667, -5.143895418987112222, -26.49515656621686333 ) ) ;
#2668 = ORIENTED_EDGE ( 'NONE', *, *, #87344, .F. ) ;
#2669 = EDGE_LOOP ( 'NONE', ( #16007, #37598, #18262, #85035 ) ) ;
#2670 = CARTESIAN_POINT ( 'NONE',  ( -46.53036571332072668, -24.66019654487199375, 8.947790411086122830 ) ) ;
#2671 = VERTEX_POINT ( 'NONE', #74606 ) ;
#2672 = CARTESIAN_POINT ( 'NONE',  ( 26.74698519091204574, 1.682774720514426114, -10.98683230472873973 ) ) ;
#2673 = CARTESIAN_POINT ( 'NONE',  ( 15.87343765641381665, 14.11872912734625274, -1.500000000000002220 ) ) ;
#2674 = ORIENTED_EDGE ( 'NONE', *, *, #27192, .F. ) ;
#2675 = CARTESIAN_POINT ( 'NONE',  ( -68.62287095715004170, -23.73907113216991860, -1.053371485793230367 ) ) ;
#2676 = CARTESIAN_POINT ( 'NONE',  ( 15.22768361601695020, -15.61070304372801587, -1.500000000000002220 ) ) ;
#2677 = FACE_OUTER_BOUND ( 'NONE', #26501, .T. ) ;
#2678 = CARTESIAN_POINT ( 'NONE',  ( -107.5228709571500332, -23.94994826722564696, -0.6494450866342712514 ) ) ;
#2679 = CARTESIAN_POINT ( 'NONE',  ( 5.873458226074941280, -5.876774720514414518, 19.84669099281175164 ) ) ;
#2680 = CARTESIAN_POINT ( 'NONE',  ( -20.57654891367511851, 7.437132321665034240, -1.500000000000002220 ) ) ;
#2681 = CARTESIAN_POINT ( 'NONE',  ( 7.153659783701941777, -5.876774720514421624, 20.92502190304499265 ) ) ;
#2682 = ORIENTED_EDGE ( 'NONE', *, *, #73080, .F. ) ;
#2683 = CARTESIAN_POINT ( 'NONE',  ( -108.8968792378191921, -29.50249917535260380, 7.447779886225679213 ) ) ;
#2684 = CARTESIAN_POINT ( 'NONE',  ( -48.87675733776060838, -25.26337330288447092, 6.266175371071904365 ) ) ;
#2685 = VECTOR ( 'NONE', #61208, 1000.000000000000114 ) ;
#2686 = ORIENTED_EDGE ( 'NONE', *, *, #6352, .T. ) ;
#2687 = DIRECTION ( 'NONE',  ( 0.000000000000000000, -1.000000000000000000, 0.000000000000000000 ) ) ;
#2688 = ORIENTED_EDGE ( 'NONE', *, *, #100417, .T. ) ;
#2689 = CARTESIAN_POINT ( 'NONE',  ( 30.53060340732036693, -4.132774720514426292, -2.322449884495168870 ) ) ;
#2690 = LINE ( 'NONE', #47355, #98347 ) ;
#2691 = CARTESIAN_POINT ( 'NONE',  ( 21.23515499356076930, 0.7789969333488580006, 11.49999999999998934 ) ) ;
#2692 = DIRECTION ( 'NONE',  ( 0.000000000000000000, -1.000000000000000000, 0.000000000000000000 ) ) ;
#2693 = LINE ( 'NONE', #86912, #91648 ) ;
#2694 = DIRECTION ( 'NONE',  ( -1.000000000000000000, -3.773278334444167608E-23, -8.201307833595939069E-29 ) ) ;
#2696 = CARTESIAN_POINT ( 'NONE',  ( -68.63109341914197614, -24.34968618360933590, 0.1864209137778813363 ) ) ;
#2695 = B_SPLINE_CURVE_WITH_KNOTS ( 'NONE', 3,
 ( #97751, #82032, #88655, #89644 ),
 .UNSPECIFIED., .F., .F.,
 ( 4, 4 ),
 ( 1.387778780781445521E-17, 9.999999999996123101E-05 ),
 .UNSPECIFIED. ) ;
#2697 = CARTESIAN_POINT ( 'NONE',  ( -18.68671320864135765, 5.291888989699490509, 11.49999999999998934 ) ) ;
#2698 = CARTESIAN_POINT ( 'NONE',  ( -45.57565279233343603, -24.92564183028979130, 1.928384488918256645 ) ) ;
#2699 = ORIENTED_EDGE ( 'NONE', *, *, #83686, .F. ) ;
#2700 = EDGE_CURVE ( 'NONE', #3925, #53709, #36051, .T. ) ;
#2701 = CARTESIAN_POINT ( 'NONE',  ( -18.49313839071750820, -6.238557295281221826, 11.49999999999999645 ) ) ;
#2702 = CARTESIAN_POINT ( 'NONE',  ( -5.063563723219555612, -6.376774720514408301, 19.46509473978807847 ) ) ;
#2703 = EDGE_CURVE ( 'NONE', #39193, #923, #57935, .T. ) ;
#2704 = CARTESIAN_POINT ( 'NONE',  ( 13.91401389203221406, -3.316774720514426456, 27.24920385068457662 ) ) ;
#2705 = EDGE_LOOP ( 'NONE', ( #68137, #77377, #63466, #71904 ) ) ;
#2706 = EDGE_CURVE ( 'NONE', #20861, #52175, #91331, .T. ) ;
#2707 = DIRECTION ( 'NONE',  ( -3.469446951953615372E-15, 1.000000000000000000, 0.000000000000000000 ) ) ;
#2708 = CARTESIAN_POINT ( 'NONE',  ( -89.63160522007152053, -24.15543982623907482, -0.2315651400026483009 ) ) ;
#2709 = EDGE_CURVE ( 'NONE', #59212, #24964, #56680, .T. ) ;
#2710 = AXIS2_PLACEMENT_3D ( 'NONE', #94424, #63505, #26429 ) ;
#2711 = DIRECTION ( 'NONE',  ( 0.000000000000000000, -1.000000000000000000, 0.000000000000000000 ) ) ;
#2712 = CARTESIAN_POINT ( 'NONE',  ( -81.01753736565918018, -25.24813972518663618, 7.476685482214374900 ) ) ;
#2713 = CARTESIAN_POINT ( 'NONE',  ( -2.223759785643201869, -19.53228827767608777, -1.500000000000002220 ) ) ;
#2714 = ORIENTED_EDGE ( 'NONE', *, *, #46349, .T. ) ;
#2715 = CARTESIAN_POINT ( 'NONE',  ( -7.160000000000000142, -10.77121780415746599, 1.154761385154455366 ) ) ;
#2716 = CARTESIAN_POINT ( 'NONE',  ( -43.55620429048339304, -24.64898659630528854, 1.056161002820822592 ) ) ;
#2717 = AXIS2_PLACEMENT_3D ( 'NONE', #61487, #45256, #8190 ) ;
#2719 = ADVANCED_FACE ( 'NONE', ( #86225 ), #77335, .T. ) ;
#2718 = PERSON_AND_ORGANIZATION_ROLE ( 'design_owner' ) ;
#2720 = CARTESIAN_POINT ( 'NONE',  ( 3.045412351277957175, -5.876774720514421624, 20.90433128744512814 ) ) ;
#2721 = CARTESIAN_POINT ( 'NONE',  ( 33.74607884027702909, 5.965225279485572685, -4.999864028243830916 ) ) ;
#2722 = CARTESIAN_POINT ( 'NONE',  ( -5.366453405989236813, 0.000000000000000000, 0.000000000000000000 ) ) ;
#2723 = CARTESIAN_POINT ( 'NONE',  ( -97.54592273218207765, -24.66019654487199730, 8.947790411086115725 ) ) ;
#2724 = LINE ( 'NONE', #33664, #12843 ) ;
#2725 = TOROIDAL_SURFACE ( 'NONE', #99955, 253.2618649670780826, 0.8159999999999999476 ) ;
#2726 = AXIS2_PLACEMENT_3D ( 'NONE', #91133, #66831, #75400 ) ;
#2727 = CARTESIAN_POINT ( 'NONE',  ( -69.36083545395123906, -25.31201746261485752, 6.029876604266336315 ) ) ;
#2728 = CARTESIAN_POINT ( 'NONE',  ( 25.61870917940689196, -5.965225279485572685, 29.49402280011862487 ) ) ;
#2729 = CARTESIAN_POINT ( 'NONE',  ( -12.53609265798794681, -15.47265773855268378, -1.500000000000002220 ) ) ;
#2730 = B_SPLINE_CURVE_WITH_KNOTS ( 'NONE', 3,
 ( #18879, #95510, #66592, #96505, #25497, #11766, #81284, #42253, #80285, #10779 ),
 .UNSPECIFIED., .F., .F.,
 ( 4, 2, 2, 2, 4 ),
 ( 0.000000000000000000, 0.0002024578457012554070, 0.0004049156914025108141, 0.0006073735371037662211, 0.0008098313828050216281 ),
 .UNSPECIFIED. ) ;
#2731 = CARTESIAN_POINT ( 'NONE',  ( -75.62528596432828465, -24.92592662359561473, 8.075495903018000021 ) ) ;
#2732 = CARTESIAN_POINT ( 'NONE',  ( -16.51628311069853083, -11.03946451426814690, -1.500000000000002220 ) ) ;
#2733 = ORIENTED_EDGE ( 'NONE', *, *, #11745, .T. ) ;
#2734 = VECTOR ( 'NONE', #94311, 1000.000000000000000 ) ;
#2735 = CARTESIAN_POINT ( 'NONE',  ( -120.5895376238167103, -23.48783264082479505, -1.443836473390058384 ) ) ;
#2736 = DIRECTION ( 'NONE',  ( -1.000000000000000000, -3.773278334444166432E-23, -8.201307841325785021E-29 ) ) ;
#2737 = CARTESIAN_POINT ( 'NONE',  ( 0.06697178475903577122, -6.376774720514410077, 19.29815762497054976 ) ) ;
#2738 = CARTESIAN_POINT ( 'NONE',  ( 8.817327481837082814, -3.316774720514257702, -28.08864864913269699 ) ) ;
#2739 = CARTESIAN_POINT ( 'NONE',  ( 20.50115541507891948, 3.495740877612329101, 11.49999999999999645 ) ) ;
#2740 = CARTESIAN_POINT ( 'NONE',  ( -38.22287095715005734, -23.47593901973090169, -1.443836447538997980 ) ) ;
#2741 = CARTESIAN_POINT ( 'NONE',  ( -62.52287095715006160, -23.47596703998600631, 11.44779298504228926 ) ) ;
#2742 = CARTESIAN_POINT ( 'NONE',  ( -12.33899560737860313, 19.21699747222852395, 11.49999999999999645 ) ) ;
#2743 = EDGE_LOOP ( 'NONE', ( #38964, #69432, #64951, #10772 ) ) ;
#2744 = DIRECTION ( 'NONE',  ( -0.000000000000000000, 2.173523156925979552E-06, -0.9999999999976378895 ) ) ;
#2745 = CYLINDRICAL_SURFACE ( 'NONE', #14415, 6.000000000000000888 ) ;
#2746 = ORIENTED_EDGE ( 'NONE', *, *, #35016, .T. ) ;
#2747 = CARTESIAN_POINT ( 'NONE',  ( -10.81679630089563915, -17.07601267366916886, 11.49999999999998934 ) ) ;
#2748 = CARTESIAN_POINT ( 'NONE',  ( 7.478911390063968767, -6.376774720514422512, 20.82112274756839199 ) ) ;
#2749 = LINE ( 'NONE', #70247, #83620 ) ;
#2750 = AXIS2_PLACEMENT_3D ( 'NONE', #100199, #60191, #53579 ) ;
#2751 = CARTESIAN_POINT ( 'NONE',  ( -100.6228709571499991, -24.15431212366392089, -0.2830839119429089390 ) ) ;
#2753 = EDGE_LOOP ( 'NONE', ( #12243, #42485, #15967, #43095 ) ) ;
#2752 = EDGE_CURVE ( 'NONE', #79650, #40077, #54791, .T. ) ;
#2754 = CARTESIAN_POINT ( 'NONE',  ( -70.62287095715005592, -24.99156045073392463, 7.747789690856161648 ) ) ;
#2755 = CARTESIAN_POINT ( 'NONE',  ( -100.6228709571500559, -23.47593901973091235, -1.443836447539001089 ) ) ;
#2756 = CARTESIAN_POINT ( 'NONE',  ( -8.782848147209532996, 18.00178819457707746, -1.500000000000002220 ) ) ;
#2757 = CARTESIAN_POINT ( 'NONE',  ( 11.42219733811748306, 17.55150860717643724, 11.49999999999999645 ) ) ;
#2758 = AXIS2_PLACEMENT_3D ( 'NONE', #96157, #87542, #94139 ) ;
#2759 = CARTESIAN_POINT ( 'NONE',  ( -27.70544111104076990, -24.65058036537550024, 8.251826706788236265 ) ) ;
#2760 = DIRECTION ( 'NONE',  ( -1.000000000000000000, 0.000000000000000000, 0.000000000000000000 ) ) ;
#2761 = CARTESIAN_POINT ( 'NONE',  ( 3.837975233861466329, 21.70421690940786874, 11.49999999999998934 ) ) ;
#2762 = EDGE_CURVE ( 'NONE', #98254, #92450, #32439, .T. ) ;
#2763 = CARTESIAN_POINT ( 'NONE',  ( -40.41683116089613748, -25.27806106706002964, 5.082404452749530677 ) ) ;
#2764 = ORIENTED_EDGE ( 'NONE', *, *, #68567, .F. ) ;
#2765 = B_SPLINE_CURVE_WITH_KNOTS ( 'NONE', 3,
 ( #70657, #76740, #78248, #7242, #61558, #92477, #15353, #15854, #46317, #46825, #8257, #8759, #39697, #39195, #70153, #638, #62551, #72169, #1653, #18865, #57455, #2163, #49338, #87885, #55946, #32589, #95494 ),
 .UNSPECIFIED., .F., .F.,
 ( 4, 1, 1, 1, 1, 1, 1, 1, 1, 1, 1, 1, 1, 1, 1, 1, 1, 1, 1, 1, 1, 1, 1, 1, 4 ),
 ( 0.000000000000000000, 0.03378811616271038681, 0.06719393237388025797, 0.09986241085682510954, 0.1325666121262582542, 0.1651511732547865374, 0.1979131873557924692, 0.2313190035669614730, 0.2650832782673732679, 0.2992553087581151794, 0.3343985665049788447, 0.3699428235093072392, 0.4062835607000603866, 0.4440638196985079444, 0.4829977068727749345, 0.5233544466133041029, 0.5655365896041484319, 0.6096129240658189063, 0.6563908113764170826, 0.7058854949364568032, 0.7583245002617304831, 0.8138317829411497728, 0.8727945590393887398, 0.9347222295400740011, 1.000000000000000000 ),
 .UNSPECIFIED. ) ;
#2766 = CARTESIAN_POINT ( 'NONE',  ( -60.52287095715006160, -23.47593901973090169, -1.443836447538996870 ) ) ;
#2767 = LINE ( 'NONE', #48939, #54171 ) ;
#2768 = CARTESIAN_POINT ( 'NONE',  ( -72.62691918628158305, -24.51314013834316796, 0.6176544820404145097 ) ) ;
#2769 = VERTEX_POINT ( 'NONE', #55295 ) ;
#2770 = CARTESIAN_POINT ( 'NONE',  ( 2.936453026386435017, -6.376774720514406525, 18.60215244312560401 ) ) ;
#2771 = B_SPLINE_CURVE_WITH_KNOTS ( 'NONE', 3,
 ( #23018, #85944, #92051, #30656 ),
 .UNSPECIFIED., .F., .F.,
 ( 4, 4 ),
 ( 0.9604717738612708056, 0.9694782051333865613 ),
 .UNSPECIFIED. ) ;
#2772 = ORIENTED_EDGE ( 'NONE', *, *, #50805, .F. ) ;
#2773 = ORIENTED_EDGE ( 'NONE', *, *, #100154, .F. ) ;
#2774 = CARTESIAN_POINT ( 'NONE',  ( -83.52287095715006160, -23.47596703998600631, 11.44779298504228571 ) ) ;
#2775 = DIRECTION ( 'NONE',  ( 0.000000000000000000, 0.000000000000000000, 1.000000000000000000 ) ) ;
#2776 = CARTESIAN_POINT ( 'NONE',  ( -58.62287095715004881, -23.48783264082478439, -1.443836473390069264 ) ) ;
#2777 = CARTESIAN_POINT ( 'NONE',  ( 18.81462172601333549, -8.267562025728075525, -1.500000000000002220 ) ) ;
#2778 = VERTEX_POINT ( 'NONE', #85726 ) ;
#2779 = CARTESIAN_POINT ( 'NONE',  ( -0.7395115731254252589, 18.09566585216508727, -9.000000000000000000 ) ) ;
#2780 = CARTESIAN_POINT ( 'NONE',  ( -23.71328795744024376, 0.3587747205144057872, -17.58350715675015863 ) ) ;
#2781 = DIRECTION ( 'NONE',  ( 4.472869286569333237E-16, 1.000000000000000000, -7.102795889480452575E-16 ) ) ;
#2782 = CARTESIAN_POINT ( 'NONE',  ( -6.278373996654322831, -21.41630973362384083, 11.49999999999998934 ) ) ;
#2783 = VECTOR ( 'NONE', #82547, 1000.000000000000000 ) ;
#2784 = CARTESIAN_POINT ( 'NONE',  ( -70.80335600588159650, -25.15073531561621323, 6.999027372372252920 ) ) ;
#2785 = DIRECTION ( 'NONE',  ( 0.000000000000000000, 0.000000000000000000, -1.000000000000000000 ) ) ;
#2786 = EDGE_LOOP ( 'NONE', ( #1665, #80195, #83007, #82612 ) ) ;
#2787 = PLANE ( 'NONE',  #64733 ) ;
#2788 = CARTESIAN_POINT ( 'NONE',  ( -6.660000000000001030, -11.08332949055823846, -0.7794760011071779626 ) ) ;
#2789 = CARTESIAN_POINT ( 'NONE',  ( 15.14581745102402088, -14.33592658440916523, 11.49999999999998934 ) ) ;
#2790 = VERTEX_POINT ( 'NONE', #30435 ) ;
#2791 = B_SPLINE_CURVE_WITH_KNOTS ( 'NONE', 3,
 ( #17247, #30473, #70036, #62435 ),
 .UNSPECIFIED., .F., .F.,
 ( 4, 4 ),
 ( 0.000000000000000000, 0.002134615384615401457 ),
 .UNSPECIFIED. ) ;
#2793 = ORIENTED_EDGE ( 'NONE', *, *, #34831, .F. ) ;
#2792 = DIRECTION ( 'NONE',  ( 5.238131417152343399E-15, 0.000000000000000000, 1.000000000000000000 ) ) ;
#2794 = AXIS2_PLACEMENT_3D ( 'NONE', #71261, #56049, #41826 ) ;
#2795 = ORIENTED_EDGE ( 'NONE', *, *, #7638, .F. ) ;
#2796 = CARTESIAN_POINT ( 'NONE',  ( -32.82969853631264101, -25.04397465799123168, 2.466842825816077944 ) ) ;
#2797 = CARTESIAN_POINT ( 'NONE',  ( -9.798014431990228701, 18.61115389415964572, -1.500000000000002220 ) ) ;
#2798 = VERTEX_POINT ( 'NONE', #15710 ) ;
#2799 = AXIS2_PLACEMENT_3D ( 'NONE', #12390, #35746, #66717 ) ;
#2800 = CARTESIAN_POINT ( 'NONE',  ( -114.5562042904833930, -23.48783264082478794, -1.443836473390060604 ) ) ;
#2801 = DIRECTION ( 'NONE',  ( -0.000000000000000000, 0.000000000000000000, -1.000000000000000000 ) ) ;
#2802 = CARTESIAN_POINT ( 'NONE',  ( -120.5186613917142182, -24.40133493613049964, 9.663955038902800609 ) ) ;
#2803 = VECTOR ( 'NONE', #82415, 1000.000000000000114 ) ;
#2804 = CARTESIAN_POINT ( 'NONE',  ( -86.58307941256070706, -24.66019654487200086, 8.947790411086115725 ) ) ;
#2805 = CARTESIAN_POINT ( 'NONE',  ( -49.52287095715006160, -24.64898659630367561, 1.056161002820821038 ) ) ;
#2806 = CARTESIAN_POINT ( 'NONE',  ( 12.82194709444435077, -17.51738216156474337, -1.500000000000002220 ) ) ;
#2807 = CARTESIAN_POINT ( 'NONE',  ( -57.52287095715007581, -24.51283580621365132, 0.6167428607019714848 ) ) ;
#2809 = ORIENTED_EDGE ( 'NONE', *, *, #79106, .T. ) ;
#2808 = CARTESIAN_POINT ( 'NONE',  ( 11.91227609878784399, -18.80521639033699799, 11.49999999999999645 ) ) ;
#2810 = CARTESIAN_POINT ( 'NONE',  ( -51.44586644541745812, -25.24728857774910296, 5.815367749938357811 ) ) ;
#2811 = CARTESIAN_POINT ( 'NONE',  ( 8.567893164715611576, -0.1262136116457373280, -3.707288619710387145 ) ) ;
#2812 = CARTESIAN_POINT ( 'NONE',  ( -79.11611000704996854, -29.50249039766296022, 3.409318347773680369 ) ) ;
#2813 = ORIENTED_EDGE ( 'NONE', *, *, #39610, .F. ) ;
#2815 = ORIENTED_EDGE ( 'NONE', *, *, #21069, .F. ) ;
#2814 = CARTESIAN_POINT ( 'NONE',  ( -13.89275734969026566, 5.965225279485572685, 30.51402280011862089 ) ) ;
#2816 = ORIENTED_EDGE ( 'NONE', *, *, #17500, .T. ) ;
#2817 = CARTESIAN_POINT ( 'NONE',  ( -122.6228709571500417, -29.50250243563736774, 8.947779886222134493 ) ) ;
#2818 = CARTESIAN_POINT ( 'NONE',  ( -35.52287095715006870, -24.99132157543083821, 2.256160258750667502 ) ) ;
#2819 = CARTESIAN_POINT ( 'NONE',  ( -29.49875734969026198, 0.3587747205144265483, 10.11402280011862587 ) ) ;
#2820 = VERTEX_POINT ( 'NONE', #92328 ) ;
#2821 = ADVANCED_FACE ( 'NONE', ( #47175 ), #31438, .T. ) ;
#2822 = CARTESIAN_POINT ( 'NONE',  ( -42.62287095715007013, -24.35013146730202394, 9.818937971375111928 ) ) ;
#2823 = CARTESIAN_POINT ( 'NONE',  ( 5.309366582633749054, -21.77581755331916824, -1.500000000000002220 ) ) ;
#2824 = ORIENTED_EDGE ( 'NONE', *, *, #97108, .T. ) ;
#2825 = ORIENTED_EDGE ( 'NONE', *, *, #90659, .F. ) ;
#2826 = CARTESIAN_POINT ( 'NONE',  ( -34.52287095715006870, -24.50321055353803956, 9.387540953477520489 ) ) ;
#2827 = DIRECTION ( 'NONE',  ( 0.000000000000000000, 0.000000000000000000, -1.000000000000000000 ) ) ;
#2828 = EDGE_CURVE ( 'NONE', #30682, #36801, #11912, .T. ) ;
#2829 = CARTESIAN_POINT ( 'NONE',  ( -39.44890538690540893, -25.29243216311327913, 4.249687596552191415 ) ) ;
#2830 = AXIS2_PLACEMENT_3D ( 'NONE', #92371, #93366, #24365 ) ;
#2831 = CARTESIAN_POINT ( 'NONE',  ( 31.13709916799238897, 5.945958180706680807, -1.190136329645604230 ) ) ;
#2832 = ADVANCED_FACE ( 'NONE', ( #31943 ), #62913, .T. ) ;
#2833 = CARTESIAN_POINT ( 'NONE',  ( -30.57951140250705180, -25.14081846633245831, 7.291654623549840508 ) ) ;
#2834 = CARTESIAN_POINT ( 'NONE',  ( -9.542874777335924819, 17.09510996321218101, 11.49999999999998934 ) ) ;
#2835 = B_SPLINE_SURFACE_WITH_KNOTS ( 'NONE', 3, 3, ( 
 ( #94244, #24727, #2414, #62826 ),
 ( #55208, #79523, #49592, #10012 ),
 ( #86137, #95751, #56209, #25742 ),
 ( #57215, #11017, #16613, #71931 ),
 ( #72429, #47591, #55710, #33343 ),
 ( #64335, #10510, #64841, #48090 ),
 ( #25232, #78508, #88148, #24235 ),
 ( #18618, #1414, #9012, #80525 ),
 ( #9513, #41985, #39963, #56712 ),
 ( #87137, #40472, #79015, #87646 ) ),
 .UNSPECIFIED., .F., .F., .F.,
 ( 4, 3, 3, 4 ),
 ( 4, 4 ),
 ( 0.0004766839783845154836, 0.1491231665100183901, 0.2234464077758353262, 0.2977696490416522623 ),
 ( 0.04949997504963826039, 0.05054219714328903046 ),
 .UNSPECIFIED. ) ;
#2836 = EDGE_CURVE ( 'NONE', #86491, #14136, #76058, .T. ) ;
#2837 = CYLINDRICAL_SURFACE ( 'NONE', #8587, 22.69500000000000384 ) ;
#2838 = ORIENTED_EDGE ( 'NONE', *, *, #39555, .T. ) ;
#2839 = CARTESIAN_POINT ( 'NONE',  ( -2.508422780830330989, 21.39056295969660582, 11.49999999999998934 ) ) ;
#2840 = CIRCLE ( 'NONE', #62823, 129.7684398600581233 ) ;
#2841 = CARTESIAN_POINT ( 'NONE',  ( -75.52287095715004739, -25.00182538069145366, 7.747789668545101094 ) ) ;
#2842 = ADVANCED_FACE ( 'NONE', ( #2497 ), #93560, .T. ) ;
#2843 = DIRECTION ( 'NONE',  ( -1.000000000000000000, -0.000000000000000000, -0.000000000000000000 ) ) ;
#2844 = CARTESIAN_POINT ( 'NONE',  ( -101.6526051508143382, -25.23550958530647748, 3.607042638994091277 ) ) ;
#2845 = CARTESIAN_POINT ( 'NONE',  ( -77.62287095715004170, -23.96177878511308634, 10.65340807706329862 ) ) ;
#2846 = CARTESIAN_POINT ( 'NONE',  ( 14.22603995551189371, 18.00578905361294346, -1.500000000000002220 ) ) ;
#2847 = APPLICATION_PROTOCOL_DEFINITION ( 'international standard', 'config_control_design', 1994, #7717 ) ;
#2848 = CARTESIAN_POINT ( 'NONE',  ( -84.92287095715008149, -23.47596703998600631, 11.44779298504227860 ) ) ;
#2849 = CARTESIAN_POINT ( 'NONE',  ( -49.64567008890409028, -23.96119346886879953, -0.6495511937832114668 ) ) ;
#2850 = CARTESIAN_POINT ( 'NONE',  ( -2.827821146493835425, 19.88259668395040691, 11.49999999999999645 ) ) ;
#2851 = LINE ( 'NONE', #73843, #98071 ) ;
#2852 = CARTESIAN_POINT ( 'NONE',  ( 282.9764569301858046, 0.3587747205144265483, 20.79159422840526616 ) ) ;
#2853 = PRODUCT ( 'Hook_Varsay\X2\0131\X0\lan', 'Hook_Varsay\X2\0131\X0\lan', '', ( #90556 ) ) ;
#2854 = CARTESIAN_POINT ( 'NONE',  ( -82.62287095715005592, -24.65952944569304606, 1.056160979905699016 ) ) ;
#2855 = CARTESIAN_POINT ( 'NONE',  ( 12.88745205056431864, 5.152774720521900775, -28.14312002385407041 ) ) ;
#2856 = EDGE_CURVE ( 'NONE', #64065, #73483, #94208, .T. ) ;
#2857 = CARTESIAN_POINT ( 'NONE',  ( -126.5228709571500616, -23.48786465467241769, 11.44779295918253581 ) ) ;
#2858 = CARTESIAN_POINT ( 'NONE',  ( 16.83370257367741019, -10.51912618480096206, -1.500000000000002220 ) ) ;
#2859 = PLANE ( 'NONE',  #64221 ) ;
#2860 = CARTESIAN_POINT ( 'NONE',  ( 17.62393913918218402, -8.800128315780904487, -1.500000000000002220 ) ) ;
#2861 = AXIS2_PLACEMENT_3D ( 'NONE', #89804, #67472, #21272 ) ;
#2862 = CARTESIAN_POINT ( 'NONE',  ( 15.14080536460163984, -5.152774720514426754, -26.62908960815042292 ) ) ;
#2863 = CARTESIAN_POINT ( 'NONE',  ( 32.50838937279093699, -2.682774720514426559, -10.74666623472941573 ) ) ;
#2864 = SECURITY_CLASSIFICATION_LEVEL ( 'unclassified' ) ;
#2865 = CARTESIAN_POINT ( 'NONE',  ( -60.52287095715006160, -23.47596703998600631, 11.44779298504228926 ) ) ;
#2866 = CARTESIAN_POINT ( 'NONE',  ( -39.04496629636555127, -25.28398045664843252, 4.275496105309666284 ) ) ;
#2867 = CARTESIAN_POINT ( 'NONE',  ( 20.50092990308456464, -2.467789585553555654, 11.49999999999999645 ) ) ;
#2868 = CARTESIAN_POINT ( 'NONE',  ( 4.281508569253434260, -6.376774720514422512, 21.28700241941785265 ) ) ;
#2869 = VECTOR ( 'NONE', #84348, 1000.000000000000114 ) ;
#2870 = CARTESIAN_POINT ( 'NONE',  ( -128.5228709571500758, -23.48786465467242479, 11.44779295918253581 ) ) ;
#2871 = CARTESIAN_POINT ( 'NONE',  ( -20.69567741759225399, -9.018594580484563750, 11.49999999999999645 ) ) ;
#2872 = VERTEX_POINT ( 'NONE', #18214 ) ;
#2873 = CARTESIAN_POINT ( 'NONE',  ( -69.56233234027952506, -25.12219073830083005, 6.775360582497007123 ) ) ;
#2874 = CARTESIAN_POINT ( 'NONE',  ( -51.28856610397944849, -25.28231816955815603, 4.101867242166210126 ) ) ;
#2875 = CARTESIAN_POINT ( 'NONE',  ( -64.52287095715004739, -24.34917612406836795, 0.1852690917426522976 ) ) ;
#2876 = VECTOR ( 'NONE', #19769, 1000.000000000000114 ) ;
#2877 = EDGE_CURVE ( 'NONE', #85731, #78408, #82252, .T. ) ;
#2878 = DIRECTION ( 'NONE',  ( -0.000000000000000000, 1.000000000000000000, -0.000000000000000000 ) ) ;
#2879 = CARTESIAN_POINT ( 'NONE',  ( -2.780940648273603433, -6.376774720514413630, 20.02088365235843881 ) ) ;
#2880 = EDGE_CURVE ( 'NONE', #91650, #19525, #69954, .T. ) ;
#2881 = ORIENTED_EDGE ( 'NONE', *, *, #37206, .F. ) ;
#2882 = CARTESIAN_POINT ( 'NONE',  ( 21.72910700495702230, 7.846448622349001312, 11.49999999999999645 ) ) ;
#2883 = CARTESIAN_POINT ( 'NONE',  ( 2.723195454624489642, 22.67993996152103620, 11.49999999999998934 ) ) ;
#2884 = FACE_OUTER_BOUND ( 'NONE', #28070, .T. ) ;
#2885 = CARTESIAN_POINT ( 'NONE',  ( -106.6228709571501270, -23.96177878511308634, 10.65340807706329507 ) ) ;
#2886 = CARTESIAN_POINT ( 'NONE',  ( -63.64183645978062032, -23.96169478059713143, 10.65365249895718236 ) ) ;
#2887 = CARTESIAN_POINT ( 'NONE',  ( 16.76845895467136671, -15.01613412638008782, 11.49999999999999645 ) ) ;
#2888 = ORIENTED_EDGE ( 'NONE', *, *, #17378, .T. ) ;
#2889 = CARTESIAN_POINT ( 'NONE',  ( -43.53993766296616030, -24.34968618360933235, 0.1864209137778850833 ) ) ;
#2890 = CARTESIAN_POINT ( 'NONE',  ( -21.79611004543898289, 2.820803583321412678, 11.49999999999998934 ) ) ;
#2891 = CARTESIAN_POINT ( 'NONE',  ( 31.90158556755667973, 4.901725665521331265, -4.230180255418043878 ) ) ;
#2892 = CARTESIAN_POINT ( 'NONE',  ( -111.5588656375797427, -23.48783264082477018, -1.443836473390086805 ) ) ;
#2893 = CARTESIAN_POINT ( 'NONE',  ( -29.24573430514233507, -25.21724468935045138, 5.187748752069927249 ) ) ;
#2894 = ORIENTED_EDGE ( 'NONE', *, *, #63272, .T. ) ;
#2895 = CARTESIAN_POINT ( 'NONE',  ( -48.54083561204919306, -24.35071581493543036, 9.817618358456027039 ) ) ;
#2896 = EDGE_CURVE ( 'NONE', #60171, #62319, #6300, .T. ) ;
#2897 = CARTESIAN_POINT ( 'NONE',  ( -0.005606649364735081555, -5.876774720514410077, 19.25713806424188235 ) ) ;
#2898 = ORIENTED_EDGE ( 'NONE', *, *, #5944, .F. ) ;
#2899 = CARTESIAN_POINT ( 'NONE',  ( -68.92287095715006728, -23.47596703998600631, 11.44779298504227683 ) ) ;
#2900 = CARTESIAN_POINT ( 'NONE',  ( -1.317410511717131971, -20.46822056820986546, 11.49999999999998934 ) ) ;
#2901 = ORIENTED_EDGE ( 'NONE', *, *, #47493, .T. ) ;
#2902 = ORIENTED_EDGE ( 'NONE', *, *, #23112, .F. ) ;
#2903 = EDGE_LOOP ( 'NONE', ( #54698, #71332, #28234, #8202, #30585, #82277, #21813, #24449, #14643 ) ) ;
#2904 = CARTESIAN_POINT ( 'NONE',  ( -81.45489302840726964, -25.23432015487805558, 6.407480964600187789 ) ) ;
#2905 = CARTESIAN_POINT ( 'NONE',  ( 19.36532470938277228, 12.59445105952145738, 11.49999999999998934 ) ) ;
#2906 = CARTESIAN_POINT ( 'NONE',  ( 14.43441819135929194, 3.316774720514426456, -28.36222020317710957 ) ) ;
#2907 = CARTESIAN_POINT ( 'NONE',  ( 5.487062353440709472, 19.58251264919930534, -1.500000000000002220 ) ) ;
#2908 = EDGE_CURVE ( 'NONE', #98373, #33368, #74003, .T. ) ;
#2909 = ORIENTED_EDGE ( 'NONE', *, *, #47982, .F. ) ;
#2910 = VECTOR ( 'NONE', #29364, 1000.000000000000000 ) ;
#2911 = CARTESIAN_POINT ( 'NONE',  ( -87.62287095715004170, -23.48783264082478794, -1.443836473390063269 ) ) ;
#2912 = CARTESIAN_POINT ( 'NONE',  ( -51.50153678516716127, -25.20718309714190042, 3.380703470003659117 ) ) ;
#2913 = CARTESIAN_POINT ( 'NONE',  ( -70.35895856474229504, -29.50249453571665725, 5.313164501615338153 ) ) ;
#2914 = CARTESIAN_POINT ( 'NONE',  ( -66.52287095715006160, -24.64965694238407323, 8.947790433994200043 ) ) ;
#2915 = ORIENTED_EDGE ( 'NONE', *, *, #97147, .F. ) ;
#2916 = CARTESIAN_POINT ( 'NONE',  ( -28.57654128002459260, -24.76880929330465975, 2.620674272415148831 ) ) ;
#2917 = CARTESIAN_POINT ( 'NONE',  ( -93.52287095715006160, -23.47596703998600631, 11.44779298504228393 ) ) ;
#2918 = VERTEX_POINT ( 'NONE', #58286 ) ;
#2919 = CARTESIAN_POINT ( 'NONE',  ( -20.13249939377427111, -5.111880259578561514, -1.500000000000002220 ) ) ;
#2920 = EDGE_LOOP ( 'NONE', ( #72097, #9257 ) ) ;
#2921 = CC_DESIGN_DATE_AND_TIME_ASSIGNMENT ( #35660, #97048, ( #94066 ) ) ;
#2923 = ORIENTED_EDGE ( 'NONE', *, *, #52677, .T. ) ;
#2922 = FACE_OUTER_BOUND ( 'NONE', #84486, .T. ) ;
#2924 = B_SPLINE_SURFACE_WITH_KNOTS ( 'NONE', 3, 3, ( 
 ( #34938, #4500, #89227, #19696 ),
 ( #35445, #58776, #48686, #60786 ),
 ( #52658, #82604, #35934, #68387 ),
 ( #12593, #43556, #37436, #82111 ),
 ( #44550, #91702, #98821, #36430 ),
 ( #14080, #74492, #51668, #51164 ),
 ( #14584, #5978, #37930, #59788 ),
 ( #5482, #99802, #29813, #60288 ),
 ( #20697, #28320, #4986, #61287 ),
 ( #28823, #66904, #22186, #97825 ) ),
 .UNSPECIFIED., .F., .F., .F.,
 ( 4, 3, 3, 4 ),
 ( 4, 4 ),
 ( 0.0004766839783818627120, 0.1491231665100170856, 0.2234464077758346878, 0.2977696490416523178 ),
 ( 0.1995180942284267289, 0.2006497111947407042 ),
 .UNSPECIFIED. ) ;
#2925 = CARTESIAN_POINT ( 'NONE',  ( 31.79364159983995464, 5.965225279485572685, -11.59305536555894278 ) ) ;
#2926 = CARTESIAN_POINT ( 'NONE',  ( 5.326923076923078426, -6.376774720514420736, 20.76772836538461320 ) ) ;
#2927 = VERTEX_POINT ( 'NONE', #74490 ) ;
#2928 = VERTEX_POINT ( 'NONE', #89225 ) ;
#2929 = CARTESIAN_POINT ( 'NONE',  ( -29.62287095715004881, -23.39678932012542845, -1.443836140311830940 ) ) ;
#2930 = CARTESIAN_POINT ( 'NONE',  ( -31.23108742109252134, -23.47593901973090169, -1.443836447538998424 ) ) ;
#2932 = ORIENTED_EDGE ( 'NONE', *, *, #56986, .F. ) ;
#2931 = CARTESIAN_POINT ( 'NONE',  ( 21.13397978930849064, -6.478279476769641221, 11.49999999999999645 ) ) ;
#2933 = FACE_OUTER_BOUND ( 'NONE', #20590, .T. ) ;
#2934 = CARTESIAN_POINT ( 'NONE',  ( -14.16962031475959272, 17.58799634409329471, 11.49999999999998934 ) ) ;
#2935 = VECTOR ( 'NONE', #98158, 1000.000000000000114 ) ;
#2936 = B_SPLINE_CURVE_WITH_KNOTS ( 'NONE', 3,
 ( #17819, #79205, #73117, #65523, #3605, #65026 ),
 .UNSPECIFIED., .F., .F.,
 ( 4, 2, 4 ),
 ( 6.391158118964604309E-06, 0.001387004593080786580, 0.002767618028042608501 ),
 .UNSPECIFIED. ) ;
#2938 = ORIENTED_EDGE ( 'NONE', *, *, #90090, .F. ) ;
#2937 = CARTESIAN_POINT ( 'NONE',  ( -75.62287095715004170, -29.50249982740957577, 7.747779886224967605 ) ) ;
#2939 = ORIENTED_EDGE ( 'NONE', *, *, #14356, .F. ) ;
#2940 = CARTESIAN_POINT ( 'NONE',  ( -93.52287095715006160, -23.47593901973090524, -1.443836447538996648 ) ) ;
#2941 = AXIS2_PLACEMENT_3D ( 'NONE', #65196, #48951, #66192 ) ;
#2942 = DIRECTION ( 'NONE',  ( 0.000000000000000000, -1.000000000000000000, 0.000000000000000000 ) ) ;
#2943 = VERTEX_POINT ( 'NONE', #27325 ) ;
#2944 = CARTESIAN_POINT ( 'NONE',  ( -20.81765089029956783, 3.879123387127271005, 11.49999999999998934 ) ) ;
#2945 = CARTESIAN_POINT ( 'NONE',  ( 29.76216731806157867, -5.356774720514427379, 26.42665638500616154 ) ) ;
#2946 = DIRECTION ( 'NONE',  ( -0.000000000000000000, 0.000000000000000000, 1.000000000000000000 ) ) ;
#2947 = DIRECTION ( 'NONE',  ( 0.000000000000000000, 0.000000000000000000, 1.000000000000000000 ) ) ;
#2948 = CARTESIAN_POINT ( 'NONE',  ( -20.66209241242137296, -8.185968977665980972, -1.500000000000002220 ) ) ;
#2949 = FACE_OUTER_BOUND ( 'NONE', #45637, .T. ) ;
#2950 = EDGE_CURVE ( 'NONE', #22734, #39283, #45201, .T. ) ;
#2951 = ORIENTED_EDGE ( 'NONE', *, *, #82704, .F. ) ;
#2952 = FACE_OUTER_BOUND ( 'NONE', #27000, .T. ) ;
#2953 = CARTESIAN_POINT ( 'NONE',  ( -48.52287095715006160, -24.65952944569304606, 1.056160979905693686 ) ) ;
#2954 = CARTESIAN_POINT ( 'NONE',  ( -18.23339674026497903, -6.527145932826366348, 11.49999999999999645 ) ) ;
#2955 = CARTESIAN_POINT ( 'NONE',  ( -36.56104652793175802, -23.73791477778911130, 11.05961554403171121 ) ) ;
#2956 = CARTESIAN_POINT ( 'NONE',  ( 26.73860345374794178, 1.477225279485574028, -1.272392034746785860 ) ) ;
#2957 = CARTESIAN_POINT ( 'NONE',  ( -4.154358412494840280, 19.03220294597612039, 11.49999999999998934 ) ) ;
#2958 = EDGE_CURVE ( 'NONE', #72281, #69181, #20195, .T. ) ;
#2959 = CARTESIAN_POINT ( 'NONE',  ( 17.37860173834871347, 12.56526366372364301, 11.49999999999998934 ) ) ;
#2960 = PLANE ( 'NONE',  #45023 ) ;
#2961 = CARTESIAN_POINT ( 'NONE',  ( -0.7614568544629641833, -5.876774720514408301, 19.18727597066020962 ) ) ;
#2962 = EDGE_CURVE ( 'NONE', #38599, #77757, #3484, .T. ) ;
#2963 = CARTESIAN_POINT ( 'NONE',  ( -66.62287095715005592, -29.50250243563736774, 8.947779886222143375 ) ) ;
#2964 = DIRECTION ( 'NONE',  ( -0.4009304992412306978, -6.454799914155190814E-16, -0.9161084732596777025 ) ) ;
#2965 = CARTESIAN_POINT ( 'NONE',  ( 16.48639501038195121, -15.69157857782056276, -1.500000000000002220 ) ) ;
#2966 = CARTESIAN_POINT ( 'NONE',  ( 3.422029459436209011E-17, -20.94946567084330979, 2.842192172511120715E-16 ) ) ;
#2967 = CARTESIAN_POINT ( 'NONE',  ( -106.5112337399359035, -24.66019654487200441, 8.947790411086108620 ) ) ;
#2968 = CARTESIAN_POINT ( 'NONE',  ( -101.5228709571500900, -24.66019654487200441, 8.947790411086119278 ) ) ;
#2969 = CARTESIAN_POINT ( 'NONE',  ( 14.81759351585047391, 13.34335055255382052, 11.49999999999999645 ) ) ;
#2970 = CARTESIAN_POINT ( 'NONE',  ( -78.55620429048339304, -24.64898659630528854, 1.056161002820828143 ) ) ;
#2971 = B_SPLINE_CURVE_WITH_KNOTS ( 'NONE', 3,
 ( #23269, #78554, #38511, #92294 ),
 .UNSPECIFIED., .F., .F.,
 ( 4, 4 ),
 ( 0.000000000000000000, 1.000000000000000000 ),
 .UNSPECIFIED. ) ;
#2972 = DIRECTION ( 'NONE',  ( 0.000000000000000000, -1.000000000000000000, 0.000000000000000000 ) ) ;
#2973 = CARTESIAN_POINT ( 'NONE',  ( -56.92287095715008149, -23.47596703998600276, 11.44779298504227860 ) ) ;
#2974 = EDGE_LOOP ( 'NONE', ( #28351, #59246, #47547, #91223, #17126 ) ) ;
#2975 = ADVANCED_FACE ( 'NONE', ( #50665 ), #29312, .T. ) ;
#2976 = PLANE ( 'NONE',  #5579 ) ;
#2977 = CARTESIAN_POINT ( 'NONE',  ( -77.52287095715009002, -24.34917612406836795, 0.1852690917426540462 ) ) ;
#2978 = B_SPLINE_CURVE_WITH_KNOTS ( 'NONE', 3,
 ( #35766, #52486, #83416, #13903 ),
 .UNSPECIFIED., .F., .F.,
 ( 4, 4 ),
 ( 0.4208004833249490706, 0.4298069145970646598 ),
 .UNSPECIFIED. ) ;
#2979 = CARTESIAN_POINT ( 'NONE',  ( -21.46818342838279392, -2.986162219498790904, 11.49999999999998934 ) ) ;
#2980 = CARTESIAN_POINT ( 'NONE',  ( -51.93149462243455616, -25.25905089634592571, 6.174051128686508072 ) ) ;
#2981 = CARTESIAN_POINT ( 'NONE',  ( 13.74000504945409418, 13.82049530813991467, -1.500000000000002220 ) ) ;
#2982 = CARTESIAN_POINT ( 'NONE',  ( -49.52287095715006160, -23.48783264082477018, -1.443836473390095465 ) ) ;
#2983 = ORIENTED_EDGE ( 'NONE', *, *, #54716, .T. ) ;
#2984 = SHAPE_DEFINITION_REPRESENTATION ( #64431, #44034 ) ;
#2985 = CARTESIAN_POINT ( 'NONE',  ( -69.62287095715009855, -23.95044443724992078, 10.65354141964650125 ) ) ;
#2986 = CARTESIAN_POINT ( 'NONE',  ( 10.07161678670223637, 17.78519941539584792, 11.49999999999999645 ) ) ;
#2987 = CARTESIAN_POINT ( 'NONE',  ( -128.5228709571500474, -23.48783264083417066, -1.443836473375472274 ) ) ;
#2988 = B_SPLINE_CURVE_WITH_KNOTS ( 'NONE', 3,
 ( #53597, #22113, #14508, #45483 ),
 .UNSPECIFIED., .F., .F.,
 ( 4, 4 ),
 ( 0.000000000000000000, 0.0001000000000000167422 ),
 .UNSPECIFIED. ) ;
#2989 = DIRECTION ( 'NONE',  ( 0.06474050504609950296, -0.8381167135261472501, -0.5416355246053439210 ) ) ;
#2990 = VERTEX_POINT ( 'NONE', #91209 ) ;
#2991 = CARTESIAN_POINT ( 'NONE',  ( -52.62287095715004170, -23.47596703998600276, 11.44779298504227505 ) ) ;
#2992 = CARTESIAN_POINT ( 'NONE',  ( -40.52287095715006870, -23.48786465467241058, 11.44779295918255180 ) ) ;
#2993 = CARTESIAN_POINT ( 'NONE',  ( -39.06913928595307084, -25.27985329021985805, 4.503859356828002092 ) ) ;
#2994 = CARTESIAN_POINT ( 'NONE',  ( -49.28110964179429487, -25.31439463334452000, 6.053971487819386432 ) ) ;
#2995 = CARTESIAN_POINT ( 'NONE',  ( -109.6260488237147257, -24.34968618360934300, 0.1864209137778879144 ) ) ;
#2996 = ORIENTED_EDGE ( 'NONE', *, *, #70286, .F. ) ;
#2997 = CARTESIAN_POINT ( 'NONE',  ( -66.59743546961844629, -23.96169478059713143, 10.65365249895718058 ) ) ;
#2998 = AXIS2_PLACEMENT_3D ( 'NONE', #19182, #50644, #47269 ) ;
#2999 = ADVANCED_FACE ( 'NONE', ( #81613 ), #82109, .F. ) ;
#3000 = CARTESIAN_POINT ( 'NONE',  ( -21.75629724252761577, 7.406401271465676395, 11.49999999999999645 ) ) ;
#3001 = CARTESIAN_POINT ( 'NONE',  ( 18.68554041145753786, -12.99315341008173519, 11.49999999999998934 ) ) ;
#3002 = CARTESIAN_POINT ( 'NONE',  ( -110.5124691553814102, -24.73531770709095312, 8.716586749053508498 ) ) ;
#3003 = CARTESIAN_POINT ( 'NONE',  ( -28.98875734969026041, 3.316774720514426456, 26.43402280011862615 ) ) ;
#3004 = CARTESIAN_POINT ( 'NONE',  ( -81.52287095715006160, -23.47596703998600631, 11.44779298504228571 ) ) ;
#3005 = CARTESIAN_POINT ( 'NONE',  ( -74.52287095715007581, -23.48786465467241058, 11.44779295918254647 ) ) ;
#3006 = DIRECTION ( 'NONE',  ( 1.000000000000000000, 3.773278334444166432E-23, 8.201307841325785021E-29 ) ) ;
#3007 = CARTESIAN_POINT ( 'NONE',  ( -19.96805355746080934, -8.928269573510897672, -1.500000000000002220 ) ) ;
#3008 = CARTESIAN_POINT ( 'NONE',  ( -69.49425340576027565, -24.66019654487199375, 8.947790411086119278 ) ) ;
#3009 = EDGE_CURVE ( 'NONE', #43349, #54056, #22502, .T. ) ;
#3010 = CARTESIAN_POINT ( 'NONE',  ( -27.39359161974487122, -24.75620229959870500, 2.307003371749687837 ) ) ;
#3011 = DIRECTION ( 'NONE',  ( -3.773278334444166432E-23, 1.000000000000000000, 0.000000000000000000 ) ) ;
#3012 = CARTESIAN_POINT ( 'NONE',  ( -99.14000973721185517, -25.31200576846117656, 5.341016405764093200 ) ) ;
#3013 = VERTEX_POINT ( 'NONE', #59272 ) ;
#3014 = VECTOR ( 'NONE', #49035, 1000.000000000000000 ) ;
#3015 = CARTESIAN_POINT ( 'NONE',  ( -17.38880980700008294, 10.71821138944157603, 11.49999999999998934 ) ) ;
#3016 = ORIENTED_EDGE ( 'NONE', *, *, #24626, .T. ) ;
#3017 = ORIENTED_EDGE ( 'NONE', *, *, #25149, .T. ) ;
#3018 = CARTESIAN_POINT ( 'NONE',  ( 22.51966570110743149, 4.691836548664650053, -1.500000000000002220 ) ) ;
#3019 = CARTESIAN_POINT ( 'NONE',  ( -80.52287095715001897, -24.52232992886362339, 0.6492154411906039257 ) ) ;
#3020 = VERTEX_POINT ( 'NONE', #67392 ) ;
#3021 = CARTESIAN_POINT ( 'NONE',  ( -29.52287095715006160, -24.57685061924431835, 8.947790457046968626 ) ) ;
#3022 = DIRECTION ( 'NONE',  ( -0.000000000000000000, 1.000000000000000000, -0.000000000000000000 ) ) ;
#3023 = CARTESIAN_POINT ( 'NONE',  ( 26.37445894957760828, 1.682774720514426114, -11.69480419648520986 ) ) ;
#3024 = CARTESIAN_POINT ( 'NONE',  ( -117.5800378283677929, -25.21791271819481750, 6.461860001696705602 ) ) ;
#3025 = VECTOR ( 'NONE', #94064, 1000.000000000000114 ) ;
#3027 = ORIENTED_EDGE ( 'NONE', *, *, #44790, .T. ) ;
#3026 = CARTESIAN_POINT ( 'NONE',  ( 21.30238844577196389, 2.035401582669650544, 11.49999999999999645 ) ) ;
#3028 = VERTEX_POINT ( 'NONE', #45056 ) ;
#3029 = CARTESIAN_POINT ( 'NONE',  ( -19.97062832128981213, -9.750827054148329509, -1.500000000000002220 ) ) ;
#3030 = CARTESIAN_POINT ( 'NONE',  ( -4.528870947376731237, 20.18191347215651987, -1.500000000000002220 ) ) ;
#3031 = EDGE_CURVE ( 'NONE', #56230, #85117, #66392, .T. ) ;
#3032 = ORIENTED_EDGE ( 'NONE', *, *, #94322, .T. ) ;
#3033 = CARTESIAN_POINT ( 'NONE',  ( -5.850750514176234596, -6.376774720514411854, 19.74039977944280366 ) ) ;
#3034 = CARTESIAN_POINT ( 'NONE',  ( 3.121233215686890272, -5.876774720514405637, 18.93204046835445808 ) ) ;
#3035 = VERTEX_POINT ( 'NONE', #5480 ) ;
#3036 = CARTESIAN_POINT ( 'NONE',  ( -83.62287095715005592, -24.64965695001468404, 8.947790433994182280 ) ) ;
#3037 = EDGE_LOOP ( 'NONE', ( #81822, #51213 ) ) ;
#3038 = CARTESIAN_POINT ( 'NONE',  ( 12.99736557111424595, 6.475225279485574248, -27.13536621820933448 ) ) ;
#3039 = CARTESIAN_POINT ( 'NONE',  ( 19.90007246472742608, 6.374896562862660154, -1.500000000000002220 ) ) ;
#3040 = CARTESIAN_POINT ( 'NONE',  ( -21.72861685410901700, 2.547970858986955189, 11.49999999999999645 ) ) ;
#3041 = DIRECTION ( 'NONE',  ( 0.000000000000000000, 0.000000000000000000, -1.000000000000000000 ) ) ;
#3042 = DIRECTION ( 'NONE',  ( -3.773278334453079030E-23, 0.9999999999976377785, 2.173523156925979128E-06 ) ) ;
#3043 = CARTESIAN_POINT ( 'NONE',  ( 16.80569330386292748, 14.95695114220347932, 11.49999999999998934 ) ) ;
#3044 = EDGE_CURVE ( 'NONE', #52189, #91108, #56592, .T. ) ;
#3045 = EDGE_CURVE ( 'NONE', #27537, #59423, #30039, .T. ) ;
#3046 = CARTESIAN_POINT ( 'NONE',  ( 2.438461900574103502, 20.79476225230834174, -1.500000000000002220 ) ) ;
#3047 = FACE_OUTER_BOUND ( 'NONE', #33648, .T. ) ;
#3048 = CARTESIAN_POINT ( 'NONE',  ( 21.57151214508649772, -9.529487854913506695, 0.000000000000000000 ) ) ;
#3049 = DIRECTION ( 'NONE',  ( 0.000000000000000000, -1.000000000000000000, 0.000000000000000000 ) ) ;
#3050 = ORIENTED_EDGE ( 'NONE', *, *, #34766, .F. ) ;
#3051 = EDGE_CURVE ( 'NONE', #8894, #9998, #21597, .T. ) ;
#3052 = ORIENTED_EDGE ( 'NONE', *, *, #35638, .T. ) ;
#3053 = EDGE_LOOP ( 'NONE', ( #97371, #48906, #90486, #17493 ) ) ;
#3054 = CARTESIAN_POINT ( 'NONE',  ( -52.59322633568044125, -24.15543982623907482, -0.2315651400026529916 ) ) ;
#3055 = ORIENTED_EDGE ( 'NONE', *, *, #37873, .T. ) ;
#3056 = CARTESIAN_POINT ( 'NONE',  ( 9.091334071971768793, -19.38302982324925239, -1.500000000000002220 ) ) ;
#3057 = ORIENTED_EDGE ( 'NONE', *, *, #15059, .F. ) ;
#3058 = CARTESIAN_POINT ( 'NONE',  ( -59.52287095715006160, -24.65952944569304961, 1.056160979905695463 ) ) ;
#3059 = CARTESIAN_POINT ( 'NONE',  ( -1.999300432013352058, 20.99099883833691749, -1.500000000000002220 ) ) ;
#3060 = DIRECTION ( 'NONE',  ( 0.9975640502598241977, -0.06975647374412546897, -0.000000000000000000 ) ) ;
#3061 = VECTOR ( 'NONE', #74120, 1000.000000000000000 ) ;
#3062 = CARTESIAN_POINT ( 'NONE',  ( 29.73860345376319714, 1.477225279485574028, -8.849814207987165560 ) ) ;
#3064 = CARTESIAN_POINT ( 'NONE',  ( -50.59276831212685011, -24.40133493613049964, 9.663955038902802386 ) ) ;
#3063 = AXIS2_PLACEMENT_3D ( 'NONE', #65182, #59044, #35206 ) ;
#3065 = CARTESIAN_POINT ( 'NONE',  ( -101.5550284192910482, -23.96119346886880663, -0.6495511937832049165 ) ) ;
#3066 = CARTESIAN_POINT ( 'NONE',  ( -109.4123506053088306, -25.30719144561626877, 4.546003555234384486 ) ) ;
#3067 = CARTESIAN_POINT ( 'NONE',  ( 21.39010012190943755, 5.354582491813655309, -1.500000000000002220 ) ) ;
#3068 = ORIENTED_EDGE ( 'NONE', *, *, #45751, .T. ) ;
#3069 = CARTESIAN_POINT ( 'NONE',  ( -65.58632257377641395, -24.63419186844610920, 9.035850630976922204 ) ) ;
#3070 = EDGE_CURVE ( 'NONE', #11582, #5913, #25199, .T. ) ;
#3071 = PLANE ( 'NONE',  #18985 ) ;
#3072 = CARTESIAN_POINT ( 'NONE',  ( -63.52287095715004739, -23.47593901973090169, -1.443836447538996870 ) ) ;
#3073 = VECTOR ( 'NONE', #23590, 1000.000000000000114 ) ;
#3074 = CARTESIAN_POINT ( 'NONE',  ( -29.83767755215908579, -25.25218218361323963, 3.798368663089754182 ) ) ;
#3075 = LINE ( 'NONE', #44500, #24622 ) ;
#3077 = CARTESIAN_POINT ( 'NONE',  ( -57.62287095715004881, -24.64965695001468404, 8.947790433994185832 ) ) ;
#3076 = VECTOR ( 'NONE', #82099, 1000.000000000000114 ) ;
#3078 = CARTESIAN_POINT ( 'NONE',  ( -16.05942832139214360, -14.02155611864158402, -1.500000000000002220 ) ) ;
#3079 = DIRECTION ( 'NONE',  ( 1.000000000000000000, 0.000000000000000000, 0.000000000000000000 ) ) ;
#3080 = LINE ( 'NONE', #71587, #43068 ) ;
#3081 = EDGE_CURVE ( 'NONE', #59423, #22424, #61519, .T. ) ;
#3082 = DIRECTION ( 'NONE',  ( -0.4725087886537609472, 0.000000000000000000, -0.8813259582271223413 ) ) ;
#3083 = CARTESIAN_POINT ( 'NONE',  ( -85.52287095715006160, -23.48783264082476663, -1.443836473390089470 ) ) ;
#3084 = CARTESIAN_POINT ( 'NONE',  ( -5.352388609804938469, -21.92410630658433845, -1.500000000000002220 ) ) ;
#3085 = B_SPLINE_CURVE_WITH_KNOTS ( 'NONE', 3,
 ( #61304, #53690, #92230, #53189, #14605, #5500 ),
 .UNSPECIFIED., .F., .F.,
 ( 4, 2, 4 ),
 ( 0.000000000000000000, 0.001380764517854767568, 0.002761529035709535135 ),
 .UNSPECIFIED. ) ;
#3086 = EDGE_CURVE ( 'NONE', #88166, #85265, #948, .T. ) ;
#3087 = PLANE ( 'NONE',  #91147 ) ;
#3088 = VERTEX_POINT ( 'NONE', #39430 ) ;
#3089 = CYLINDRICAL_SURFACE ( 'NONE', #77343, 4.300000000000000711 ) ;
#3090 = CARTESIAN_POINT ( 'NONE',  ( 7.853763894818856173, -10.48276843398940272, 1.273485471867758401 ) ) ;
#3091 = CARTESIAN_POINT ( 'NONE',  ( -2.117704968268854682, 19.61795684621070990, 11.49999999999999645 ) ) ;
#3092 = CARTESIAN_POINT ( 'NONE',  ( -65.05438548721848235, 5.356774720514425603, 0.7300228001186309656 ) ) ;
#3093 = VECTOR ( 'NONE', #1740, 1000.000000000000000 ) ;
#3094 = CARTESIAN_POINT ( 'NONE',  ( -40.52287095715005449, -23.48783264082476308, -1.443836473390097908 ) ) ;
#3095 = B_SPLINE_CURVE_WITH_KNOTS ( 'NONE', 3,
 ( #69867, #78963, #31297, #85083, #32300, #61768 ),
 .UNSPECIFIED., .F., .F.,
 ( 4, 2, 4 ),
 ( 1.570755371634033063E-05, 0.001396183895866086886, 0.002776660238015833410 ),
 .UNSPECIFIED. ) ;
#3096 = ORIENTED_EDGE ( 'NONE', *, *, #26536, .F. ) ;
#3097 = EDGE_CURVE ( 'NONE', #53939, #31747, #5793, .T. ) ;
#3098 = CARTESIAN_POINT ( 'NONE',  ( -3.212051231530180573, 17.72614232434105119, 9.000000000000000000 ) ) ;
#3099 = DIRECTION ( 'NONE',  ( -3.773278334453080206E-23, 0.9999999999976377785, 2.173523156925979975E-06 ) ) ;
#3100 = CARTESIAN_POINT ( 'NONE',  ( -105.5228709571500616, -24.15516710230294706, 10.28746687063725496 ) ) ;
#3101 = CARTESIAN_POINT ( 'NONE',  ( -21.33164055427280914, -3.227942221655450972, 11.49999999999998934 ) ) ;
#3102 = FACE_OUTER_BOUND ( 'NONE', #78911, .T. ) ;
#3103 = CARTESIAN_POINT ( 'NONE',  ( -76.55620429048340725, -24.66019654487199375, 8.947790411086128159 ) ) ;
#3104 = EDGE_CURVE ( 'NONE', #19708, #1781, #7466, .T. ) ;
#3105 = DIRECTION ( 'NONE',  ( 0.000000000000000000, -1.000000000000000000, 0.000000000000000000 ) ) ;
#3106 = PLANE ( 'NONE',  #81504 ) ;
#3107 = CARTESIAN_POINT ( 'NONE',  ( -19.69265041987409859, 1.759638296948408787, 11.49999999999998934 ) ) ;
#3108 = ORIENTED_EDGE ( 'NONE', *, *, #23303, .F. ) ;
#3109 = CARTESIAN_POINT ( 'NONE',  ( -19.75413285895528404, 4.560271753130525241, 11.49999999999999645 ) ) ;
#3110 = CARTESIAN_POINT ( 'NONE',  ( -6.901944873432418248, -5.876774720514410966, 19.15221817653406688 ) ) ;
#3111 = VECTOR ( 'NONE', #24656, 1000.000000000000114 ) ;
#3112 = VERTEX_POINT ( 'NONE', #6979 ) ;
#3113 = CARTESIAN_POINT ( 'NONE',  ( -52.52287095715006870, -24.65952944569303895, 1.056160979905693686 ) ) ;
#3114 = CARTESIAN_POINT ( 'NONE',  ( -99.54853273079524456, -25.27620648591849317, 4.157275027402507206 ) ) ;
#3115 = CARTESIAN_POINT ( 'NONE',  ( -59.52287095715006160, -23.48786465467241769, 11.44779295918254824 ) ) ;
#3116 = CARTESIAN_POINT ( 'NONE',  ( -31.52287095715006160, -23.48786465467240347, 11.44779295918255357 ) ) ;
#3117 = DIRECTION ( 'NONE',  ( 0.000000000000000000, -1.000000000000000000, 0.000000000000000000 ) ) ;
#3118 = LINE ( 'NONE', #27444, #30035 ) ;
#3119 = CARTESIAN_POINT ( 'NONE',  ( 18.22975119132022215, -8.346483668847822557, 11.49999999999998934 ) ) ;
#3120 = CARTESIAN_POINT ( 'NONE',  ( 33.69795529655567634, -6.475225279485573360, 20.86760796525322093 ) ) ;
#3121 = VERTEX_POINT ( 'NONE', #85594 ) ;
#3122 = EDGE_CURVE ( 'NONE', #27644, #75868, #55405, .T. ) ;
#3123 = CARTESIAN_POINT ( 'NONE',  ( -58.58953762381672448, -24.66019654487199375, 8.947790411086138818 ) ) ;
#3124 = CARTESIAN_POINT ( 'NONE',  ( -35.47582077153254687, -24.73486907724917572, 1.287355809206972346 ) ) ;
#3125 = CARTESIAN_POINT ( 'NONE',  ( -79.60960783475657365, -25.30268815552712525, 5.271914168462072503 ) ) ;
#3126 = CARTESIAN_POINT ( 'NONE',  ( -60.52287095715006160, -29.50247984919015209, -1.443849546365056913 ) ) ;
#3127 = CARTESIAN_POINT ( 'NONE',  ( -100.8386611319390340, -25.11990008798473539, 2.885623019206728479 ) ) ;
#3128 = EDGE_CURVE ( 'NONE', #56669, #59957, #73555, .T. ) ;
#3129 = CARTESIAN_POINT ( 'NONE',  ( -118.5228709571500758, -23.47593901973090524, -1.443836447538996204 ) ) ;
#3130 = ORIENTED_EDGE ( 'NONE', *, *, #43922, .F. ) ;
#3131 = AXIS2_PLACEMENT_3D ( 'NONE', #74977, #4498, #60285 ) ;
#3132 = AXIS2_PLACEMENT_3D ( 'NONE', #53415, #44805, #83848 ) ;
#3133 = CARTESIAN_POINT ( 'NONE',  ( -12.25758032491116367, 16.21837406056298292, -1.500000000000002220 ) ) ;
#3134 = ORIENTED_EDGE ( 'NONE', *, *, #1202, .F. ) ;
#3135 = CARTESIAN_POINT ( 'NONE',  ( 31.62961302973990030, 4.065030569019225659, 27.09489828165477476 ) ) ;
#3136 = CARTESIAN_POINT ( 'NONE',  ( -122.5228709571501327, -23.96127896941632329, -0.6493128931037981388 ) ) ;
#3137 = ORIENTED_EDGE ( 'NONE', *, *, #51496, .F. ) ;
#3138 = VECTOR ( 'NONE', #67185, 1000.000000000000114 ) ;
#3139 = CARTESIAN_POINT ( 'NONE',  ( -59.63219212808159853, -24.35071581493543746, 9.817618358456035921 ) ) ;
#3140 = CARTESIAN_POINT ( 'NONE',  ( -50.36234373730416536, -25.12215419459477417, 7.100827092886333958 ) ) ;
#3141 = VECTOR ( 'NONE', #68135, 1000.000000000000000 ) ;
#3142 = CARTESIAN_POINT ( 'NONE',  ( -30.47287095715008221, -25.15028201304190603, 6.970007236040878240 ) ) ;
#3143 = CARTESIAN_POINT ( 'NONE',  ( 15.88363568188429653, -14.04911357082368006, 11.49999999999999645 ) ) ;
#3144 = AXIS2_PLACEMENT_3D ( 'NONE', #58903, #43673, #74611 ) ;
#3145 = CARTESIAN_POINT ( 'NONE',  ( -14.81638660137672225, 16.44347145309322045, -1.500000000000002220 ) ) ;
#3146 = CARTESIAN_POINT ( 'NONE',  ( -10.57813111170615983, 17.65445453266677234, 11.49999999999998934 ) ) ;
#3147 = EDGE_CURVE ( 'NONE', #50923, #42247, #15086, .T. ) ;
#3148 = ORIENTED_EDGE ( 'NONE', *, *, #56843, .T. ) ;
#3149 = CARTESIAN_POINT ( 'NONE',  ( -94.52287095715010423, -23.96177878511309345, 10.65340807706329862 ) ) ;
#3150 = EDGE_LOOP ( 'NONE', ( #74660, #92380, #60576, #31729 ) ) ;
#3151 = CARTESIAN_POINT ( 'NONE',  ( -54.62367899608845789, -24.65952944569304606, 1.056160979905696573 ) ) ;
#3152 = CARTESIAN_POINT ( 'NONE',  ( -49.62287095715005592, -23.47593901973091235, -1.443836447539009749 ) ) ;
#3153 = VERTEX_POINT ( 'NONE', #99318 ) ;
#3154 = ORIENTED_EDGE ( 'NONE', *, *, #3971, .F. ) ;
#3155 = ORIENTED_EDGE ( 'NONE', *, *, #35938, .T. ) ;
#3156 = CARTESIAN_POINT ( 'NONE',  ( -116.6228709571500559, -24.64965695001469115, 8.947790433994175174 ) ) ;
#3157 = CARTESIAN_POINT ( 'NONE',  ( 6.853365600657045142, -6.376774720514415407, 20.20310688689519196 ) ) ;
#3158 = CARTESIAN_POINT ( 'NONE',  ( 6.329711958793041049, -6.376774720514411854, 19.73172534246499765 ) ) ;
#3159 = CARTESIAN_POINT ( 'NONE',  ( 15.29587703590233971, -13.95322596517325664, -1.500000000000002220 ) ) ;
#3160 = CARTESIAN_POINT ( 'NONE',  ( 19.28387207504633949, -9.851753786812027514, 11.49999999999999645 ) ) ;
#3161 = ORIENTED_EDGE ( 'NONE', *, *, #88054, .F. ) ;
#3162 = EDGE_CURVE ( 'NONE', #58462, #54139, #50546, .T. ) ;
#3163 = CARTESIAN_POINT ( 'NONE',  ( -98.89858548345738143, -25.26741689086502518, 5.967726646190992135 ) ) ;
#3164 = CARTESIAN_POINT ( 'NONE',  ( -109.5562042904833646, -23.48786465467241769, 11.44779295918253581 ) ) ;
#3165 = CARTESIAN_POINT ( 'NONE',  ( -12.73782554413503654, -18.45060914899308457, -1.500000000000002220 ) ) ;
#3166 = ADVANCED_FACE ( 'NONE', ( #37434 ), #38425, .T. ) ;
#3167 = EDGE_CURVE ( 'NONE', #20563, #14365, #54663, .T. ) ;
#3168 = CARTESIAN_POINT ( 'NONE',  ( 32.33217928425156629, -6.475225279485573360, -12.20610769812808982 ) ) ;
#3169 = LINE ( 'NONE', #95497, #9213 ) ;
#3170 = ORIENTED_EDGE ( 'NONE', *, *, #13788, .T. ) ;
#3171 = CARTESIAN_POINT ( 'NONE',  ( 29.65385891689261655, 5.748374461104726940, 28.02705487427158104 ) ) ;
#3172 = CARTESIAN_POINT ( 'NONE',  ( 13.35520464978777788, -3.511397109468809674, -28.20545335007043164 ) ) ;
#3173 = ADVANCED_FACE ( 'NONE', ( #47051 ), #55172, .F. ) ;
#3174 = ORIENTED_EDGE ( 'NONE', *, *, #35349, .F. ) ;
#3175 = ORIENTED_EDGE ( 'NONE', *, *, #68361, .F. ) ;
#3176 = DIRECTION ( 'NONE',  ( 0.000000000000000000, -0.000000000000000000, -1.000000000000000000 ) ) ;
#3177 = ORIENTED_EDGE ( 'NONE', *, *, #77143, .F. ) ;
#3178 = CARTESIAN_POINT ( 'NONE',  ( -100.9228709571500815, -23.47596703998600631, 11.44779298504227860 ) ) ;
#3179 = CARTESIAN_POINT ( 'NONE',  ( 7.993063233546146229, -19.64520799392144568, -1.500000000000002220 ) ) ;
#3180 = ORIENTED_EDGE ( 'NONE', *, *, #26797, .F. ) ;
#3181 = CARTESIAN_POINT ( 'NONE',  ( -88.64270303220058622, -23.48783264082477018, -1.443836473390093467 ) ) ;
#3182 = CARTESIAN_POINT ( 'NONE',  ( -1.743439162979827595, 21.76861016152796324, -1.500000000000002220 ) ) ;
#3183 = CARTESIAN_POINT ( 'NONE',  ( -52.49583607988384415, -24.35071581493542681, 9.817618358456037697 ) ) ;
#3184 = CARTESIAN_POINT ( 'NONE',  ( -119.4728709571500502, -29.48149383318413541, 5.000941581248042667 ) ) ;
#3185 = DIRECTION ( 'NONE',  ( 0.000000000000000000, 0.000000000000000000, -1.000000000000000000 ) ) ;
#3186 = CARTESIAN_POINT ( 'NONE',  ( 16.40513048700843513, 14.50174154637248591, -1.500000000000002220 ) ) ;
#3187 = DIRECTION ( 'NONE',  ( -3.773278334453079030E-23, 0.9999999999976377785, 2.173523156925979128E-06 ) ) ;
#3188 = ORIENTED_EDGE ( 'NONE', *, *, #27940, .F. ) ;
#3189 = CARTESIAN_POINT ( 'NONE',  ( 25.82028661651826340, 4.376709120396486519, -11.31108007975979923 ) ) ;
#3191 = EDGE_CURVE ( 'NONE', #76987, #54552, #68384, .T. ) ;
#3190 = CARTESIAN_POINT ( 'NONE',  ( -85.49691046782774606, -24.92592662359561473, 8.075495903018000021 ) ) ;
#3192 = ADVANCED_FACE ( 'NONE', ( #18092 ), #1239, .T. ) ;
#3193 = EDGE_LOOP ( 'NONE', ( #93746, #91635, #100206, #8613 ) ) ;
#3194 = EDGE_CURVE ( 'NONE', #3328, #58613, #88113, .T. ) ;
#3195 = CARTESIAN_POINT ( 'NONE',  ( -90.62287095715002749, -24.83602698348159876, 1.605859176311266845 ) ) ;
#3196 = ORIENTED_EDGE ( 'NONE', *, *, #92370, .F. ) ;
#3197 = DIRECTION ( 'NONE',  ( 0.000000000000000000, 0.9999999999976377785, 2.173523156925979128E-06 ) ) ;
#3198 = CARTESIAN_POINT ( 'NONE',  ( -82.62632419238170201, -24.51314013834315375, 0.6176544820404169522 ) ) ;
#3199 = CARTESIAN_POINT ( 'NONE',  ( -18.66175431467001999, 10.11895122522205526, -1.500000000000002220 ) ) ;
#3200 = FACE_OUTER_BOUND ( 'NONE', #15248, .T. ) ;
#3201 = CARTESIAN_POINT ( 'NONE',  ( -30.56674980027052513, -25.57033040079277697, 6.142048374048878046 ) ) ;
#3202 = VECTOR ( 'NONE', #11055, 1000.000000000000000 ) ;
#3203 = EDGE_CURVE ( 'NONE', #70138, #48999, #48563, .T. ) ;
#3204 = FACE_OUTER_BOUND ( 'NONE', #20709, .T. ) ;
#3205 = CARTESIAN_POINT ( 'NONE',  ( -129.5228709571501042, -24.34917612406838572, 0.1852690917426648154 ) ) ;
#3206 = CARTESIAN_POINT ( 'NONE',  ( -2.795030477444873540, 19.22867370847827573, -1.500000000000002220 ) ) ;
#3207 = CARTESIAN_POINT ( 'NONE',  ( -45.62377143496699006, -25.00158670708910691, 2.256160236439225031 ) ) ;
#3208 = EDGE_LOOP ( 'NONE', ( #32083, #72723, #89118, #65795 ) ) ;
#3209 = CARTESIAN_POINT ( 'NONE',  ( 11.71876819965036809, 15.69520123712499249, 11.49999999999999645 ) ) ;
#3210 = FACE_OUTER_BOUND ( 'NONE', #43603, .T. ) ;
#3211 = AXIS2_PLACEMENT_3D ( 'NONE', #39172, #55924, #86846 ) ;
#3212 = CARTESIAN_POINT ( 'NONE',  ( -33.62287095715005592, -29.50250243563736774, 8.947779886222150481 ) ) ;
#3213 = EDGE_LOOP ( 'NONE', ( #55601, #25717, #70925, #79240 ) ) ;
#3214 = ADVANCED_FACE ( 'NONE', ( #33816 ), #67593, .T. ) ;
#3215 = CARTESIAN_POINT ( 'NONE',  ( 4.189750619059152470, -5.876774720514426953, 21.76591699724029283 ) ) ;
#3216 = CARTESIAN_POINT ( 'NONE',  ( -75.62287095715004170, -24.52232992886363405, 0.6492154411906084777 ) ) ;
#3217 = VECTOR ( 'NONE', #11143, 1000.000000000000000 ) ;
#3218 = B_SPLINE_CURVE_WITH_KNOTS ( 'NONE', 3,
 ( #58428, #59924, #81244, #83236 ),
 .UNSPECIFIED., .F., .F.,
 ( 4, 4 ),
 ( 0.000000000000000000, 1.000000000000000000 ),
 .UNSPECIFIED. ) ;
#3220 = EDGE_CURVE ( 'NONE', #71152, #10158, #81994, .T. ) ;
#3219 = CARTESIAN_POINT ( 'NONE',  ( -2.499999999999986677, 22.00000000000000000, 2.100000000000000089 ) ) ;
#3221 = CARTESIAN_POINT ( 'NONE',  ( -81.79035934495350091, -25.24813800626475668, 6.685839573822437210 ) ) ;
#3222 = CARTESIAN_POINT ( 'NONE',  ( 19.69511366699831001, -0.05742560045514189665, 11.49999999999998934 ) ) ;
#3223 = EDGE_CURVE ( 'NONE', #91718, #55380, #77116, .T. ) ;
#3224 = AXIS2_PLACEMENT_3D ( 'NONE', #24463, #47811, #56440 ) ;
#3225 = VERTEX_POINT ( 'NONE', #42944 ) ;
#3226 = VECTOR ( 'NONE', #72604, 1000.000000000000000 ) ;
#3227 = PLANE ( 'NONE',  #3494 ) ;
#3228 = FACE_OUTER_BOUND ( 'NONE', #274, .T. ) ;
#3229 = VECTOR ( 'NONE', #54579, 1000.000000000000000 ) ;
#3230 = MECHANICAL_CONTEXT ( 'NONE', #80333, 'mechanical' ) ;
#3231 = ORIENTED_EDGE ( 'NONE', *, *, #8216, .T. ) ;
#3232 = CARTESIAN_POINT ( 'NONE',  ( -125.5228709571500900, -24.52323809116986197, 9.355190652339425483 ) ) ;
#3233 = CARTESIAN_POINT ( 'NONE',  ( -105.6228709571500133, -24.14406661707766588, 10.28769366152058318 ) ) ;
#3234 = DIRECTION ( 'NONE',  ( -3.773278334453080206E-23, 0.9999999999976377785, 2.173523156925979975E-06 ) ) ;
#3235 = CARTESIAN_POINT ( 'NONE',  ( -97.63250974841577090, -23.96169478059714208, 10.65365249895717703 ) ) ;
#3236 = CARTESIAN_POINT ( 'NONE',  ( -102.6228709571500559, -24.64965695001469115, 8.947790433994178727 ) ) ;
#3237 = CYLINDRICAL_SURFACE ( 'NONE', #22990, 84.48086791635432746 ) ;
#3238 = DIRECTION ( 'NONE',  ( -0.000000000000000000, 1.000000000000000000, -0.000000000000000000 ) ) ;
#3239 = CARTESIAN_POINT ( 'NONE',  ( 19.59856454566043382, -3.714209461170434157, 11.49999999999998934 ) ) ;
#3240 = CARTESIAN_POINT ( 'NONE',  ( -101.1018588697504157, -25.22871456504708121, 3.550613621098617223 ) ) ;
#3241 = CARTESIAN_POINT ( 'NONE',  ( -1.345660788846553935, -19.86331345790170033, -1.500000000000002220 ) ) ;
#3242 = VERTEX_POINT ( 'NONE', #75360 ) ;
#3243 = LINE ( 'NONE', #88963, #23243 ) ;
#3244 = CARTESIAN_POINT ( 'NONE',  ( -50.47208811125949524, -25.13340551635397091, 7.100116733165068972 ) ) ;
#3245 = DIRECTION ( 'NONE',  ( -0.000000000000000000, -1.000000000000000000, -0.000000000000000000 ) ) ;
#3246 = CARTESIAN_POINT ( 'NONE',  ( 10.74487964110493188, -6.376774720514429617, -24.99341878722455235 ) ) ;
#3247 = CARTESIAN_POINT ( 'NONE',  ( 13.57807927624399902, 15.74560944506941951, 11.49999999999999645 ) ) ;
#3248 = CARTESIAN_POINT ( 'NONE',  ( -7.586742644780859912, -6.376774720514413630, 19.78730719034165020 ) ) ;
#3249 = CARTESIAN_POINT ( 'NONE',  ( -51.24209892600672589, -25.23977856974979517, 3.738451043460532031 ) ) ;
#3250 = CARTESIAN_POINT ( 'NONE',  ( 12.37853024107498534, -19.16169124346054176, 11.49999999999999645 ) ) ;
#3251 = ORIENTED_EDGE ( 'NONE', *, *, #60230, .T. ) ;
#3252 = PLANE ( 'NONE',  #869 ) ;
#3253 = CARTESIAN_POINT ( 'NONE',  ( -91.52287095715006160, -23.47596703998600631, 11.44779298504228393 ) ) ;
#3254 = ORIENTED_EDGE ( 'NONE', *, *, #44216, .F. ) ;
#3255 = CARTESIAN_POINT ( 'NONE',  ( 19.74221769882431587, -4.499994434135383692, 11.49999999999998934 ) ) ;
#3256 = B_SPLINE_CURVE_WITH_KNOTS ( 'NONE', 3,
 ( #12824, #29054, #98558, #21924, #37173, #5721 ),
 .UNSPECIFIED., .F., .F.,
 ( 4, 2, 4 ),
 ( 1.570755371634376281E-05, 0.001396183895866091223, 0.002776660238015838614 ),
 .UNSPECIFIED. ) ;
#3257 = CARTESIAN_POINT ( 'NONE',  ( -106.5228709571500758, -23.48786465467242479, 11.44779295918253936 ) ) ;
#3258 = CARTESIAN_POINT ( 'NONE',  ( -4.568292318365942073, -0.3587747205144265483, 30.06720597538392425 ) ) ;
#3259 = LINE ( 'NONE', #42325, #610 ) ;
#3260 = ORIENTED_EDGE ( 'NONE', *, *, #73861, .T. ) ;
#3261 = CARTESIAN_POINT ( 'NONE',  ( -79.26571160490151158, -25.31578574338585952, 5.001522333041759083 ) ) ;
#3262 = CARTESIAN_POINT ( 'NONE',  ( -10.11875734969026119, 3.519249775642004696, 30.51402280011862445 ) ) ;
#3263 = CARTESIAN_POINT ( 'NONE',  ( -19.61284664649099696, 3.773188449817356904, -1.500000000000002220 ) ) ;
#3264 = CARTESIAN_POINT ( 'NONE',  ( 19.44712688777480736, 7.780496645421295376, 11.49999999999999645 ) ) ;
#3265 = CARTESIAN_POINT ( 'NONE',  ( 9.032095062437601740, 5.965225279485574461, -28.07116626896318579 ) ) ;
#3266 = CARTESIAN_POINT ( 'NONE',  ( 31.79364159983995464, -6.475225279485573360, -11.59305536555894278 ) ) ;
#3267 = CARTESIAN_POINT ( 'NONE',  ( 6.148021820315829444, -21.18842874637755358, 11.49999999999998934 ) ) ;
#3268 = AXIS2_PLACEMENT_3D ( 'NONE', #4889, #11992, #20101 ) ;
#3269 = CARTESIAN_POINT ( 'NONE',  ( -46.92287095715006018, -23.47593901973090169, -1.443836447538997980 ) ) ;
#3270 = ORIENTED_EDGE ( 'NONE', *, *, #25349, .F. ) ;
#3271 = DIRECTION ( 'NONE',  ( 7.960204194457801640E-17, 1.000000000000000000, 0.000000000000000000 ) ) ;
#3272 = CARTESIAN_POINT ( 'NONE',  ( -122.5228709571500616, -29.50250243563736774, 8.947779886222134493 ) ) ;
#3273 = DIRECTION ( 'NONE',  ( 0.000000000000000000, 0.000000000000000000, 1.000000000000000000 ) ) ;
#3274 = CARTESIAN_POINT ( 'NONE',  ( -31.62287095715005236, -23.48783264082477729, -1.443836473390074149 ) ) ;
#3275 = EDGE_CURVE ( 'NONE', #84354, #40031, #28607, .T. ) ;
#3276 = ORIENTED_EDGE ( 'NONE', *, *, #73571, .T. ) ;
#3277 = VECTOR ( 'NONE', #21837, 1000.000000000000000 ) ;
#3278 = EDGE_CURVE ( 'NONE', #80847, #69272, #65793, .T. ) ;
#3279 = ORIENTED_EDGE ( 'NONE', *, *, #43912, .T. ) ;
#3280 = CARTESIAN_POINT ( 'NONE',  ( 14.43441819135929727, 5.965225279485572685, -28.36222020317710246 ) ) ;
#3281 = CARTESIAN_POINT ( 'NONE',  ( -84.92287095715006728, -23.47593901973090169, -1.443836447538996870 ) ) ;
#3282 = CARTESIAN_POINT ( 'NONE',  ( -51.52287095715008292, -23.47593901973090169, -1.443836447538997092 ) ) ;
#3283 = CARTESIAN_POINT ( 'NONE',  ( -17.91610926057384034, -10.00117247862695358, -1.500000000000002220 ) ) ;
#3284 = EDGE_CURVE ( 'NONE', #12764, #77091, #66299, .T. ) ;
#3285 = ORIENTED_EDGE ( 'NONE', *, *, #40044, .F. ) ;
#3286 = DIRECTION ( 'NONE',  ( -3.773278334453079030E-23, 0.9999999999976377785, 2.173523156925979128E-06 ) ) ;
#3287 = VECTOR ( 'NONE', #92886, 1000.000000000000114 ) ;
#3288 = CARTESIAN_POINT ( 'NONE',  ( -10.21507754268103696, 3.584423063163226786, 29.48076484700401068 ) ) ;
#3289 = CARTESIAN_POINT ( 'NONE',  ( 28.30015606816038698, -1.477225279485574028, -13.13501953239208575 ) ) ;
#3290 = CARTESIAN_POINT ( 'NONE',  ( -12.45998644600372884, -18.51849504856558681, 11.49999999999998934 ) ) ;
#3291 = ADVANCED_FACE ( 'NONE', ( #97709 ), #3883, .T. ) ;
#3292 = EDGE_CURVE ( 'NONE', #46565, #42982, #90597, .T. ) ;
#3293 = CARTESIAN_POINT ( 'NONE',  ( -0.1256113942619183910, -21.42386179076044073, -0.9709657327914303915 ) ) ;
#3294 = CARTESIAN_POINT ( 'NONE',  ( -32.99388727629348494, -25.12026506542017046, 2.831122744435439209 ) ) ;
#3295 = ORIENTED_EDGE ( 'NONE', *, *, #77382, .F. ) ;
#3296 = CARTESIAN_POINT ( 'NONE',  ( 4.784292611718075072, -3.316774720514426456, -25.54547254883186014 ) ) ;
#3297 = AXIS2_PLACEMENT_3D ( 'NONE', #70447, #69445, #85667 ) ;
#3298 = FACE_OUTER_BOUND ( 'NONE', #96131, .T. ) ;
#3299 = CIRCLE ( 'NONE', #16230, 0.3000000000000016542 ) ;
#3300 = B_SPLINE_CURVE_WITH_KNOTS ( 'NONE', 3,
 ( #63380, #70974, #48142, #1464, #25285, #17676 ),
 .UNSPECIFIED., .F., .F.,
 ( 4, 2, 4 ),
 ( 6.384118678612496926E-06, 0.001386860460828376286, 0.002767336802978140158 ),
 .UNSPECIFIED. ) ;
#3301 = CARTESIAN_POINT ( 'NONE',  ( 12.78316523911058944, -16.47895720935621711, -1.500000000000002220 ) ) ;
#3302 = VERTEX_POINT ( 'NONE', #12962 ) ;
#3304 = ORIENTED_EDGE ( 'NONE', *, *, #297, .F. ) ;
#3303 = CARTESIAN_POINT ( 'NONE',  ( -40.07618229162368095, -25.11765537177068808, 2.873089416660186135 ) ) ;
#3305 = ORIENTED_EDGE ( 'NONE', *, *, #42415, .F. ) ;
#3306 = AXIS2_PLACEMENT_3D ( 'NONE', #34145, #87414, #40247 ) ;
#3307 = LINE ( 'NONE', #27121, #6581 ) ;
#3308 = CARTESIAN_POINT ( 'NONE',  ( 20.75205275252385206, -3.532026382766447536, -1.500000000000002220 ) ) ;
#3309 = VECTOR ( 'NONE', #55680, 1000.000000000000114 ) ;
#3310 = ORIENTED_EDGE ( 'NONE', *, *, #42800, .F. ) ;
#3311 = LINE ( 'NONE', #59082, #12197 ) ;
#3312 = CARTESIAN_POINT ( 'NONE',  ( -53.52287095715006160, -23.95044443724992789, 10.65354141964649415 ) ) ;
#3313 = CARTESIAN_POINT ( 'NONE',  ( -120.5553384622658939, -24.15602025860899360, 10.28564288303534902 ) ) ;
#3314 = FACE_OUTER_BOUND ( 'NONE', #86391, .T. ) ;
#3315 = CARTESIAN_POINT ( 'NONE',  ( -83.62287095715005592, -23.47593901973091235, -1.443836447539004642 ) ) ;
#3316 = CARTESIAN_POINT ( 'NONE',  ( 21.03555826204448209, -5.341079136732027166, -1.500000000000002220 ) ) ;
#3317 = CARTESIAN_POINT ( 'NONE',  ( -81.04964064216432007, -25.24759771266412045, 6.946763360114873720 ) ) ;
#3319 = ORIENTED_EDGE ( 'NONE', *, *, #51851, .T. ) ;
#3318 = CARTESIAN_POINT ( 'NONE',  ( 2.321567282091853812, -22.14299765706108403, 11.49999999999999645 ) ) ;
#3320 = CARTESIAN_POINT ( 'NONE',  ( -51.50851365739161736, -25.31441895692774935, 5.995695726151790694 ) ) ;
#3321 = DIRECTION ( 'NONE',  ( 0.000000000000000000, 0.000000000000000000, -1.000000000000000000 ) ) ;
#3322 = EDGE_CURVE ( 'NONE', #47722, #46585, #35326, .T. ) ;
#3323 = CARTESIAN_POINT ( 'NONE',  ( -69.62287095715005592, -23.48786465467241058, 11.44779295918254824 ) ) ;
#3324 = ORIENTED_EDGE ( 'NONE', *, *, #76805, .F. ) ;
#3326 = ORIENTED_EDGE ( 'NONE', *, *, #2145, .F. ) ;
#3325 = CARTESIAN_POINT ( 'NONE',  ( -76.62287095715009855, -24.50216790748098816, 0.6166512839513735855 ) ) ;
#3327 = EDGE_CURVE ( 'NONE', #74882, #1888, #73879, .T. ) ;
#3328 = VERTEX_POINT ( 'NONE', #97213 ) ;
#3329 = CARTESIAN_POINT ( 'NONE',  ( -27.96875734969026084, -6.475225279485573360, -0.08597719988137648983 ) ) ;
#3330 = CARTESIAN_POINT ( 'NONE',  ( -107.5228709571500758, -24.65952944569304961, 1.056160979905704123 ) ) ;
#3331 = CARTESIAN_POINT ( 'NONE',  ( -126.5228709571500616, -24.64965694238408034, 8.947790433994189385 ) ) ;
#3332 = ORIENTED_EDGE ( 'NONE', *, *, #70416, .F. ) ;
#3333 = LINE ( 'NONE', #81437, #50361 ) ;
#3334 = CARTESIAN_POINT ( 'NONE',  ( 15.48037617655995923, 16.25473645317415361, -1.500000000000002220 ) ) ;
#3335 = VERTEX_POINT ( 'NONE', #59160 ) ;
#3336 = CARTESIAN_POINT ( 'NONE',  ( 31.55236408230781819, 6.376774720514426953, 19.84760796525321780 ) ) ;
#3337 = CARTESIAN_POINT ( 'NONE',  ( -101.5888304102239630, -24.35071581493543746, 9.817618358456027039 ) ) ;
#3338 = CARTESIAN_POINT ( 'NONE',  ( 9.464509667904351886, 3.316774720514128028, -27.03659963365196717 ) ) ;
#3339 = DIRECTION ( 'NONE',  ( 1.000000000000000000, 0.000000000000000000, 0.000000000000000000 ) ) ;
#3341 = ADVANCED_FACE ( 'NONE', ( #29200 ), #35817, .T. ) ;
#3340 = CARTESIAN_POINT ( 'NONE',  ( -63.93323764602512682, -24.26827793580486059, 9.960784317162946877 ) ) ;
#3342 = CARTESIAN_POINT ( 'NONE',  ( 19.39309126630920588, -2.812899550206792831, 11.49999999999998934 ) ) ;
#3343 = CARTESIAN_POINT ( 'NONE',  ( -59.55620429048337883, -24.65952944569304961, 1.056160979905694797 ) ) ;
#3344 = ORIENTED_EDGE ( 'NONE', *, *, #13484, .T. ) ;
#3345 = CARTESIAN_POINT ( 'NONE',  ( -18.53595284743415661, 10.95218985133829825, -1.500000000000002220 ) ) ;
#3346 = CARTESIAN_POINT ( 'NONE',  ( -60.62287095715004881, -23.48783264082478439, -1.443836473390068820 ) ) ;
#3347 = CARTESIAN_POINT ( 'NONE',  ( -71.28784841027113828, -25.12218989441461048, 6.387103282270394367 ) ) ;
#3348 = CARTESIAN_POINT ( 'NONE',  ( 32.25183987940364005, 5.965225279485572685, 2.026414261721653176 ) ) ;
#3350 = ADVANCED_FACE ( 'NONE', ( #28203 ), #89109, .F. ) ;
#3349 = AXIS2_PLACEMENT_3D ( 'NONE', #13992, #44969, #99227 ) ;
#3351 = CARTESIAN_POINT ( 'NONE',  ( -77.62287095715007013, -23.48786465467241413, 11.44779295918254469 ) ) ;
#3352 = CARTESIAN_POINT ( 'NONE',  ( -16.74478417649319084, -15.65585335247391896, -1.500000000000002220 ) ) ;
#3353 = APPROVAL_DATE_TIME ( #72852, #48847 ) ;
#3354 = DIRECTION ( 'NONE',  ( 0.000000000000000000, -2.173523156925979552E-06, 0.9999999999976378895 ) ) ;
#3355 = DIRECTION ( 'NONE',  ( 1.000000000000000000, 3.773278334444166432E-23, 8.201307841325785021E-29 ) ) ;
#3356 = CARTESIAN_POINT ( 'NONE',  ( -16.07871291144651593, -12.00523380332558965, 11.49999999999999645 ) ) ;
#3357 = CARTESIAN_POINT ( 'NONE',  ( -109.7637679387061809, -25.28814089820113153, 2.928686338884283202 ) ) ;
#3358 = DIRECTION ( 'NONE',  ( 0.000000000000000000, 0.000000000000000000, -1.000000000000000000 ) ) ;
#3359 = B_SPLINE_CURVE_WITH_KNOTS ( 'NONE', 3,
 ( #80227, #57414, #34563, #58895, #4615, #35562 ),
 .UNSPECIFIED., .F., .F.,
 ( 4, 2, 4 ),
 ( 1.570887131794333942E-05, 0.001396322306279761073, 0.002776935741241578874 ),
 .UNSPECIFIED. ) ;
#3360 = DIRECTION ( 'NONE',  ( 0.000000000000000000, 0.000000000000000000, -1.000000000000000000 ) ) ;
#3361 = CARTESIAN_POINT ( 'NONE',  ( -82.52287095715006160, -29.50248528299804818, 1.056150453629038477 ) ) ;
#3362 = CARTESIAN_POINT ( 'NONE',  ( -96.22287095715006444, -23.47596703998600631, 11.44779298504227860 ) ) ;
#3363 = CARTESIAN_POINT ( 'NONE',  ( -7.754168067426306266, 18.25094163199162622, -1.500000000000002220 ) ) ;
#3364 = CARTESIAN_POINT ( 'NONE',  ( -2.188401442307694289, -5.876774720514411854, 19.46153846153846700 ) ) ;
#3365 = CARTESIAN_POINT ( 'NONE',  ( -14.27994306655487300, -13.59162091658854798, -1.500000000000002220 ) ) ;
#3366 = CARTESIAN_POINT ( 'NONE',  ( -75.58953762381673869, -23.48786465467241058, 11.44779295918254647 ) ) ;
#3367 = AXIS2_PLACEMENT_3D ( 'NONE', #15901, #24517, #94031 ) ;
#3368 = DATE_AND_TIME ( #18067, #11805 ) ;
#3369 = AXIS2_PLACEMENT_3D ( 'NONE', #15600, #24712, #77492 ) ;
#3370 = CARTESIAN_POINT ( 'NONE',  ( -57.52287095715005449, -23.47596703998600631, 11.44779298504228926 ) ) ;
#3371 = DIRECTION ( 'NONE',  ( 0.000000000000000000, 0.000000000000000000, 1.000000000000000000 ) ) ;
#3372 = CARTESIAN_POINT ( 'NONE',  ( 18.07347782881280907, 9.871946371954690491, 11.49999999999999645 ) ) ;
#3373 = CARTESIAN_POINT ( 'NONE',  ( -42.62287095715007013, -23.96127896941632685, -0.6493128931037909224 ) ) ;
#3374 = AXIS2_PLACEMENT_3D ( 'NONE', #50621, #18660, #49635 ) ;
#3375 = CARTESIAN_POINT ( 'NONE',  ( -21.51096707683950626, -7.176001652309477841, 11.49999999999999645 ) ) ;
#3376 = ORIENTED_EDGE ( 'NONE', *, *, #22735, .F. ) ;
#3377 = CARTESIAN_POINT ( 'NONE',  ( -126.5562042904833930, -23.47593901973091235, -1.443836447538995760 ) ) ;
#3378 = CARTESIAN_POINT ( 'NONE',  ( -50.60192890204033489, -25.31221690582124140, 4.716031646587921067 ) ) ;
#3379 = CARTESIAN_POINT ( 'NONE',  ( -110.6228709571500559, -24.51254535404253687, 9.355368623467654743 ) ) ;
#3380 = CARTESIAN_POINT ( 'NONE',  ( -56.52287095715009713, -23.96177878511308990, 10.65340807706330217 ) ) ;
#3381 = ORIENTED_EDGE ( 'NONE', *, *, #54926, .T. ) ;
#3382 = DIRECTION ( 'NONE',  ( 0.000000000000000000, -0.000000000000000000, -1.000000000000000000 ) ) ;
#3383 = B_SPLINE_CURVE_WITH_KNOTS ( 'NONE', 3,
 ( #85212, #32431, #56290, #30925 ),
 .UNSPECIFIED., .F., .F.,
 ( 4, 4 ),
 ( 0.000000000000000000, 0.0001000000000000167422 ),
 .UNSPECIFIED. ) ;
#3384 = CARTESIAN_POINT ( 'NONE',  ( -15.12447472116105729, 17.10960193589383849, -1.500000000000002220 ) ) ;
#3385 = CARTESIAN_POINT ( 'NONE',  ( -100.5228709571500758, -23.47593901973090524, -1.443836447538996648 ) ) ;
#3386 = DIRECTION ( 'NONE',  ( -1.000000000000000000, 0.000000000000000000, 0.000000000000000000 ) ) ;
#3387 = DIRECTION ( 'NONE',  ( -3.491481338843133355E-15, 1.000000000000000000, -2.352173255807804438E-16 ) ) ;
#3388 = CARTESIAN_POINT ( 'NONE',  ( -22.32441756149717094, -2.617931739244098388, 11.49999999999999645 ) ) ;
#3389 = ORIENTED_EDGE ( 'NONE', *, *, #57873, .F. ) ;
#3390 = B_SPLINE_CURVE_WITH_KNOTS ( 'NONE', 3,
 ( #36995, #28885, #98887, #90787 ),
 .UNSPECIFIED., .F., .F.,
 ( 4, 4 ),
 ( 9.399644415434986408E-16, 2.036287925413292384E-05 ),
 .UNSPECIFIED. ) ;
#3391 = CARTESIAN_POINT ( 'NONE',  ( -43.64074243423868182, -24.15543982623907127, -0.2315651400026568496 ) ) ;
#3392 = CARTESIAN_POINT ( 'NONE',  ( 21.10488023177059347, -6.046698511884514460, -1.500000000000002220 ) ) ;
#3393 = CARTESIAN_POINT ( 'NONE',  ( 32.76111974776238611, 3.316774720514426900, -3.850861272813261849 ) ) ;
#3394 = CARTESIAN_POINT ( 'NONE',  ( 30.77564450787169648, -4.772774720514425972, -9.689394075852828081 ) ) ;
#3395 = CARTESIAN_POINT ( 'NONE',  ( -70.16027724210108829, -25.03456847279097630, 7.555221055302367539 ) ) ;
#3396 = ORIENTED_EDGE ( 'NONE', *, *, #24926, .F. ) ;
#3397 = CARTESIAN_POINT ( 'NONE',  ( -92.62287095715005592, -29.50248528299804818, 1.056150453629040253 ) ) ;
#3398 = CARTESIAN_POINT ( 'NONE',  ( -10.75273025779354263, -5.876774720514426953, 16.96478738960562893 ) ) ;
#3399 = ORIENTED_EDGE ( 'NONE', *, *, #68320, .T. ) ;
#3400 = CARTESIAN_POINT ( 'NONE',  ( -54.62797921530123801, -24.51419770103157347, 9.386484678747176957 ) ) ;
#3401 = EDGE_CURVE ( 'NONE', #87031, #642, #60169, .T. ) ;
#3402 = CARTESIAN_POINT ( 'NONE',  ( 20.49162120248849561, -0.4999214236376636200, -1.500000000000002220 ) ) ;
#3403 = VERTEX_POINT ( 'NONE', #81990 ) ;
#3404 = ORIENTED_EDGE ( 'NONE', *, *, #17334, .F. ) ;
#3405 = ORIENTED_EDGE ( 'NONE', *, *, #74947, .F. ) ;
#3406 = DIRECTION ( 'NONE',  ( 0.3133898629642186684, 7.885106708985488048E-16, -0.9496245541219267006 ) ) ;
#3407 = CARTESIAN_POINT ( 'NONE',  ( 8.286623624103266097E-13, -23.05000000000000426, 11.49999999999998934 ) ) ;
#3408 = LINE ( 'NONE', #40952, #81137 ) ;
#3409 = CARTESIAN_POINT ( 'NONE',  ( -12.25758032491116367, 16.21837406056298292, -1.500000000000002220 ) ) ;
#3410 = EDGE_CURVE ( 'NONE', #57091, #76361, #87920, .T. ) ;
#3411 = ORIENTED_EDGE ( 'NONE', *, *, #42967, .F. ) ;
#3412 = CARTESIAN_POINT ( 'NONE',  ( -1.044871794871793602, -5.876774720514418071, 20.44941907051282115 ) ) ;
#3413 = CARTESIAN_POINT ( 'NONE',  ( -29.66017770924821306, -23.66242766326485736, 11.05961561336856569 ) ) ;
#3414 = EDGE_CURVE ( 'NONE', #65188, #68864, #89603, .T. ) ;
#3415 = CARTESIAN_POINT ( 'NONE',  ( -105.5894920141959687, -24.52300882791530157, 0.6510814631126371488 ) ) ;
#3416 = CARTESIAN_POINT ( 'NONE',  ( -70.70237668956666255, -25.25855373138085014, 7.522646402401707455 ) ) ;
#3417 = ORIENTED_EDGE ( 'NONE', *, *, #32360, .F. ) ;
#3418 = CARTESIAN_POINT ( 'NONE',  ( -27.68651082257922980, -24.76880854176360813, 2.274903372879362617 ) ) ;
#3419 = CARTESIAN_POINT ( 'NONE',  ( -99.52287095715011844, -23.48783264083466449, -1.443836473374706442 ) ) ;
#3420 = EDGE_CURVE ( 'NONE', #57878, #62448, #50054, .T. ) ;
#3421 = ORIENTED_EDGE ( 'NONE', *, *, #59697, .F. ) ;
#3422 = EDGE_CURVE ( 'NONE', #60099, #45760, #7344, .T. ) ;
#3423 = CARTESIAN_POINT ( 'NONE',  ( -2.730994233912177549, 20.60462238790213618, 11.49999999999998934 ) ) ;
#3424 = TOROIDAL_SURFACE ( 'NONE', #21267, 19.00000000000000355, 1.000000000000000000 ) ;
#3425 = ORIENTED_EDGE ( 'NONE', *, *, #71491, .F. ) ;
#3427 = EDGE_LOOP ( 'NONE', ( #44782, #68483, #92247, #41809 ) ) ;
#3426 = CARTESIAN_POINT ( 'NONE',  ( -39.45233922144024064, -25.28612432382913511, 4.312181222606807474 ) ) ;
#3428 = DIRECTION ( 'NONE',  ( -3.773278334453079618E-23, 0.9999999999976377785, 2.173523156925979975E-06 ) ) ;
#3429 = CARTESIAN_POINT ( 'NONE',  ( 32.59332756141814258, -2.682774720514426559, -11.41404606144462086 ) ) ;
#3430 = ORIENTED_EDGE ( 'NONE', *, *, #44468, .F. ) ;
#3431 = ORIENTED_EDGE ( 'NONE', *, *, #5842, .F. ) ;
#3432 = DIRECTION ( 'NONE',  ( -3.773278334453079618E-23, 0.9999999999976377785, 2.173523156925979975E-06 ) ) ;
#3433 = DIRECTION ( 'NONE',  ( 1.000000000000000000, 3.773278334444166432E-23, 8.201307841325785021E-29 ) ) ;
#3434 = CARTESIAN_POINT ( 'NONE',  ( -71.30457154551152144, -25.24515236888725056, 6.209207408895393243 ) ) ;
#3436 = VERTEX_POINT ( 'NONE', #48301 ) ;
#3435 = CARTESIAN_POINT ( 'NONE',  ( -20.36895902721504825, -8.506870616244709637, 11.49999999999999645 ) ) ;
#3437 = DIRECTION ( 'NONE',  ( 0.000000000000000000, -0.7071067811865525687, 0.7071067811865425767 ) ) ;
#3438 = CARTESIAN_POINT ( 'NONE',  ( -19.18631400275845422, -11.98935526391121087, 11.49999999999998934 ) ) ;
#3440 = VERTEX_POINT ( 'NONE', #71635 ) ;
#3439 = CYLINDRICAL_SURFACE ( 'NONE', #57196, 4.080000000000000071 ) ;
#3441 = AXIS2_PLACEMENT_3D ( 'NONE', #41393, #25661, #56633 ) ;
#3442 = ORIENTED_EDGE ( 'NONE', *, *, #25021, .T. ) ;
#3443 = APPROVAL_PERSON_ORGANIZATION ( #80453, #66842, #96185 ) ;
#3444 = PLANE ( 'NONE',  #1305 ) ;
#3445 = DIRECTION ( 'NONE',  ( 0.8788171126619707119, -0.4771587602595986910, 6.123031769111886291E-17 ) ) ;
#3446 = VERTEX_POINT ( 'NONE', #29695 ) ;
#3447 = CARTESIAN_POINT ( 'NONE',  ( 9.297385241821217505, 19.04214385377821017, -1.500000000000002220 ) ) ;
#3448 = CARTESIAN_POINT ( 'NONE',  ( -78.97085663747836293, -25.03138025248980725, 6.301136368351477834 ) ) ;
#3449 = CARTESIAN_POINT ( 'NONE',  ( -7.326695514711824231, -6.376774720514417183, 20.26757654895259719 ) ) ;
#3450 = CARTESIAN_POINT ( 'NONE',  ( -41.18130138025338738, -25.29969733389206965, 5.386376836069856289 ) ) ;
#3451 = CARTESIAN_POINT ( 'NONE',  ( 17.16062296631688255, 14.07911611715085876, -1.500000000000002220 ) ) ;
#3452 = CARTESIAN_POINT ( 'NONE',  ( -49.44333826525905806, -25.13941437307980920, 7.288210270445980576 ) ) ;
#3453 = EDGE_LOOP ( 'NONE', ( #42380, #36140, #60518, #70811 ) ) ;
#3454 = DIRECTION ( 'NONE',  ( -1.000000000000000000, 0.000000000000000000, 0.000000000000000000 ) ) ;
#3455 = CARTESIAN_POINT ( 'NONE',  ( 29.73860345376319003, -14.82721238576461609, -4.021180035027960287 ) ) ;
#3456 = CARTESIAN_POINT ( 'NONE',  ( -40.80745846450592040, -25.11777459330632922, 2.873756378189262772 ) ) ;
#3457 = PLANE ( 'NONE',  #8103 ) ;
#3458 = CARTESIAN_POINT ( 'NONE',  ( 18.23270504744370868, -6.907985942191454676, 11.49999999999998934 ) ) ;
#3459 = CARTESIAN_POINT ( 'NONE',  ( 21.40653236543258231, -1.377805879665675803, 11.49999999999998934 ) ) ;
#3460 = CARTESIAN_POINT ( 'NONE',  ( -27.12458168156152638, -24.57999515849961369, 1.715463076443914936 ) ) ;
#3461 = CARTESIAN_POINT ( 'NONE',  ( -107.5895376238167387, -23.48786465467241769, 11.44779295918253936 ) ) ;
#3462 = DIRECTION ( 'NONE',  ( -1.000000000000000000, -3.773278334444166432E-23, -8.201307841325785021E-29 ) ) ;
#3463 = EDGE_CURVE ( 'NONE', #3899, #39432, #29865, .T. ) ;
#3464 = CARTESIAN_POINT ( 'NONE',  ( -12.29745307268338195, -19.16510367807413218, -1.500000000000002220 ) ) ;
#3465 = EDGE_CURVE ( 'NONE', #95862, #42749, #60665, .T. ) ;
#3466 = CARTESIAN_POINT ( 'NONE',  ( -102.5955334420205105, -23.73766607897671932, -1.055555164236430477 ) ) ;
#3467 = CARTESIAN_POINT ( 'NONE',  ( -24.90875734969025501, 3.316774720514426456, 26.43402280011862615 ) ) ;
#3468 = CARTESIAN_POINT ( 'NONE',  ( -12.53609265798794681, -15.47265773855268378, 11.49999999999999645 ) ) ;
#3469 = CARTESIAN_POINT ( 'NONE',  ( -31.52287095715004028, -23.94994826722564696, -0.6494450866342755813 ) ) ;
#3470 = CARTESIAN_POINT ( 'NONE',  ( -128.5228709571500474, -24.50321055353803601, 9.387540953477504502 ) ) ;
#3471 = LINE ( 'NONE', #19665, #31043 ) ;
#3472 = ORIENTED_EDGE ( 'NONE', *, *, #86762, .T. ) ;
#3473 = CARTESIAN_POINT ( 'NONE',  ( -25.55988077703415939, -24.90308938919016768, 4.202771167367211902 ) ) ;
#3474 = DIRECTION ( 'NONE',  ( 2.352173255807804438E-16, -2.352173255807796056E-16, -1.000000000000000000 ) ) ;
#3475 = CARTESIAN_POINT ( 'NONE',  ( 8.489507321284875729, -19.98171680480944445, -1.500000000000002220 ) ) ;
#3476 = CARTESIAN_POINT ( 'NONE',  ( -51.88092039732551086, -25.21678524435695223, 6.552750624006524305 ) ) ;
#3477 = CARTESIAN_POINT ( 'NONE',  ( -6.365771329251782795, -18.49506561991874065, -1.500000000000002220 ) ) ;
#3478 = DIRECTION ( 'NONE',  ( 0.7689940216596069522, 5.365801633547218220E-16, -0.6392559695863496705 ) ) ;
#3479 = ORIENTED_EDGE ( 'NONE', *, *, #82080, .F. ) ;
#3480 = APPROVAL_DATE_TIME ( #72992, #54338 ) ;
#3481 = CARTESIAN_POINT ( 'NONE',  ( -60.62287095715003460, -24.83620972994591014, 8.398175272781363887 ) ) ;
#3482 = CARTESIAN_POINT ( 'NONE',  ( -8.052747710315523832, 18.77774781879659116, 11.49999999999999645 ) ) ;
#3483 = DIRECTION ( 'NONE',  ( -1.000000000000000000, -3.491481338843133355E-15, -2.352173255807796056E-16 ) ) ;
#3484 = B_SPLINE_CURVE_WITH_KNOTS ( 'NONE', 3,
 ( #97823, #36927, #13579, #66902, #20695, #44547, #19693, #96830 ),
 .UNSPECIFIED., .F., .F.,
 ( 4, 2, 2, 4 ),
 ( -0.001240355328176650195, -0.0002398155169397891452, 0.0007607242942970719041, 0.002761803916770794003 ),
 .UNSPECIFIED. ) ;
#3485 = AXIS2_PLACEMENT_3D ( 'NONE', #3361, #57639, #11944 ) ;
#3486 = CARTESIAN_POINT ( 'NONE',  ( -89.52287095715011844, -23.94994826722565406, -0.6494450866342716955 ) ) ;
#3487 = ORIENTED_EDGE ( 'NONE', *, *, #33526, .T. ) ;
#3488 = CARTESIAN_POINT ( 'NONE',  ( -53.22287095715005023, -23.47596703998600276, 11.44779298504227860 ) ) ;
#3489 = DIRECTION ( 'NONE',  ( -3.773278334444167608E-23, 1.000000000000000000, 0.000000000000000000 ) ) ;
#3490 = CARTESIAN_POINT ( 'NONE',  ( -63.52287095715006160, -29.50250243563736774, 8.947779886222145151 ) ) ;
#3491 = CARTESIAN_POINT ( 'NONE',  ( -56.52287095715005449, -23.47593901973090169, -1.443836447538996870 ) ) ;
#3492 = VERTEX_POINT ( 'NONE', #76842 ) ;
#3493 = CARTESIAN_POINT ( 'NONE',  ( -66.58005638815387783, -24.66019654487199375, 8.947790411086119278 ) ) ;
#3494 = AXIS2_PLACEMENT_3D ( 'NONE', #9812, #35158, #18426 ) ;
#3495 = CARTESIAN_POINT ( 'NONE',  ( -6.529369910325518944, -22.02198592821369516, 11.49999999999999645 ) ) ;
#3496 = CARTESIAN_POINT ( 'NONE',  ( 5.860688371469950475, 21.97560254587667217, -1.500000000000002220 ) ) ;
#3497 = CARTESIAN_POINT ( 'NONE',  ( 4.332134589405623792, -6.376774720514427841, 21.69242924468134959 ) ) ;
#3498 = CARTESIAN_POINT ( 'NONE',  ( -91.58953762381673869, -23.48786465467241769, 11.44779295918254114 ) ) ;
#3499 = CARTESIAN_POINT ( 'NONE',  ( -90.50269887387773338, -24.73486907724917927, 1.287355809206966573 ) ) ;
#3500 = LOCAL_TIME ( 0, 54, 15.00000000000000000, #49018 ) ;
#3501 = DIRECTION ( 'NONE',  ( -1.084136044942898696E-16, -0.000000000000000000, 1.000000000000000000 ) ) ;
#3502 = CARTESIAN_POINT ( 'NONE',  ( -27.25988310792305214, 0.3587747205144265483, 30.32664379231667695 ) ) ;
#3503 = CARTESIAN_POINT ( 'NONE',  ( 6.672210613628693388, 20.84999943921648935, -1.500000000000002220 ) ) ;
#3504 = CARTESIAN_POINT ( 'NONE',  ( -74.52287095715009002, -23.94994826722564696, -0.6494450866342713624 ) ) ;
#3505 = CARTESIAN_POINT ( 'NONE',  ( -48.91427541414667957, -25.28859040982994344, 5.814958163393877832 ) ) ;
#3506 = CARTESIAN_POINT ( 'NONE',  ( 31.48454476783385658, 4.132774720514426292, -1.134026763942596494 ) ) ;
#3507 = CARTESIAN_POINT ( 'NONE',  ( -96.52287095715011844, -24.33927499327855770, 9.819080762295806508 ) ) ;
#3508 = ORIENTED_EDGE ( 'NONE', *, *, #67495, .F. ) ;
#3509 = CARTESIAN_POINT ( 'NONE',  ( 8.094744887094867281, -18.73235182305680624, -1.500000000000002220 ) ) ;
#3510 = ORIENTED_EDGE ( 'NONE', *, *, #25660, .T. ) ;
#3511 = EDGE_LOOP ( 'NONE', ( #41596, #12392, #54523, #87657 ) ) ;
#3512 = ORIENTED_EDGE ( 'NONE', *, *, #77043, .T. ) ;
#3513 = CARTESIAN_POINT ( 'NONE',  ( -4.971178678486217528, -22.47594730032828281, 11.49999999999998934 ) ) ;
#3514 = PLANE ( 'NONE',  #94019 ) ;
#3515 = CARTESIAN_POINT ( 'NONE',  ( 16.68447708738676383, -11.30049470069299922, -1.500000000000002220 ) ) ;
#3516 = ORIENTED_EDGE ( 'NONE', *, *, #82014, .F. ) ;
#3517 = DIRECTION ( 'NONE',  ( 0.000000000000000000, 0.000000000000000000, -1.000000000000000000 ) ) ;
#3518 = CARTESIAN_POINT ( 'NONE',  ( -29.49875734969026198, -5.965225279485572685, 7.870022800118625206 ) ) ;
#3519 = CARTESIAN_POINT ( 'NONE',  ( -95.62462609076078479, -24.92564183028979841, 1.928384488918254425 ) ) ;
#3520 = FACE_OUTER_BOUND ( 'NONE', #98848, .T. ) ;
#3522 = ORIENTED_EDGE ( 'NONE', *, *, #92533, .T. ) ;
#3521 = CARTESIAN_POINT ( 'NONE',  ( 19.99361899508246765, -7.638522130635823082, 11.49999999999999645 ) ) ;
#3523 = CARTESIAN_POINT ( 'NONE',  ( 9.552245033349362461E-16, 23.99999999999999645, 2.100000000000000089 ) ) ;
#3524 = ADVANCED_FACE ( 'NONE', ( #54047 ), #1629, .F. ) ;
#3525 = ORIENTED_EDGE ( 'NONE', *, *, #4139, .T. ) ;
#3526 = CARTESIAN_POINT ( 'NONE',  ( -9.338385371603758145, -20.21602636099808237, 11.49999999999998934 ) ) ;
#3527 = EDGE_CURVE ( 'NONE', #57212, #93999, #38299, .T. ) ;
#3528 = CARTESIAN_POINT ( 'NONE',  ( -9.011640028862021978, 18.61544202926687674, -1.500000000000002220 ) ) ;
#3529 = VERTEX_POINT ( 'NONE', #53048 ) ;
#3530 = AXIS2_PLACEMENT_3D ( 'NONE', #42623, #19257, #58346 ) ;
#3531 = B_SPLINE_CURVE_WITH_KNOTS ( 'NONE', 3,
 ( #77455, #87083, #63269, #62261, #17572, #7955 ),
 .UNSPECIFIED., .F., .F.,
 ( 4, 2, 4 ),
 ( 1.570755371633915156E-05, 0.001396183895866087103, 0.002776660238015835145 ),
 .UNSPECIFIED. ) ;
#3532 = DIRECTION ( 'NONE',  ( 0.000000000000000000, 1.000000000000000000, 0.000000000000000000 ) ) ;
#3533 = EDGE_LOOP ( 'NONE', ( #37244, #89735, #94262, #12625 ) ) ;
#3534 = DIRECTION ( 'NONE',  ( 0.000000000000000000, -1.000000000000000000, 0.000000000000000000 ) ) ;
#3535 = EDGE_LOOP ( 'NONE', ( #37942, #11616, #1415, #51184 ) ) ;
#3536 = CARTESIAN_POINT ( 'NONE',  ( 282.9764569301858046, -3.316774720514426900, 20.79159422840526616 ) ) ;
#3537 = CARTESIAN_POINT ( 'NONE',  ( 19.40473180639871131, -7.901900427366274293, -1.500000000000002220 ) ) ;
#3538 = ADVANCED_FACE ( 'NONE', ( #6855 ), #78712, .T. ) ;
#3539 = CARTESIAN_POINT ( 'NONE',  ( -19.20277006422315225, 10.48866939257135833, 11.49999999999999645 ) ) ;
#3540 = CARTESIAN_POINT ( 'NONE',  ( -26.92109862195654202, -24.77993744210030158, 7.359062092904308017 ) ) ;
#3541 = CARTESIAN_POINT ( 'NONE',  ( 17.90692129536829924, 13.62026984716248101, -1.500000000000002220 ) ) ;
#3542 = CARTESIAN_POINT ( 'NONE',  ( 7.003190781191628744, -19.75400906848480176, 11.49999999999998934 ) ) ;
#3543 = CARTESIAN_POINT ( 'NONE',  ( -26.18848782724420232, -24.88148942182913004, 5.990951222462844505 ) ) ;
#3544 = CARTESIAN_POINT ( 'NONE',  ( -108.8968792378191921, -25.06732983082694943, 7.447789526168955732 ) ) ;
#3545 = CARTESIAN_POINT ( 'NONE',  ( -70.52287095715007581, -23.47596703998600631, 11.44779298504228748 ) ) ;
#3546 = ORIENTED_EDGE ( 'NONE', *, *, #17964, .F. ) ;
#3547 = EDGE_LOOP ( 'NONE', ( #30552, #92804, #78996, #78974 ) ) ;
#3548 = ORIENTED_EDGE ( 'NONE', *, *, #28502, .F. ) ;
#3549 = VECTOR ( 'NONE', #79070, 1000.000000000000114 ) ;
#3550 = CARTESIAN_POINT ( 'NONE',  ( -52.56018645129599065, -23.73766607897671577, -1.055555164236436472 ) ) ;
#3551 = EDGE_LOOP ( 'NONE', ( #23914, #5095 ) ) ;
#3552 = CARTESIAN_POINT ( 'NONE',  ( -17.67684169981329845, 12.20363403927300183, -1.500000000000002220 ) ) ;
#3553 = ORIENTED_EDGE ( 'NONE', *, *, #97201, .F. ) ;
#3554 = DIRECTION ( 'NONE',  ( -1.000000000000000000, -3.773278334444166432E-23, -8.201307841325785021E-29 ) ) ;
#3555 = CARTESIAN_POINT ( 'NONE',  ( 2.841100885065937387, 20.89556961663114265, 11.49999999999998934 ) ) ;
#3556 = CARTESIAN_POINT ( 'NONE',  ( -30.53009340616916134, -23.47882956801885612, 11.44779287168131710 ) ) ;
#3557 = CARTESIAN_POINT ( 'NONE',  ( 33.00535138976609062, -6.376774720514426953, -12.97242311383962310 ) ) ;
#3558 = CARTESIAN_POINT ( 'NONE',  ( 24.71017632900190719, -5.356774720514427379, 1.647607965253213624 ) ) ;
#3559 = B_SPLINE_CURVE_WITH_KNOTS ( 'NONE', 3,
 ( #48769, #65010, #71099, #95926 ),
 .UNSPECIFIED., .F., .F.,
 ( 4, 4 ),
 ( 2.775557561562891043E-17, 9.999999999998898659E-05 ),
 .UNSPECIFIED. ) ;
#3560 = FACE_OUTER_BOUND ( 'NONE', #10417, .T. ) ;
#3561 = CARTESIAN_POINT ( 'NONE',  ( -129.5900272792847829, -23.48786465467242124, 11.44779295918253936 ) ) ;
#3562 = CARTESIAN_POINT ( 'NONE',  ( 20.57837473233041692, -7.934362236255416256, -1.500000000000002220 ) ) ;
#3563 = ORIENTED_EDGE ( 'NONE', *, *, #48534, .T. ) ;
#3564 = CARTESIAN_POINT ( 'NONE',  ( -116.6251875513247853, -24.34968618360935366, 0.1864209137779019310 ) ) ;
#3565 = CC_DESIGN_APPROVAL ( #9079, ( #3711 ) ) ;
#3566 = DIRECTION ( 'NONE',  ( -1.000000000000000000, 0.000000000000000000, 0.000000000000000000 ) ) ;
#3567 = DIRECTION ( 'NONE',  ( 0.000000000000000000, 0.000000000000000000, -1.000000000000000000 ) ) ;
#3568 = ADVANCED_FACE ( 'NONE', ( #84973 ), #83793, .T. ) ;
#3569 = CARTESIAN_POINT ( 'NONE',  ( -26.94934480766437090, -25.03522359940358655, 4.936952632524853612 ) ) ;
#3570 = VECTOR ( 'NONE', #38406, 1000.000000000000114 ) ;
#3571 = B_SPLINE_CURVE_WITH_KNOTS ( 'NONE', 3,
 ( #70608, #32045, #41171, #63016, #64033, #94947 ),
 .UNSPECIFIED., .F., .F.,
 ( 4, 2, 4 ),
 ( 0.000000000000000000, 0.001380764517853247299, 0.002761529035706494599 ),
 .UNSPECIFIED. ) ;
#3572 = DIRECTION ( 'NONE',  ( 3.773278334444166432E-23, -1.000000000000000000, 0.000000000000000000 ) ) ;
#3573 = LOCAL_TIME ( 0, 54, 15.00000000000000000, #40270 ) ;
#3574 = PLANE ( 'NONE',  #93555 ) ;
#3575 = CARTESIAN_POINT ( 'NONE',  ( 15.73328655151706101, -14.44092690703295467, -1.500000000000002220 ) ) ;
#3576 = PLANE ( 'NONE',  #46616 ) ;
#3577 = CARTESIAN_POINT ( 'NONE',  ( -52.55620429048339304, -23.48783264082477729, -1.443836473390070596 ) ) ;
#3578 = ADVANCED_FACE ( 'NONE', ( #64049 ), #91078, .T. ) ;
#3579 = CARTESIAN_POINT ( 'NONE',  ( -19.69812919673063689, 5.965225279485592225, -22.00173861453435720 ) ) ;
#3580 = CARTESIAN_POINT ( 'NONE',  ( -81.48149462243459595, -25.23679622552714363, 6.293943003980942308 ) ) ;
#3581 = CARTESIAN_POINT ( 'NONE',  ( 14.59886444729927923, 17.24780449347180067, -1.500000000000002220 ) ) ;
#3582 = DIRECTION ( 'NONE',  ( 4.015954566446630556E-15, 1.000000000000000000, 1.297050502119899750E-15 ) ) ;
#3583 = ORIENTED_EDGE ( 'NONE', *, *, #76468, .F. ) ;
#3584 = CARTESIAN_POINT ( 'NONE',  ( 7.681304422638354445, 3.316774720514426900, -28.19747436301255661 ) ) ;
#3585 = CARTESIAN_POINT ( 'NONE',  ( -79.63359157097742980, -24.15543982623907127, -0.2315651400026654261 ) ) ;
#3586 = CARTESIAN_POINT ( 'NONE',  ( -9.637476322613308000, -17.25261889746210997, 11.49999999999999645 ) ) ;
#3587 = CARTESIAN_POINT ( 'NONE',  ( -123.6228709571500559, -24.66019654487200086, 8.947790411086117501 ) ) ;
#3588 = CARTESIAN_POINT ( 'NONE',  ( -67.51596563316087440, -23.73766607897670511, -1.055555164236457788 ) ) ;
#3589 = ORIENTED_EDGE ( 'NONE', *, *, #85474, .F. ) ;
#3590 = CARTESIAN_POINT ( 'NONE',  ( -79.11611000704996854, -25.21083105912962097, 3.409327675794633361 ) ) ;
#3591 = CARTESIAN_POINT ( 'NONE',  ( -28.98875734969026041, 5.965225279485572685, 15.62202280011862321 ) ) ;
#3592 = DIRECTION ( 'NONE',  ( -0.000000000000000000, -1.000000000000000000, -0.000000000000000000 ) ) ;
#3593 = CARTESIAN_POINT ( 'NONE',  ( -21.62496174240652991, 0.2022338437372764308, 11.49999999999998934 ) ) ;
#3594 = CARTESIAN_POINT ( 'NONE',  ( 7.150000000000004796, -2.000000000000001776, 24.00000000000000000 ) ) ;
#3595 = FACE_OUTER_BOUND ( 'NONE', #91005, .T. ) ;
#3596 = CARTESIAN_POINT ( 'NONE',  ( -10.21384395349174490, -3.316774720514427344, 29.49402280011862487 ) ) ;
#3597 = CARTESIAN_POINT ( 'NONE',  ( -80.93923948188344752, -25.05551947452300254, 7.504864834147113584 ) ) ;
#3598 = CARTESIAN_POINT ( 'NONE',  ( -12.15653940608521566, -15.58205587995076868, -1.500000000000002220 ) ) ;
#3599 = ORIENTED_EDGE ( 'NONE', *, *, #21854, .F. ) ;
#3600 = CARTESIAN_POINT ( 'NONE',  ( 9.769481717609929561, -17.74358427669893956, 11.49999999999999645 ) ) ;
#3601 = CARTESIAN_POINT ( 'NONE',  ( -7.603582339867426043, -5.876774720514417183, 19.86545874326176175 ) ) ;
#3602 = PRODUCT_DEFINITION ( 'UNKNOWN', '', #79677, #99657 ) ;
#3603 = VECTOR ( 'NONE', #60225, 1000.000000000000000 ) ;
#3604 = EDGE_LOOP ( 'NONE', ( #45589, #42466, #63252, #15716 ) ) ;
#3605 = CARTESIAN_POINT ( 'NONE',  ( -67.52287095715009002, -24.51387760970725083, 9.387446482453412955 ) ) ;
#3606 = CARTESIAN_POINT ( 'NONE',  ( 22.81105451610979173, 6.475225279485573360, -16.21691820600746681 ) ) ;
#3607 = CARTESIAN_POINT ( 'NONE',  ( -19.77875734969026311, -5.356774720514425603, 0.7300228001186309656 ) ) ;
#3608 = CARTESIAN_POINT ( 'NONE',  ( 5.271800844963591359, -3.316774720514426011, -28.56638892015329034 ) ) ;
#3609 = FACE_OUTER_BOUND ( 'NONE', #55261, .T. ) ;
#3610 = CARTESIAN_POINT ( 'NONE',  ( -71.62287095715005592, -24.64898659630528854, 1.056161002820824368 ) ) ;
#3611 = CARTESIAN_POINT ( 'NONE',  ( -12.65591448191638335, 15.52279176289047236, -1.500000000000002220 ) ) ;
#3612 = DIRECTION ( 'NONE',  ( 1.000000000000000000, 0.000000000000000000, 0.000000000000000000 ) ) ;
#3613 = ORIENTED_EDGE ( 'NONE', *, *, #72932, .F. ) ;
#3614 = EDGE_CURVE ( 'NONE', #63089, #50699, #90430, .T. ) ;
#3615 = CARTESIAN_POINT ( 'NONE',  ( -50.38822539166533687, -25.31297217564049973, 4.736250530714762874 ) ) ;
#3616 = B_SPLINE_CURVE_WITH_KNOTS ( 'NONE', 3,
 ( #40302, #72261, #64670, #17454 ),
 .UNSPECIFIED., .F., .F.,
 ( 4, 4 ),
 ( 0.000000000000000000, 9.999999999997510880E-05 ),
 .UNSPECIFIED. ) ;
#3617 = VECTOR ( 'NONE', #75065, 1000.000000000000114 ) ;
#3618 = CARTESIAN_POINT ( 'NONE',  ( -35.62660857665062508, -24.92564183028978775, 1.928384488918258199 ) ) ;
#3619 = LINE ( 'NONE', #34566, #98862 ) ;
#3620 = AXIS2_PLACEMENT_3D ( 'NONE', #14800, #74223, #20918 ) ;
#3621 = FACE_OUTER_BOUND ( 'NONE', #66225, .T. ) ;
#3622 = CARTESIAN_POINT ( 'NONE',  ( -73.60709162415560058, -23.48783264082477018, -1.443836473390094355 ) ) ;
#3623 = CARTESIAN_POINT ( 'NONE',  ( 15.76197349289695815, 3.603191427427850257, -28.09505689080078739 ) ) ;
#3624 = LINE ( 'NONE', #26948, #66388 ) ;
#3625 = ORIENTED_EDGE ( 'NONE', *, *, #37313, .T. ) ;
#3626 = CARTESIAN_POINT ( 'NONE',  ( -18.23349369547262810, -8.965252873808195133, 11.49999999999998934 ) ) ;
#3627 = ORIENTED_EDGE ( 'NONE', *, *, #47805, .T. ) ;
#3628 = EDGE_CURVE ( 'NONE', #14971, #11757, #58999, .T. ) ;
#3629 = CARTESIAN_POINT ( 'NONE',  ( -3.987988226355533072, 22.59150145119509290, -1.500000000000002220 ) ) ;
#3630 = CARTESIAN_POINT ( 'NONE',  ( 31.66639312903740944, 5.493490882720638346, 28.57493973316412905 ) ) ;
#3631 = VERTEX_POINT ( 'NONE', #72144 ) ;
#3632 = DIRECTION ( 'NONE',  ( 0.000000000000000000, -1.000000000000000000, 0.000000000000000000 ) ) ;
#3633 = CARTESIAN_POINT ( 'NONE',  ( -49.27841808360716414, -25.26263977505040970, 6.176812849117304438 ) ) ;
#3634 = AXIS2_PLACEMENT_3D ( 'NONE', #25393, #86788, #33015 ) ;
#3635 = DIRECTION ( 'NONE',  ( -3.773278334453080206E-23, 0.9999999999976377785, 2.173523156925979975E-06 ) ) ;
#3636 = CARTESIAN_POINT ( 'NONE',  ( 4.708956132399880978, 20.65895737721473679, 11.49999999999999645 ) ) ;
#3637 = ORGANIZATION ( 'NAUO-ORG1', 'UNSPECIFIED', 'UNSPECIFIED' ) ;
#3638 = CARTESIAN_POINT ( 'NONE',  ( -18.12599551585701008, -12.76988789260850332, 11.49999999999998934 ) ) ;
#3639 = ADVANCED_FACE ( 'NONE', ( #93797 ), #68419, .T. ) ;
#3640 = CARTESIAN_POINT ( 'NONE',  ( 9.149160795417088821, -18.46424698110740437, 11.49999999999998934 ) ) ;
#3641 = EDGE_LOOP ( 'NONE', ( #61447, #62910, #24123, #82420 ) ) ;
#3642 = DIRECTION ( 'NONE',  ( -1.000000000000000000, -3.773278334444167608E-23, -8.201307833595939069E-29 ) ) ;
#3643 = ORIENTED_EDGE ( 'NONE', *, *, #10243, .T. ) ;
#3644 = CARTESIAN_POINT ( 'NONE',  ( -54.49654312574512005, -24.34968618360932879, 0.1864209137778771175 ) ) ;
#3645 = CARTESIAN_POINT ( 'NONE',  ( 17.47419131657910540, -6.376774720514426953, 28.31804950686278843 ) ) ;
#3646 = EDGE_LOOP ( 'NONE', ( #82728, #89777, #82234, #88904 ) ) ;
#3647 = EDGE_LOOP ( 'NONE', ( #46761, #68544, #30198, #30 ) ) ;
#3648 = VERTEX_POINT ( 'NONE', #9064 ) ;
#3649 = VECTOR ( 'NONE', #24484, 1000.000000000000114 ) ;
#3650 = CARTESIAN_POINT ( 'NONE',  ( -70.62287095715005592, -25.00182538069145011, 7.747789668545097541 ) ) ;
#3651 = CARTESIAN_POINT ( 'NONE',  ( -108.5562042904833788, -24.65952944569304961, 1.056160979905704345 ) ) ;
#3652 = CARTESIAN_POINT ( 'NONE',  ( 5.963731207934512391, -5.876774720514413630, 19.80418863844947097 ) ) ;
#3653 = CARTESIAN_POINT ( 'NONE',  ( -16.26442346200556344, 12.93145763113255775, -1.500000000000002220 ) ) ;
#3654 = EDGE_CURVE ( 'NONE', #73030, #53704, #97055, .T. ) ;
#3655 = CARTESIAN_POINT ( 'NONE',  ( 10.00111611332133421, -19.26892646806700071, 11.49999999999999645 ) ) ;
#3656 = EDGE_LOOP ( 'NONE', ( #33104, #54476, #26850, #75271 ) ) ;
#3657 = DIRECTION ( 'NONE',  ( 0.000000000000000000, 0.000000000000000000, -1.000000000000000000 ) ) ;
#3658 = CARTESIAN_POINT ( 'NONE',  ( -115.5500786810796257, -25.00158670708910691, 2.256160236439219258 ) ) ;
#3659 = CARTESIAN_POINT ( 'NONE',  ( 17.95543856985664277, -13.40637504462900331, 11.49999999999998934 ) ) ;
#3660 = CARTESIAN_POINT ( 'NONE',  ( -59.62287095715004881, -24.64898659630367916, 1.056161002820822592 ) ) ;
#3661 = LINE ( 'NONE', #49342, #49740 ) ;
#3662 = ORIENTED_EDGE ( 'NONE', *, *, #25605, .F. ) ;
#3663 = DIRECTION ( 'NONE',  ( 0.000000000000000000, 0.000000000000000000, -1.000000000000000000 ) ) ;
#3664 = DIRECTION ( 'NONE',  ( -0.000000000000000000, -0.000000000000000000, -1.000000000000000000 ) ) ;
#3665 = B_SPLINE_SURFACE_WITH_KNOTS ( 'NONE', 3, 3, ( 
 ( #25315, #3493, #24316, #64914 ),
 ( #87214, #9093, #64413, #48679 ),
 ( #78584, #17203, #1993, #10093 ),
 ( #41052, #41556, #49671, #95331 ),
 ( #56791, #2997, #87725, #18207 ),
 ( #80104, #16701, #10589, #47669 ),
 ( #40046, #72504, #32433, #33935 ) ),
 .UNSPECIFIED., .F., .F., .F.,
 ( 4, 3, 4 ),
 ( 4, 4 ),
 ( 0.7945040050992244751, 0.8970133687736503436, 0.9995227324480763231 ),
 ( 0.6396565428357663396, 0.6409645752979864497 ),
 .UNSPECIFIED. ) ;
#3666 = ORIENTED_EDGE ( 'NONE', *, *, #10467, .F. ) ;
#3667 = ORIENTED_EDGE ( 'NONE', *, *, #37561, .F. ) ;
#3668 = CARTESIAN_POINT ( 'NONE',  ( -65.05438548721848235, -3.316774720514426456, 27.45402280011862572 ) ) ;
#3669 = VERTEX_POINT ( 'NONE', #39010 ) ;
#3670 = AXIS2_PLACEMENT_3D ( 'NONE', #39624, #8684, #72096 ) ;
#3671 = CARTESIAN_POINT ( 'NONE',  ( -16.84575021678815432, -12.90291372800108505, -1.500000000000002220 ) ) ;
#3672 = ORIENTED_EDGE ( 'NONE', *, *, #94562, .T. ) ;
#3673 = CARTESIAN_POINT ( 'NONE',  ( -88.58843689727572723, -24.34968618360934656, 0.1864209137778829184 ) ) ;
#3674 = CARTESIAN_POINT ( 'NONE',  ( 0.003323472525107682655, -21.86402403546210493, -1.500000000000002220 ) ) ;
#3675 = CARTESIAN_POINT ( 'NONE',  ( -52.63895323655680869, -24.15620529776627734, 10.23563542870661003 ) ) ;
#3676 = CARTESIAN_POINT ( 'NONE',  ( -22.58250372949163420, -2.080990182559540269, 11.49999999999998934 ) ) ;
#3677 = CARTESIAN_POINT ( 'NONE',  ( -40.49257998994310270, -25.18430871546432925, 3.294941901647467031 ) ) ;
#3678 = FACE_OUTER_BOUND ( 'NONE', #58984, .T. ) ;
#3679 = CARTESIAN_POINT ( 'NONE',  ( -13.92312151449838531, -16.86485062357919773, -1.500000000000002220 ) ) ;
#3680 = CARTESIAN_POINT ( 'NONE',  ( -109.5228709571500474, -24.51387760970725793, 9.387446482453411178 ) ) ;
#3681 = VERTEX_POINT ( 'NONE', #78056 ) ;
#3682 = DIRECTION ( 'NONE',  ( 0.000000000000000000, 2.173523156925979975E-06, -0.9999999999976378895 ) ) ;
#3683 = CARTESIAN_POINT ( 'NONE',  ( -49.21454750704995007, -25.12782705690641549, 7.069183625445169206 ) ) ;
#3684 = VERTEX_POINT ( 'NONE', #56264 ) ;
#3685 = CARTESIAN_POINT ( 'NONE',  ( -90.62287095715005592, -24.92579138211019796, 1.929029949965665125 ) ) ;
#3686 = B_SPLINE_CURVE_WITH_KNOTS ( 'NONE', 3,
 ( #8564, #100381, #54250, #39513, #70464, #53748 ),
 .UNSPECIFIED., .F., .F.,
 ( 4, 2, 4 ),
 ( 0.000000000000000000, 0.001380901958385392448, 0.002761803916770784895 ),
 .UNSPECIFIED. ) ;
#3687 = ORIENTED_EDGE ( 'NONE', *, *, #88725, .F. ) ;
#3688 = AXIS2_PLACEMENT_3D ( 'NONE', #5937, #61746, #54131 ) ;
#3689 = CARTESIAN_POINT ( 'NONE',  ( -89.62287095715004170, -23.48786465467241413, 11.44779295918254114 ) ) ;
#3690 = CARTESIAN_POINT ( 'NONE',  ( -30.60890090734109137, -24.57171501248768664, 0.8294870405985493855 ) ) ;
#3691 = CARTESIAN_POINT ( 'NONE',  ( 19.37530031839547107, -8.734557088507903799, 11.49999999999998934 ) ) ;
#3692 = CARTESIAN_POINT ( 'NONE',  ( -125.6228709571500843, -25.00182538069146432, 7.747789668545100206 ) ) ;
#3693 = CARTESIAN_POINT ( 'NONE',  ( -26.25750150876569933, -24.97064684238840115, 3.573366137800960907 ) ) ;
#3694 = CARTESIAN_POINT ( 'NONE',  ( -85.62495650507575817, -24.92564183028979130, 1.928384488918251982 ) ) ;
#3695 = CARTESIAN_POINT ( 'NONE',  ( -108.9228709571500389, -23.47596703998600631, 11.44779298504227860 ) ) ;
#3696 = CARTESIAN_POINT ( 'NONE',  ( 13.61561175257155298, 13.87280521877887018, 11.49999999999998934 ) ) ;
#3697 = EDGE_CURVE ( 'NONE', #1512, #71460, #46762, .T. ) ;
#3698 = CARTESIAN_POINT ( 'NONE',  ( 30.53060340732037048, -2.682774720514426559, -2.322449884495168870 ) ) ;
#3699 = ORIENTED_EDGE ( 'NONE', *, *, #63090, .T. ) ;
#3700 = CARTESIAN_POINT ( 'NONE',  ( 3.528372621398383924, 19.26332229581237598, 11.49999999999999645 ) ) ;
#3701 = CARTESIAN_POINT ( 'NONE',  ( -5.063563723219555612, -5.876774720514406525, 19.46509473978807847 ) ) ;
#3702 = CARTESIAN_POINT ( 'NONE',  ( -47.52287095715006160, -24.64965694238406613, 8.947790433994203596 ) ) ;
#3703 = ORIENTED_EDGE ( 'NONE', *, *, #4079, .T. ) ;
#3704 = CARTESIAN_POINT ( 'NONE',  ( 32.25249349869196891, 1.682774720514426114, -12.65342752644895441 ) ) ;
#3705 = LINE ( 'NONE', #48378, #38291 ) ;
#3706 = CARTESIAN_POINT ( 'NONE',  ( -106.5228709571500900, -23.47593901973090524, -1.443836447538996204 ) ) ;
#3707 = B_SPLINE_CURVE_WITH_KNOTS ( 'NONE', 3,
 ( #4821, #82925, #35774, #66744 ),
 .UNSPECIFIED., .F., .F.,
 ( 4, 4 ),
 ( 0.000000000000000000, 9.999999999997510880E-05 ),
 .UNSPECIFIED. ) ;
#3708 = VECTOR ( 'NONE', #35151, 1000.000000000000114 ) ;
#3709 = CARTESIAN_POINT ( 'NONE',  ( -60.52287095715008292, -23.48783264082477018, -1.443836473390092801 ) ) ;
#3710 = CARTESIAN_POINT ( 'NONE',  ( 19.18734209777730015, 4.435579877058994036, 11.49999999999998934 ) ) ;
#3712 = ORIENTED_EDGE ( 'NONE', *, *, #2318, .F. ) ;
#3711 = SECURITY_CLASSIFICATION ( '', '', #89083 ) ;
#3713 = CARTESIAN_POINT ( 'NONE',  ( -94.62287095715005592, -24.50216790748205753, 0.6166512839542525048 ) ) ;
#3714 = DIRECTION ( 'NONE',  ( -1.000000000000000000, -3.773278334444167608E-23, -8.201307833595939069E-29 ) ) ;
#3715 = EDGE_CURVE ( 'NONE', #76130, #19368, #3300, .T. ) ;
#3716 = AXIS2_PLACEMENT_3D ( 'NONE', #35908, #4961, #53146 ) ;
#3717 = DATE_AND_TIME ( #19917, #52239 ) ;
#3718 = B_SPLINE_CURVE_WITH_KNOTS ( 'NONE', 3,
 ( #93799, #38514, #40531, #62363 ),
 .UNSPECIFIED., .F., .F.,
 ( 4, 4 ),
 ( 1.387778780781445521E-17, 9.999999999997510880E-05 ),
 .UNSPECIFIED. ) ;
#3719 = ORIENTED_EDGE ( 'NONE', *, *, #96841, .T. ) ;
#3720 = DIRECTION ( 'NONE',  ( -1.000000000000000000, 0.000000000000000000, 0.000000000000000000 ) ) ;
#3721 = FACE_OUTER_BOUND ( 'NONE', #14689, .T. ) ;
#3722 = CARTESIAN_POINT ( 'NONE',  ( 18.72495633783376334, -0.5000000000000000000, -1.691563534834430227 ) ) ;
#3723 = CARTESIAN_POINT ( 'NONE',  ( -97.56098245220201193, -23.48786465467241413, 11.44779295918254469 ) ) ;
#3725 = EDGE_CURVE ( 'NONE', #40253, #23306, #8130, .T. ) ;
#3724 = DIRECTION ( 'NONE',  ( -2.000709955812756421E-15, 6.669033186042521139E-15, -1.000000000000000000 ) ) ;
#3726 = CARTESIAN_POINT ( 'NONE',  ( -73.52287095715007581, -24.66019654487199730, 8.947790411086121054 ) ) ;
#3727 = CARTESIAN_POINT ( 'NONE',  ( -79.52287095715007581, -24.51283580621364067, 0.6167428607019781461 ) ) ;
#3728 = CARTESIAN_POINT ( 'NONE',  ( 16.79105032741591330, -10.77411451815220822, 11.49999999999998934 ) ) ;
#3729 = CARTESIAN_POINT ( 'NONE',  ( -0.04038319741709193306, -22.52720777467708757, 8.529593833415562543 ) ) ;
#3730 = CARTESIAN_POINT ( 'NONE',  ( -17.31707178780640533, -9.736581320607820444, -1.500000000000002220 ) ) ;
#3731 = VERTEX_POINT ( 'NONE', #58249 ) ;
#3732 = EDGE_CURVE ( 'NONE', #34120, #55445, #26282, .T. ) ;
#3733 = DIRECTION ( 'NONE',  ( 0.000000000000000000, -1.000000000000000000, 0.000000000000000000 ) ) ;
#3734 = ADVANCED_FACE ( 'NONE', ( #34906 ), #42033, .F. ) ;
#3735 = ADVANCED_FACE ( 'NONE', ( #66372 ), #34406, .F. ) ;
#3736 = LINE ( 'NONE', #60406, #41410 ) ;
#3737 = CARTESIAN_POINT ( 'NONE',  ( 8.616046215355789073, -6.376774720514426065, -25.03514012577542758 ) ) ;
#3738 = CARTESIAN_POINT ( 'NONE',  ( 17.70469293622815243, 10.90570606759641592, 11.49999999999999645 ) ) ;
#3739 = CARTESIAN_POINT ( 'NONE',  ( 1.542438661763949392, 0.000000000000000000, 2.399999999999999911 ) ) ;
#3740 = DIRECTION ( 'NONE',  ( -0.000000000000000000, -1.000000000000000000, -0.000000000000000000 ) ) ;
#3741 = CARTESIAN_POINT ( 'NONE',  ( 12.51456667378993259, 19.11410217522374921, 11.49999999999999645 ) ) ;
#3742 = ORIENTED_EDGE ( 'NONE', *, *, #76201, .T. ) ;
#3743 = B_SPLINE_SURFACE_WITH_KNOTS ( 'NONE', 3, 3, ( 
 ( #22905, #15313, #77203, #103 ),
 ( #31041, #92937, #62008, #54397 ),
 ( #85839, #32050, #8219, #78212 ),
 ( #8722, #39658, #70616, #33061 ),
 ( #72133, #24933, #94953, #48798 ),
 ( #10724, #88347, #26943, #64038 ),
 ( #86833, #41686, #96452, #3124 ),
 ( #49299, #95952, #1615, #71123 ),
 ( #3618, #55911, #25941, #94451 ),
 ( #34062, #40170, #56913, #32551 ) ),
 .UNSPECIFIED., .F., .F., .F.,
 ( 4, 3, 3, 4 ),
 ( 4, 4 ),
 ( 0.0004766839783833132119, 0.1491231665100180015, 0.2234464077758353540, 0.2977696490416527064 ),
 ( 0.9496086901223659282, 0.9511872814519944930 ),
 .UNSPECIFIED. ) ;
#3744 = CARTESIAN_POINT ( 'NONE',  ( -55.52287095715008292, -23.47593901973090169, -1.443836447538997092 ) ) ;
#3745 = CARTESIAN_POINT ( 'NONE',  ( -91.22287095715005023, -23.47596703998600276, 11.44779298504227860 ) ) ;
#3746 = ORIENTED_EDGE ( 'NONE', *, *, #8761, .T. ) ;
#3747 = CARTESIAN_POINT ( 'NONE',  ( 20.24638344296597836, 0.1212440198127159030, -1.500000000000002220 ) ) ;
#3748 = EDGE_CURVE ( 'NONE', #35109, #12184, #72979, .T. ) ;
#3749 = CARTESIAN_POINT ( 'NONE',  ( 7.475222833218381879, -6.376774720514418959, 20.91460388675487891 ) ) ;
#3750 = CARTESIAN_POINT ( 'NONE',  ( -39.62287095715005592, -29.50250243563736774, 8.947779886222148704 ) ) ;
#3751 = VECTOR ( 'NONE', #47453, 1000.000000000000114 ) ;
#3752 = CARTESIAN_POINT ( 'NONE',  ( -82.55620429048340725, -24.66019654487199730, 8.947790411086128159 ) ) ;
#3753 = EDGE_LOOP ( 'NONE', ( #47082, #50777, #71707, #72182 ) ) ;
#3754 = DIRECTION ( 'NONE',  ( -3.773278334453080206E-23, 0.9999999999976377785, 2.173523156925979975E-06 ) ) ;
#3755 = DIRECTION ( 'NONE',  ( 1.000000000000000000, 0.000000000000000000, 0.000000000000000000 ) ) ;
#3756 = CARTESIAN_POINT ( 'NONE',  ( -1.415466703587968667, 19.98303252902060834, -1.500000000000002220 ) ) ;
#3757 = AXIS2_PLACEMENT_3D ( 'NONE', #83958, #76823, #30670 ) ;
#3758 = CARTESIAN_POINT ( 'NONE',  ( 12.99892964944760543, 16.54660993828877125, 11.49999999999999645 ) ) ;
#3759 = CARTESIAN_POINT ( 'NONE',  ( -29.76904096422576274, -25.22379592436849194, 5.866293395515224773 ) ) ;
#3760 = CARTESIAN_POINT ( 'NONE',  ( -5.891025641025637860, -6.376774720514427841, 21.75000000000000711 ) ) ;
#3761 = CARTESIAN_POINT ( 'NONE',  ( 3.837975233861466329, 21.70421690940786874, -1.500000000000002220 ) ) ;
#3762 = EDGE_CURVE ( 'NONE', #55465, #25617, #25003, .T. ) ;
#3763 = CARTESIAN_POINT ( 'NONE',  ( -53.52287095715006870, -24.64965694238574656, 8.947790433994203596 ) ) ;
#3764 = DIRECTION ( 'NONE',  ( -3.773278334453079030E-23, 0.9999999999976377785, 2.173523156925979128E-06 ) ) ;
#3765 = CARTESIAN_POINT ( 'NONE',  ( -127.5228709571500616, -24.64965694238408034, 8.947790433994189385 ) ) ;
#3766 = EDGE_CURVE ( 'NONE', #6469, #98127, #9798, .T. ) ;
#3767 = CARTESIAN_POINT ( 'NONE',  ( -91.15361000704896810, -25.27880950044357178, 5.947789066507965572 ) ) ;
#3768 = CARTESIAN_POINT ( 'NONE',  ( -31.47684055086448396, -24.65952944569304250, 1.056160979905695463 ) ) ;
#3769 = ORIENTED_EDGE ( 'NONE', *, *, #31497, .F. ) ;
#3770 = ORIENTED_EDGE ( 'NONE', *, *, #26761, .F. ) ;
#3771 = CARTESIAN_POINT ( 'NONE',  ( -80.52287095715007581, -23.48783264082477018, -1.443836473390091246 ) ) ;
#3772 = CARTESIAN_POINT ( 'NONE',  ( -61.35927149850876816, -25.04662945190125001, 7.499198004902734915 ) ) ;
#3773 = CARTESIAN_POINT ( 'NONE',  ( -90.25931482958500851, -25.31788868711539209, 4.644810524077565006 ) ) ;
#3774 = CARTESIAN_POINT ( 'NONE',  ( 12.93548710985481698, 15.95582723538240266, -1.500000000000002220 ) ) ;
#3775 = EDGE_CURVE ( 'NONE', #99074, #82884, #43181, .T. ) ;
#3776 = ORIENTED_EDGE ( 'NONE', *, *, #16769, .T. ) ;
#3777 = CARTESIAN_POINT ( 'NONE',  ( 27.53860345374808105, -1.477225279485574028, 19.84760796525321780 ) ) ;
#3778 = CARTESIAN_POINT ( 'NONE',  ( 0.000000000000000000, -0.3850000000000046163, 1.529999999999998916 ) ) ;
#3779 = CARTESIAN_POINT ( 'NONE',  ( -83.52287095715007581, -23.48783264082477018, -1.443836473390090802 ) ) ;
#3780 = CARTESIAN_POINT ( 'NONE',  ( 21.63714550250683644, -5.416328558471028565, 11.49999999999998934 ) ) ;
#3781 = EDGE_CURVE ( 'NONE', #97633, #29959, #97302, .T. ) ;
#3783 = CARTESIAN_POINT ( 'NONE',  ( 29.70566059910618861, -3.975162330554212531, 28.10075438475601928 ) ) ;
#3782 = VECTOR ( 'NONE', #25291, 1000.000000000000000 ) ;
#3784 = PLANE ( 'NONE',  #10824 ) ;
#3785 = ORIENTED_EDGE ( 'NONE', *, *, #67950, .F. ) ;
#3786 = ADVANCED_FACE ( 'NONE', ( #35897 ), #51362, .T. ) ;
#3787 = CARTESIAN_POINT ( 'NONE',  ( -32.62287095715006302, -23.47596703998600276, 11.44779298504227505 ) ) ;
#3788 = DIRECTION ( 'NONE',  ( -3.773278334453080206E-23, 0.9999999999976377785, 2.173523156925979975E-06 ) ) ;
#3789 = CARTESIAN_POINT ( 'NONE',  ( -20.80165436122882383, -1.723964017131293103, 11.49999999999998934 ) ) ;
#3790 = ORIENTED_EDGE ( 'NONE', *, *, #66935, .F. ) ;
#3792 = ORIENTED_EDGE ( 'NONE', *, *, #28294, .F. ) ;
#3791 = CARTESIAN_POINT ( 'NONE',  ( -92.58953762381672448, -24.65952944569304606, 1.056160979905705455 ) ) ;
#3793 = ORIENTED_EDGE ( 'NONE', *, *, #8987, .F. ) ;
#3794 = VECTOR ( 'NONE', #30757, 1000.000000000000114 ) ;
#3795 = CARTESIAN_POINT ( 'NONE',  ( -70.34543693012690824, -25.25935350734801332, 7.563173724185935143 ) ) ;
#3796 = CARTESIAN_POINT ( 'NONE',  ( -10.38599875782317206, -18.32754119035049101, -1.500000000000002220 ) ) ;
#3797 = VERTEX_POINT ( 'NONE', #22689 ) ;
#3798 = CARTESIAN_POINT ( 'NONE',  ( 5.326923076923078426, -6.376774720514420736, 20.76772836538461320 ) ) ;
#3799 = CARTESIAN_POINT ( 'NONE',  ( 6.546094359317672584, -5.876774720514411854, 19.73546617144828375 ) ) ;
#3800 = CARTESIAN_POINT ( 'NONE',  ( -79.52287095715006160, -29.50247984919015209, -1.443849546365053582 ) ) ;
#3801 = CIRCLE ( 'NONE', #76690, 18.35000000000000142 ) ;
#3802 = CARTESIAN_POINT ( 'NONE',  ( -76.63010253711489383, -24.35071581493543036, 9.817618358456028815 ) ) ;
#3803 = CARTESIAN_POINT ( 'NONE',  ( 7.311104923646705167, -5.876774720514415407, 20.13320233724603980 ) ) ;
#3804 = CARTESIAN_POINT ( 'NONE',  ( 21.38347125639554136, -3.707035686939989638, -1.500000000000002220 ) ) ;
#3805 = CARTESIAN_POINT ( 'NONE',  ( 5.271800844963591359, -3.316774720514426456, -28.56638892015329745 ) ) ;
#3807 = ORIENTED_EDGE ( 'NONE', *, *, #171, .T. ) ;
#3806 = CARTESIAN_POINT ( 'NONE',  ( -19.83904684311861644, 10.14288308415042827, 11.49999999999999645 ) ) ;
#3808 = B_SPLINE_CURVE_WITH_KNOTS ( 'NONE', 3,
 ( #24763, #99876, #69947, #55747, #48127, #79055, #80062, #88183, #57742, #96291, #64370, #41010, #3456, #2447, #79562, #32895 ),
 .UNSPECIFIED., .F., .F.,
 ( 4, 2, 2, 2, 2, 2, 2, 4 ),
 ( 8.673617379884035472E-19, 0.0002758817178494569707, 0.0005517634356989130741, 0.0008276451535483693401, 0.001103526871397825281, 0.001655290307096738463, 0.001931172024946204921, 0.002207053742795670945 ),
 .UNSPECIFIED. ) ;
#3809 = CARTESIAN_POINT ( 'NONE',  ( -50.92793838057655620, -25.24728748494000286, 5.312585385865816079 ) ) ;
#3810 = CARTESIAN_POINT ( 'NONE',  ( 7.155337544004596317, -6.376774720514417183, 20.64714842558261765 ) ) ;
#3811 = PLANE ( 'NONE',  #39139 ) ;
#3812 = ORIENTED_EDGE ( 'NONE', *, *, #79298, .F. ) ;
#3813 = B_SPLINE_CURVE_WITH_KNOTS ( 'NONE', 3,
 ( #22038, #99167, #22531, #29666 ),
 .UNSPECIFIED., .F., .F.,
 ( 4, 4 ),
 ( 0.000000000000000000, 9.999999999998897304E-05 ),
 .UNSPECIFIED. ) ;
#3815 = ORIENTED_EDGE ( 'NONE', *, *, #88286, .T. ) ;
#3814 = CARTESIAN_POINT ( 'NONE',  ( -105.2228709571500787, -23.47596703998600631, 11.44779298504227860 ) ) ;
#3816 = VERTEX_POINT ( 'NONE', #13085 ) ;
#3817 = LINE ( 'NONE', #58591, #43251 ) ;
#3818 = CARTESIAN_POINT ( 'NONE',  ( -49.87852880094167318, -25.29918105047413945, 4.602234888658000678 ) ) ;
#3819 = CARTESIAN_POINT ( 'NONE',  ( 31.37501302269236092, 4.132774720514428068, -3.717120176012355781 ) ) ;
#3820 = CARTESIAN_POINT ( 'NONE',  ( -105.5228709571500616, -23.85196035786900026, -0.8779234886475166810 ) ) ;
#3821 = ORIENTED_EDGE ( 'NONE', *, *, #53001, .T. ) ;
#3822 = CARTESIAN_POINT ( 'NONE',  ( -130.5728709571500303, -24.93503760150525395, 8.366236236982352636 ) ) ;
#3823 = CARTESIAN_POINT ( 'NONE',  ( -19.78178409256797465, 10.57734301857266246, -1.500000000000002220 ) ) ;
#3824 = EDGE_LOOP ( 'NONE', ( #19718, #49691, #50337, #64827, #54737, #69528, #42189, #8083, #70023, #34708, #66887, #32644 ) ) ;
#3825 = CARTESIAN_POINT ( 'NONE',  ( -72.55620429048340725, -23.48783264082478794, -1.443836473390067487 ) ) ;
#3827 = LINE ( 'NONE', #34273, #88023 ) ;
#3826 = VECTOR ( 'NONE', #84899, 1000.000000000000114 ) ;
#3828 = CARTESIAN_POINT ( 'NONE',  ( 8.583179188118256420, 5.356774720514425603, -25.03641645905366886 ) ) ;
#3829 = CARTESIAN_POINT ( 'NONE',  ( -34.52287095715006160, -29.50247984919015209, -1.443849546365062242 ) ) ;
#3830 = CARTESIAN_POINT ( 'NONE',  ( -130.5728709571501156, -24.82935162629097547, 1.633150109380539172 ) ) ;
#3831 = CARTESIAN_POINT ( 'NONE',  ( 18.24213732562919787, -7.162457363581539838, -1.500000000000002220 ) ) ;
#3832 = CIRCLE ( 'NONE', #47655, 2.349999999999999645 ) ;
#3833 = DIRECTION ( 'NONE',  ( 0.000000000000000000, -0.9999999999976377785, -2.173523156925979128E-06 ) ) ;
#3834 = VERTEX_POINT ( 'NONE', #98825 ) ;
#3835 = CARTESIAN_POINT ( 'NONE',  ( 13.04721882220160012, 17.14300067834640373, -1.500000000000002220 ) ) ;
#3836 = CARTESIAN_POINT ( 'NONE',  ( -129.6228709571500417, -24.64965695001463430, 8.947790411086117501 ) ) ;
#3837 = CARTESIAN_POINT ( 'NONE',  ( -70.86754458488196917, -25.25639569759052705, 6.955654243306450546 ) ) ;
#3838 = CARTESIAN_POINT ( 'NONE',  ( -95.62287095715002749, -25.00182538069145721, 7.747789668545097541 ) ) ;
#3839 = DIRECTION ( 'NONE',  ( 0.000000000000000000, -1.000000000000000000, 0.000000000000000000 ) ) ;
#3840 = CARTESIAN_POINT ( 'NONE',  ( -16.88208375265294237, -15.58181570610299715, -1.500000000000002220 ) ) ;
#3841 = B_SPLINE_CURVE_WITH_KNOTS ( 'NONE', 3,
 ( #47342, #37722, #53466, #22972 ),
 .UNSPECIFIED., .F., .F.,
 ( 4, 4 ),
 ( 0.9211577762202510788, 0.9301642074923666126 ),
 .UNSPECIFIED. ) ;
#3842 = EDGE_CURVE ( 'NONE', #61654, #14296, #84305, .T. ) ;
#3843 = APPROVAL_DATE_TIME ( #87566, #47005 ) ;
#3844 = CARTESIAN_POINT ( 'NONE',  ( -84.62287095715008434, -23.47596703998600631, 11.44779298504227860 ) ) ;
#3845 = CARTESIAN_POINT ( 'NONE',  ( -49.56822730090311779, -23.48783264082477018, -1.443836473390094133 ) ) ;
#3846 = CARTESIAN_POINT ( 'NONE',  ( 15.80722972286721983, -12.41807379269815215, 11.49999999999999645 ) ) ;
#3847 = CARTESIAN_POINT ( 'NONE',  ( -77.52287095715006160, -29.50248528299804818, 1.056150453629038477 ) ) ;
#3848 = DIRECTION ( 'NONE',  ( 1.232047923278981953E-16, 1.000000000000000000, 0.000000000000000000 ) ) ;
#3849 = EDGE_CURVE ( 'NONE', #83993, #17395, #14085, .T. ) ;
#3850 = CARTESIAN_POINT ( 'NONE',  ( -69.62287095715005592, -29.50247984919015209, -1.443849546365055359 ) ) ;
#3851 = CARTESIAN_POINT ( 'NONE',  ( -79.62287095715005592, -24.64965695001468404, 8.947790433994182280 ) ) ;
#3852 = DIRECTION ( 'NONE',  ( -3.773278334453079030E-23, 0.9999999999976377785, 2.173523156925979128E-06 ) ) ;
#3853 = CARTESIAN_POINT ( 'NONE',  ( -19.77004505525285083, 2.005399880840008642, -1.500000000000002220 ) ) ;
#3854 = ADVANCED_FACE ( 'NONE', ( #100305 ), #84105, .F. ) ;
#3855 = DIRECTION ( 'NONE',  ( 3.773278334444166432E-23, -1.000000000000000000, 0.000000000000000000 ) ) ;
#3856 = CARTESIAN_POINT ( 'NONE',  ( -0.6023826358649750912, 19.72334862104828090, -1.500000000000002220 ) ) ;
#3857 = EDGE_CURVE ( 'NONE', #25844, #67625, #75864, .T. ) ;
#3858 = CARTESIAN_POINT ( 'NONE',  ( -42.55306471323350337, -23.96119346886880663, -0.6495511937831992544 ) ) ;
#3859 = EDGE_CURVE ( 'NONE', #15452, #38350, #34725, .T. ) ;
#3860 = APPROVAL_ROLE ( '' ) ;
#3861 = EDGE_CURVE ( 'NONE', #41110, #8126, #89185, .T. ) ;
#3862 = CARTESIAN_POINT ( 'NONE',  ( 14.44544951633968566, 3.759487683616679288, -28.33948095063585271 ) ) ;
#3863 = CARTESIAN_POINT ( 'NONE',  ( 2.932009311892267434, -6.376774720514410077, 19.53174284846577891 ) ) ;
#3864 = CARTESIAN_POINT ( 'NONE',  ( -20.24099117049231467, 3.958469829285517161, 11.49999999999999645 ) ) ;
#3865 = B_SPLINE_CURVE_WITH_KNOTS ( 'NONE', 3,
 ( #78902, #41362, #18018, #32235 ),
 .UNSPECIFIED., .F., .F.,
 ( 4, 4 ),
 ( 0.000000000000000000, 9.999999999999592548E-05 ),
 .UNSPECIFIED. ) ;
#3866 = LINE ( 'NONE', #10966, #23793 ) ;
#3867 = CIRCLE ( 'NONE', #7102, 10.11363636363636331 ) ;
#3868 = CARTESIAN_POINT ( 'NONE',  ( 21.71957326813621592, -6.446789169762093152, 11.49999999999999645 ) ) ;
#3869 = ORIENTED_EDGE ( 'NONE', *, *, #20780, .T. ) ;
#3870 = CARTESIAN_POINT ( 'NONE',  ( -102.6228709571500559, -24.65952944569304606, 1.056160979905702124 ) ) ;
#3871 = CARTESIAN_POINT ( 'NONE',  ( -50.65411740745392422, -25.31193108374115752, 4.703768078485199844 ) ) ;
#3872 = VECTOR ( 'NONE', #51009, 1000.000000000000114 ) ;
#3873 = EDGE_CURVE ( 'NONE', #68993, #94137, #53675, .T. ) ;
#3874 = CARTESIAN_POINT ( 'NONE',  ( -27.65532027823855543, -24.93063634776342141, 8.251096489757108188 ) ) ;
#3875 = LINE ( 'NONE', #5355, #49611 ) ;
#3876 = ORIENTED_EDGE ( 'NONE', *, *, #37712, .F. ) ;
#3877 = ORIENTED_EDGE ( 'NONE', *, *, #20018, .F. ) ;
#3878 = EDGE_CURVE ( 'NONE', #94577, #33073, #10455, .T. ) ;
#3879 = CARTESIAN_POINT ( 'NONE',  ( 0.3908843598833069422, -6.376774720514420736, 20.63520656483649773 ) ) ;
#3880 = CARTESIAN_POINT ( 'NONE',  ( 21.14566350062385780, -8.679158401671109857, 11.49999999999998934 ) ) ;
#3881 = PLANE ( 'NONE',  #61665 ) ;
#3882 = CARTESIAN_POINT ( 'NONE',  ( -113.5222245837002646, -23.48786465467241058, 11.44779295918254292 ) ) ;
#3883 = PLANE ( 'NONE',  #72805 ) ;
#3884 = CARTESIAN_POINT ( 'NONE',  ( -22.50818191331092777, 0.9639279967183422837, 11.49999999999999645 ) ) ;
#3885 = ORIENTED_EDGE ( 'NONE', *, *, #56485, .F. ) ;
#3886 = B_SPLINE_CURVE_WITH_KNOTS ( 'NONE', 3,
 ( #2980, #50145, #49650, #33913, #95312, #3476, #34414, #65395, #71991, #64896, #72486, #80583, #96809, #63893, #42541, #73476, #56274, #3973 ),
 .UNSPECIFIED., .F., .F.,
 ( 4, 2, 2, 2, 2, 2, 2, 2, 4 ),
 ( 0.000000000000000000, 0.0001439754707682965951, 0.0002879509415365931902, 0.0005759018830731794415, 0.0008638528246097658013, 0.001151803766146352161, 0.001727705649219524664, 0.002015656590756111349, 0.002303607532292697817 ),
 .UNSPECIFIED. ) ;
#3887 = CARTESIAN_POINT ( 'NONE',  ( -33.58953762381672448, -23.48786465467240347, 11.44779295918255535 ) ) ;
#3888 = CARTESIAN_POINT ( 'NONE',  ( -19.44315311050126382, -10.23602577120861667, 11.49999999999998934 ) ) ;
#3889 = ADVANCED_FACE ( 'NONE', ( #52166 ), #5485, .T. ) ;
#3890 = PLANE ( 'NONE',  #91641 ) ;
#3891 = CARTESIAN_POINT ( 'NONE',  ( -29.14051086615235420, -24.79700015330595164, 6.215525944783297341 ) ) ;
#3892 = ORIENTED_EDGE ( 'NONE', *, *, #95387, .T. ) ;
#3893 = CARTESIAN_POINT ( 'NONE',  ( -63.62287095715004881, -23.95044443724992789, 10.65354141964649948 ) ) ;
#3894 = CARTESIAN_POINT ( 'NONE',  ( -111.6228709571500559, -24.64898659630368627, 1.056161002820831474 ) ) ;
#3895 = ORIENTED_EDGE ( 'NONE', *, *, #1374, .F. ) ;
#3896 = PLANE ( 'NONE',  #24194 ) ;
#3897 = CARTESIAN_POINT ( 'NONE',  ( -10.27258457790969892, -17.75692283049141196, -1.500000000000002220 ) ) ;
#3898 = ORIENTED_EDGE ( 'NONE', *, *, #44188, .F. ) ;
#3899 = VERTEX_POINT ( 'NONE', #69386 ) ;
#3900 = ORIENTED_EDGE ( 'NONE', *, *, #47879, .T. ) ;
#3901 = LINE ( 'NONE', #82989, #19405 ) ;
#3902 = CARTESIAN_POINT ( 'NONE',  ( -8.701767255460435280, 21.38705905713849020, -1.500000000000002220 ) ) ;
#3903 = CARTESIAN_POINT ( 'NONE',  ( -104.5951208871063471, -23.73791477778912196, 11.05961554403170410 ) ) ;
#3904 = CARTESIAN_POINT ( 'NONE',  ( -20.29798418530817017, 1.744846428065259136, -1.500000000000002220 ) ) ;
#3905 = CIRCLE ( 'NONE', #62208, 91.74549126261076992 ) ;
#3906 = ORIENTED_EDGE ( 'NONE', *, *, #24513, .F. ) ;
#3907 = CARTESIAN_POINT ( 'NONE',  ( -24.90875734969025501, -3.316774720514426456, 26.43402280011862615 ) ) ;
#3908 = CARTESIAN_POINT ( 'NONE',  ( -10.16634758543296613, 5.965225279485572685, 30.00402280011862288 ) ) ;
#3909 = ADVANCED_FACE ( 'NONE', ( #36434 ), #60790, .T. ) ;
#3910 = CARTESIAN_POINT ( 'NONE',  ( -89.49044893904931541, -25.11033443465437287, 2.832404802291436319 ) ) ;
#3911 = CARTESIAN_POINT ( 'NONE',  ( -35.52287095715006870, -23.47593901973090169, -1.443836447538997092 ) ) ;
#3912 = ORIENTED_EDGE ( 'NONE', *, *, #89824, .F. ) ;
#3913 = CARTESIAN_POINT ( 'NONE',  ( -28.94548163072471425, -25.21531839410873843, 3.108273061491439559 ) ) ;
#3915 = AXIS2_PLACEMENT_3D ( 'NONE', #55552, #32192, #71772 ) ;
#3914 = CARTESIAN_POINT ( 'NONE',  ( -89.62287095715004170, -23.47593901973091235, -1.443836447539002865 ) ) ;
#3916 = EDGE_LOOP ( 'NONE', ( #90847, #75029, #61708, #43069 ) ) ;
#3917 = CARTESIAN_POINT ( 'NONE',  ( -8.119355292522030254, -19.11072509857415369, 11.49999999999998934 ) ) ;
#3918 = EDGE_CURVE ( 'NONE', #86903, #13321, #53175, .T. ) ;
#3919 = ORIENTED_EDGE ( 'NONE', *, *, #47278, .T. ) ;
#3921 = ORIENTED_EDGE ( 'NONE', *, *, #52793, .T. ) ;
#3920 = CARTESIAN_POINT ( 'NONE',  ( -101.6339284197689210, -23.73766607897670511, -1.055555164236452237 ) ) ;
#3922 = CARTESIAN_POINT ( 'NONE',  ( -86.62287095715008434, -24.34917612406837861, 0.1852690917426653427 ) ) ;
#3923 = DIRECTION ( 'NONE',  ( 0.000000000000000000, -1.000000000000000000, 0.000000000000000000 ) ) ;
#3924 = ORIENTED_EDGE ( 'NONE', *, *, #71796, .T. ) ;
#3925 = VERTEX_POINT ( 'NONE', #69887 ) ;
#3926 = FACE_OUTER_BOUND ( 'NONE', #99232, .T. ) ;
#3927 = DIRECTION ( 'NONE',  ( 1.000000000000000000, 0.000000000000000000, 0.000000000000000000 ) ) ;
#3928 = CARTESIAN_POINT ( 'NONE',  ( 11.16000000000000014, -10.65233964170348635, -1.621096496867198589 ) ) ;
#3929 = CARTESIAN_POINT ( 'NONE',  ( -70.39323859381175907, -25.31201590701856574, 5.314173951595296153 ) ) ;
#3931 = ORIENTED_EDGE ( 'NONE', *, *, #88286, .F. ) ;
#3930 = CARTESIAN_POINT ( 'NONE',  ( -7.692412698405892257, 20.70400481474656118, 11.49999999999999645 ) ) ;
#3932 = CARTESIAN_POINT ( 'NONE',  ( -103.5909381567761898, -24.15543982623907482, -0.2315651400026619011 ) ) ;
#3933 = CARTESIAN_POINT ( 'NONE',  ( 1.383477600506065164, -22.57338898373578218, -1.500000000000002220 ) ) ;
#3935 = VERTEX_POINT ( 'NONE', #8489 ) ;
#3934 = CARTESIAN_POINT ( 'NONE',  ( -115.5137987077945070, -24.92592662359561473, 8.075495903017996469 ) ) ;
#3936 = ORIENTED_EDGE ( 'NONE', *, *, #37973, .F. ) ;
#3937 = CARTESIAN_POINT ( 'NONE',  ( -88.52287095715009002, -24.66019654487200441, 8.947790411086119278 ) ) ;
#3938 = DIRECTION ( 'NONE',  ( 0.000000000000000000, -1.000000000000000000, 0.000000000000000000 ) ) ;
#3939 = ORIENTED_EDGE ( 'NONE', *, *, #40369, .F. ) ;
#3940 = CARTESIAN_POINT ( 'NONE',  ( -14.79452276021403634, 15.15755283273500531, -1.500000000000002220 ) ) ;
#3941 = CARTESIAN_POINT ( 'NONE',  ( -7.318926569091948942, -6.376774720514417183, 20.09505574050193033 ) ) ;
#3942 = CARTESIAN_POINT ( 'NONE',  ( -41.82823102631974876, -25.29805763927562268, 4.565812412427879607 ) ) ;
#3943 = CARTESIAN_POINT ( 'NONE',  ( 22.20884612314100792, -2.053178116692622623, -1.500000000000002220 ) ) ;
#3944 = B_SPLINE_CURVE_WITH_KNOTS ( 'NONE', 3,
 ( #32438, #1501, #63412, #17715, #56299, #11097, #10595, #94330 ),
 .UNSPECIFIED., .F., .F.,
 ( 4, 2, 2, 4 ),
 ( -0.001224554619866345413, -0.0002241820295893642324, 0.0007761905606876169476, 0.002776935741241582777 ),
 .UNSPECIFIED. ) ;
#3945 = LINE ( 'NONE', #50609, #75965 ) ;
#3946 = ORIENTED_EDGE ( 'NONE', *, *, #10129, .F. ) ;
#3947 = CARTESIAN_POINT ( 'NONE',  ( -80.22287095715007865, -23.47596703998600631, 11.44779298504227860 ) ) ;
#3948 = CYLINDRICAL_SURFACE ( 'NONE', #76717, 2.249999999999998668 ) ;
#3949 = CARTESIAN_POINT ( 'NONE',  ( -36.61838302510732035, -23.48786465467240347, 11.44779295918255180 ) ) ;
#3950 = DIRECTION ( 'NONE',  ( -0.000000000000000000, -1.000000000000000000, -0.000000000000000000 ) ) ;
#3951 = CARTESIAN_POINT ( 'NONE',  ( -18.91883139384513157, -4.797682538509264738, 11.49999999999998934 ) ) ;
#3952 = CARTESIAN_POINT ( 'NONE',  ( 15.63241172484657682, -14.69700884395465934, -1.500000000000002220 ) ) ;
#3953 = CARTESIAN_POINT ( 'NONE',  ( -1.267404104715736279, -5.876774720514411854, 19.66076420632889921 ) ) ;
#3954 = CARTESIAN_POINT ( 'NONE',  ( 29.73828978136054602, 4.772774720514425972, -4.021765098496561386 ) ) ;
#3955 = CARTESIAN_POINT ( 'NONE',  ( -12.84880425037202656, 0.3587747205143964613, -26.59900746623529244 ) ) ;
#3957 = CIRCLE ( 'NONE', #70362, 10.20000000000000107 ) ;
#3956 = CARTESIAN_POINT ( 'NONE',  ( 2.581029390964978187, -22.66945732913600509, -1.500000000000002220 ) ) ;
#3958 = DIRECTION ( 'NONE',  ( -0.3563318776612551808, 1.473222943873815447E-23, -0.9343594559709900160 ) ) ;
#3959 = CARTESIAN_POINT ( 'NONE',  ( -102.6290229638939024, -24.15543982623908192, -0.2315651400026459694 ) ) ;
#3960 = DIRECTION ( 'NONE',  ( 0.000000000000000000, 1.000000000000000000, -0.000000000000000000 ) ) ;
#3961 = CARTESIAN_POINT ( 'NONE',  ( 16.68016870136555596, 10.92824754362290385, 11.49999999999999645 ) ) ;
#3962 = CARTESIAN_POINT ( 'NONE',  ( -31.52287095715006160, -24.50216790748204332, 0.6166512839542445112 ) ) ;
#3963 = ADVANCED_FACE ( 'NONE', ( #39439 ), #71396, .T. ) ;
#3964 = EDGE_CURVE ( 'NONE', #45335, #94542, #23699, .T. ) ;
#3965 = FACE_OUTER_BOUND ( 'NONE', #97634, .T. ) ;
#3966 = CARTESIAN_POINT ( 'NONE',  ( -48.63974925878575561, -24.15543982623907127, -0.2315651400026527418 ) ) ;
#3967 = EDGE_LOOP ( 'NONE', ( #13290, #53434, #130, #76891 ) ) ;
#3968 = CARTESIAN_POINT ( 'NONE',  ( -5.366453405989235925, -2.000000000000005329, 18.24068255301867936 ) ) ;
#3969 = CARTESIAN_POINT ( 'NONE',  ( -77.52287095715007581, -23.48783264082476308, -1.443836473390091912 ) ) ;
#3970 = AXIS2_PLACEMENT_3D ( 'NONE', #99449, #77610, #29442 ) ;
#3971 = EDGE_CURVE ( 'NONE', #69379, #76864, #66545, .T. ) ;
#3972 = CARTESIAN_POINT ( 'NONE',  ( 18.84366469573077296, 10.75509914293975555, -1.500000000000002220 ) ) ;
#3973 = CARTESIAN_POINT ( 'NONE',  ( -50.40895856474225667, -25.04307398257883577, 7.563174194274489892 ) ) ;
#3974 = CARTESIAN_POINT ( 'NONE',  ( -16.69004703121433408, -10.21020960635683394, -1.500000000000002220 ) ) ;
#3975 = EDGE_CURVE ( 'NONE', #5790, #43961, #92756, .T. ) ;
#3976 = CARTESIAN_POINT ( 'NONE',  ( 27.53860345374808105, 1.477225279485574028, -6.982392034746241372 ) ) ;
#3977 = APPROVAL_STATUS ( 'not_yet_approved' ) ;
#3978 = CARTESIAN_POINT ( 'NONE',  ( -60.62287095715003460, -24.63345952396255001, 9.038047939301510070 ) ) ;
#3979 = CARTESIAN_POINT ( 'NONE',  ( -20.02755620033356010, -4.236777897013602079, 11.49999999999999645 ) ) ;
#3980 = CARTESIAN_POINT ( 'NONE',  ( -27.25988310792305214, -0.3587747205144265483, 30.32664379231667695 ) ) ;
#3981 = CARTESIAN_POINT ( 'NONE',  ( -59.56094173781918499, -25.20074414198133539, 3.409327697718782080 ) ) ;
#3982 = ORIENTED_EDGE ( 'NONE', *, *, #98674, .T. ) ;
#3983 = DIRECTION ( 'NONE',  ( 0.000000000000000000, -2.173523156925979552E-06, 0.9999999999976378895 ) ) ;
#3984 = PLANE ( 'NONE',  #8795 ) ;
#3985 = DIRECTION ( 'NONE',  ( 1.000000000000000000, -4.218136541796977197E-15, 0.000000000000000000 ) ) ;
#3986 = CARTESIAN_POINT ( 'NONE',  ( -109.5126161358243309, -24.65952944569305316, 1.056160979905708786 ) ) ;
#3987 = ORIENTED_EDGE ( 'NONE', *, *, #45923, .F. ) ;
#3988 = B_SPLINE_CURVE_WITH_KNOTS ( 'NONE', 3,
 ( #2416, #41472, #18620, #32861 ),
 .UNSPECIFIED., .F., .F.,
 ( 4, 4 ),
 ( 0.000000000000000000, 9.999999999998897304E-05 ),
 .UNSPECIFIED. ) ;
#3989 = CARTESIAN_POINT ( 'NONE',  ( 14.87233727408824713, -17.56007624320114857, 11.49999999999999645 ) ) ;
#3990 = CARTESIAN_POINT ( 'NONE',  ( -22.19569011343799048, 5.130922947863589378, -1.500000000000002220 ) ) ;
#3991 = CARTESIAN_POINT ( 'NONE',  ( -110.6235418037408920, -25.00182538069147498, 7.747789668545046027 ) ) ;
#3992 = CARTESIAN_POINT ( 'NONE',  ( -4.700032041049139409, -6.144890974841530351, -9.000000000000000000 ) ) ;
#3993 = CARTESIAN_POINT ( 'NONE',  ( -98.22287095715007865, -23.47593901973090880, -1.443836447538997092 ) ) ;
#3994 = B_SPLINE_CURVE_WITH_KNOTS ( 'NONE', 3,
 ( #61095, #16393, #69189, #31122, #30122, #70193, #100109, #7787, #21999, #38732 ),
 .UNSPECIFIED., .F., .F.,
 ( 4, 2, 2, 2, 4 ),
 ( 0.002505011693330810862, 0.003215057662361453343, 0.003925103631392095824, 0.004635149600422737437, 0.005345195569453379918 ),
 .UNSPECIFIED. ) ;
#3995 = VECTOR ( 'NONE', #34910, 1000.000000000000000 ) ;
#3996 = CARTESIAN_POINT ( 'NONE',  ( -52.62287095715005592, -23.47593901973091235, -1.443836447539009749 ) ) ;
#3997 = FACE_OUTER_BOUND ( 'NONE', #50876, .T. ) ;
#3998 = CARTESIAN_POINT ( 'NONE',  ( 0.003323472525107682655, -21.86402403546210493, 11.49999999999998934 ) ) ;
#3999 = DIRECTION ( 'NONE',  ( 3.773278334444167608E-23, -1.000000000000000000, 0.000000000000000000 ) ) ;
#4000 = DIRECTION ( 'NONE',  ( -1.000000000000000000, -0.000000000000000000, -0.000000000000000000 ) ) ;
#4001 = CYLINDRICAL_SURFACE ( 'NONE', #66332, 7.652410033082762020 ) ;
#4002 = CARTESIAN_POINT ( 'NONE',  ( -58.54815136844473500, -24.15543982623907482, -0.2315651400026660645 ) ) ;
#4003 = ORIENTED_EDGE ( 'NONE', *, *, #51609, .F. ) ;
#4004 = CARTESIAN_POINT ( 'NONE',  ( 5.143668500415711442, -19.74887971880038151, 11.49999999999998934 ) ) ;
#4005 = ORIENTED_EDGE ( 'NONE', *, *, #85862, .F. ) ;
#4006 = VERTEX_POINT ( 'NONE', #94718 ) ;
#4007 = ORIENTED_EDGE ( 'NONE', *, *, #63217, .F. ) ;
#4008 = ORIENTED_EDGE ( 'NONE', *, *, #38247, .T. ) ;
#4009 = CARTESIAN_POINT ( 'NONE',  ( -22.55714481399219906, -4.634528848986672500, -1.500000000000002220 ) ) ;
#4010 = CARTESIAN_POINT ( 'NONE',  ( -79.62287095715005592, -29.50250243563736774, 8.947779886222141599 ) ) ;
#4011 = CARTESIAN_POINT ( 'NONE',  ( 5.087728227403598424, 19.53446797131710611, -1.500000000000002220 ) ) ;
#4012 = ORIENTED_EDGE ( 'NONE', *, *, #1046, .T. ) ;
#4013 = ADVANCED_FACE ( 'NONE', ( #77481 ), #62799, .F. ) ;
#4014 = CARTESIAN_POINT ( 'NONE',  ( -97.62287095715005592, -23.48783264082478794, -1.443836473390061936 ) ) ;
#4015 = LINE ( 'NONE', #65438, #4459 ) ;
#4016 = CARTESIAN_POINT ( 'NONE',  ( -95.54220411708793392, -25.00158670708911046, 2.256160236439221034 ) ) ;
#4017 = CARTESIAN_POINT ( 'NONE',  ( -117.6228709571500559, -29.50250243563736774, 8.947779886222134493 ) ) ;
#4019 = ORIENTED_EDGE ( 'NONE', *, *, #52185, .T. ) ;
#4018 = CARTESIAN_POINT ( 'NONE',  ( 16.75108703964928480, -13.32659110743468212, 11.49999999999999645 ) ) ;
#4020 = PLANE ( 'NONE',  #56605 ) ;
#4021 = ORIENTED_EDGE ( 'NONE', *, *, #58225, .F. ) ;
#4022 = CARTESIAN_POINT ( 'NONE',  ( -16.22183044023116238, -15.26045173261249310, 11.49999999999998934 ) ) ;
#4023 = CARTESIAN_POINT ( 'NONE',  ( 15.58315679939408582, 13.61395703526229894, -1.500000000000002220 ) ) ;
#4024 = ADVANCED_FACE ( 'NONE', ( #86108 ), #15588, .T. ) ;
#4025 = AXIS2_PLACEMENT_3D ( 'NONE', #46041, #54159, #21670 ) ;
#4026 = ORIENTED_EDGE ( 'NONE', *, *, #83778, .F. ) ;
#4027 = EDGE_CURVE ( 'NONE', #25694, #21553, #16240, .T. ) ;
#4028 = CARTESIAN_POINT ( 'NONE',  ( 3.749014282529493869, -5.876774720514404748, 18.52125941707705792 ) ) ;
#4029 = EDGE_LOOP ( 'NONE', ( #99891, #378, #100236, #49073 ) ) ;
#4030 = FACE_OUTER_BOUND ( 'NONE', #99357, .T. ) ;
#4031 = ORIENTED_EDGE ( 'NONE', *, *, #53751, .T. ) ;
#4032 = CARTESIAN_POINT ( 'NONE',  ( 5.851028665930490646, -3.316774720514426011, -27.43979700150094558 ) ) ;
#4033 = CARTESIAN_POINT ( 'NONE',  ( -15.18370147500227496, -14.46048895944246127, -1.500000000000002220 ) ) ;
#4034 = CARTESIAN_POINT ( 'NONE',  ( -12.54888962926113827, 17.92887824059606672, 11.49999999999999645 ) ) ;
#4035 = B_SPLINE_CURVE_WITH_KNOTS ( 'NONE', 3,
 ( #98516, #43753, #58490, #51868, #66617, #82305 ),
 .UNSPECIFIED., .F., .F.,
 ( 4, 2, 4 ),
 ( 1.570887131794176733E-05, 0.001396322306279756519, 0.002776935741241571502 ),
 .UNSPECIFIED. ) ;
#4036 = AXIS2_PLACEMENT_3D ( 'NONE', #48950, #57071, #80889 ) ;
#4037 = CARTESIAN_POINT ( 'NONE',  ( -73.50726928729523024, -24.15620529776628089, 10.23563542870660470 ) ) ;
#4038 = CARTESIAN_POINT ( 'NONE',  ( 12.90280524143238594, -18.44629484376132922, 11.49999999999998934 ) ) ;
#4039 = CARTESIAN_POINT ( 'NONE',  ( 19.40473180639871131, -7.901900427366274293, 11.49999999999998934 ) ) ;
#4040 = CARTESIAN_POINT ( 'NONE',  ( -38.49113028606867459, -24.34968618360933590, 0.1864209137778850278 ) ) ;
#4041 = CARTESIAN_POINT ( 'NONE',  ( -94.62287095715005592, -29.50250243563736774, 8.947779886222139822 ) ) ;
#4042 = PLANE ( 'NONE',  #9716 ) ;
#4043 = CARTESIAN_POINT ( 'NONE',  ( -68.62287095715005592, -23.47593901973091235, -1.443836447539006196 ) ) ;
#4044 = EDGE_LOOP ( 'NONE', ( #94980, #47371 ) ) ;
#4045 = ORIENTED_EDGE ( 'NONE', *, *, #94115, .T. ) ;
#4046 = ORIENTED_EDGE ( 'NONE', *, *, #12707, .F. ) ;
#4047 = CARTESIAN_POINT ( 'NONE',  ( -52.61349081655445303, -23.48783264082478439, -1.443836473390069708 ) ) ;
#4048 = ORIENTED_EDGE ( 'NONE', *, *, #4774, .F. ) ;
#4049 = CARTESIAN_POINT ( 'NONE',  ( -19.15072323977689095, -9.709862252083167888, -1.500000000000002220 ) ) ;
#4050 = PLANE ( 'NONE',  #81309 ) ;
#4051 = ORIENTED_EDGE ( 'NONE', *, *, #83710, .F. ) ;
#4052 = CARTESIAN_POINT ( 'NONE',  ( 20.77832821955112408, -3.674247523096572099, -1.500000000000002220 ) ) ;
#4053 = CARTESIAN_POINT ( 'NONE',  ( -23.62875734969026453, -6.143225279485574397, 24.50402280011862288 ) ) ;
#4054 = DIRECTION ( 'NONE',  ( -3.773278334453079618E-23, 0.9999999999976377785, 2.173523156925979975E-06 ) ) ;
#4055 = CARTESIAN_POINT ( 'NONE',  ( -50.52198862043362482, -23.48786465467240347, 11.44779295918255002 ) ) ;
#4056 = CARTESIAN_POINT ( 'NONE',  ( -80.88924702628075636, -25.30877091901892939, 4.592921212922877139 ) ) ;
#4057 = CARTESIAN_POINT ( 'NONE',  ( -129.5557415901027980, -24.51419770103158413, 9.386484678747176957 ) ) ;
#4058 = CARTESIAN_POINT ( 'NONE',  ( 18.18892703665305177, -12.56521834855340281, -1.500000000000002220 ) ) ;
#4059 = ORIENTED_EDGE ( 'NONE', *, *, #25399, .T. ) ;
#4060 = CARTESIAN_POINT ( 'NONE',  ( -109.5948960647422581, -25.14264220134220196, 6.986250900936221697 ) ) ;
#4061 = DIRECTION ( 'NONE',  ( 2.710505431213760099E-16, -1.000000000000000000, 0.000000000000000000 ) ) ;
#4062 = CARTESIAN_POINT ( 'NONE',  ( -41.71489324084514294, -25.31624590159391985, 4.846374443859488679 ) ) ;
#4063 = EDGE_CURVE ( 'NONE', #63440, #86142, #15291, .T. ) ;
#4064 = CARTESIAN_POINT ( 'NONE',  ( -26.94960779665208861, -25.02909261677565311, 3.798368663089755515 ) ) ;
#4065 = VECTOR ( 'NONE', #35172, 1000.000000000000114 ) ;
#4066 = CARTESIAN_POINT ( 'NONE',  ( -102.5228709571500900, -23.47593901973090524, -1.443836447538996648 ) ) ;
#4067 = CARTESIAN_POINT ( 'NONE',  ( 20.50650179695670872, -5.950058665555418180, 11.49999999999998934 ) ) ;
#4068 = CARTESIAN_POINT ( 'NONE',  ( -69.07465920187155461, -25.18135671409043397, 6.806830623293391724 ) ) ;
#4069 = CARTESIAN_POINT ( 'NONE',  ( -66.62287095715005592, -24.64898659630367916, 1.056161002820824368 ) ) ;
#4070 = CARTESIAN_POINT ( 'NONE',  ( -84.55620429048337883, -24.66019654487199730, 8.947790411086124607 ) ) ;
#4071 = DIRECTION ( 'NONE',  ( 0.000000000000000000, -0.000000000000000000, 1.000000000000000000 ) ) ;
#4072 = CARTESIAN_POINT ( 'NONE',  ( 17.82461400791848405, -13.82690402418615960, -1.500000000000002220 ) ) ;
#4073 = CARTESIAN_POINT ( 'NONE',  ( -102.5228709571501042, -23.96127896942128999, -0.6493128930940196275 ) ) ;
#4074 = ORIENTED_EDGE ( 'NONE', *, *, #28569, .T. ) ;
#4075 = DIRECTION ( 'NONE',  ( -3.773278334444166432E-23, 1.000000000000000000, 0.000000000000000000 ) ) ;
#4076 = CARTESIAN_POINT ( 'NONE',  ( -79.55429618991367136, -23.96119346886880308, -0.6495511937832122440 ) ) ;
#4077 = CARTESIAN_POINT ( 'NONE',  ( 12.09797951242163805, 15.59582292391970704, 11.49999999999999645 ) ) ;
#4078 = CARTESIAN_POINT ( 'NONE',  ( -82.62287095715005592, -23.72773821059536559, 11.05748984161097503 ) ) ;
#4079 = EDGE_CURVE ( 'NONE', #54223, #78100, #72975, .T. ) ;
#4080 = CARTESIAN_POINT ( 'NONE',  ( -67.54036089741288151, -24.51314013834315375, 0.6176544820404126224 ) ) ;
#4081 = ORIENTED_EDGE ( 'NONE', *, *, #15057, .F. ) ;
#4082 = DIRECTION ( 'NONE',  ( 0.000000000000000000, -0.9999999999976377785, -2.173523156925979975E-06 ) ) ;
#4083 = CARTESIAN_POINT ( 'NONE',  ( -29.40205842853959339, -25.26026517658197434, 2.693429348280085289 ) ) ;
#4084 = EDGE_CURVE ( 'NONE', #16907, #74034, #58912, .T. ) ;
#4085 = CARTESIAN_POINT ( 'NONE',  ( -75.52287095715006160, -24.15516710230293640, 10.28746687063726029 ) ) ;
#4086 = CARTESIAN_POINT ( 'NONE',  ( -9.004746288917990782, -19.65190454534591069, -1.500000000000002220 ) ) ;
#4087 = CARTESIAN_POINT ( 'NONE',  ( -126.6228709571500843, -23.47596703998600631, 11.44779298504227860 ) ) ;
#4088 = PLANE ( 'NONE',  #46307 ) ;
#4089 = ADVANCED_FACE ( 'NONE', ( #71900, #39935 ), #47562, .T. ) ;
#4090 = CARTESIAN_POINT ( 'NONE',  ( -92.62287095715005592, -23.48783264082479150, -1.443836473390063713 ) ) ;
#4091 = CARTESIAN_POINT ( 'NONE',  ( -90.62287095715004170, -29.50248789122583659, 2.256150453626215580 ) ) ;
#4092 = CARTESIAN_POINT ( 'NONE',  ( -6.431973572030615038, 18.70533856667250916, 11.49999999999998934 ) ) ;
#4093 = ORIENTED_EDGE ( 'NONE', *, *, #26438, .T. ) ;
#4094 = EDGE_CURVE ( 'NONE', #55468, #17140, #46873, .T. ) ;
#4095 = CARTESIAN_POINT ( 'NONE',  ( -12.33117494125061242, 16.09929768045241261, 11.49999999999999645 ) ) ;
#4096 = LINE ( 'NONE', #59377, #58608 ) ;
#4097 = EDGE_CURVE ( 'NONE', #73872, #803, #66293, .T. ) ;
#4098 = VECTOR ( 'NONE', #90810, 1000.000000000000000 ) ;
#4099 = CARTESIAN_POINT ( 'NONE',  ( -43.62287095715004170, -23.48786465467241058, 11.44779295918255180 ) ) ;
#4100 = ORIENTED_EDGE ( 'NONE', *, *, #89703, .T. ) ;
#4101 = LINE ( 'NONE', #43660, #65370 ) ;
#4102 = CARTESIAN_POINT ( 'NONE',  ( -28.47875734969025885, -5.965225279485572685, -0.08597719988137300651 ) ) ;
#4103 = DIRECTION ( 'NONE',  ( 1.000000000000000000, 3.773278334444166432E-23, 8.201307841325785021E-29 ) ) ;
#4104 = CARTESIAN_POINT ( 'NONE',  ( -52.58953762381672448, -24.64898659630367561, 1.056161002820380723 ) ) ;
#4105 = PLANE ( 'NONE',  #93204 ) ;
#4106 = CARTESIAN_POINT ( 'NONE',  ( -8.782848147209532996, 18.00178819457707746, 11.49999999999998934 ) ) ;
#4107 = EDGE_CURVE ( 'NONE', #11869, #3328, #20089, .T. ) ;
#4108 = AXIS2_PLACEMENT_3D ( 'NONE', #51961, #22472, #30101 ) ;
#4109 = DIRECTION ( 'NONE',  ( 0.000000000000000000, 0.000000000000000000, -1.000000000000000000 ) ) ;
#4110 = ORIENTED_EDGE ( 'NONE', *, *, #90775, .F. ) ;
#4111 = CIRCLE ( 'NONE', #96450, 129.7684398600581517 ) ;
#4112 = CARTESIAN_POINT ( 'NONE',  ( -51.52287095715006870, -24.51283580621365132, 0.6167428607019705966 ) ) ;
#4113 = CARTESIAN_POINT ( 'NONE',  ( -115.5895376238166961, -23.48783264082478794, -1.443836473390058384 ) ) ;
#4114 = FACE_OUTER_BOUND ( 'NONE', #25491, .T. ) ;
#4115 = CARTESIAN_POINT ( 'NONE',  ( -105.5228709571500616, -24.62226745350437440, 0.9660975649728157366 ) ) ;
#4116 = CARTESIAN_POINT ( 'NONE',  ( -73.54547332343318544, -24.34968618360933590, 0.1864209137778806424 ) ) ;
#4117 = DIRECTION ( 'NONE',  ( -0.9951627101165076983, 0.000000000000000000, 0.09824042138329588947 ) ) ;
#4118 = CARTESIAN_POINT ( 'NONE',  ( -51.53971197011429695, -25.29440776045720085, 5.833784451200526355 ) ) ;
#4119 = ORIENTED_EDGE ( 'NONE', *, *, #97259, .T. ) ;
#4120 = CARTESIAN_POINT ( 'NONE',  ( 12.41260344771940360, 16.11316662856288318, 11.49999999999998934 ) ) ;
#4121 = ORIENTED_EDGE ( 'NONE', *, *, #69016, .T. ) ;
#4122 = EDGE_CURVE ( 'NONE', #40241, #59933, #10481, .T. ) ;
#4123 = CARTESIAN_POINT ( 'NONE',  ( -22.60589916338503613, 3.847557683979087706, 11.49999999999998934 ) ) ;
#4124 = CARTESIAN_POINT ( 'NONE',  ( 31.64388307978944326, 6.098167052574009261, 27.71102684943996053 ) ) ;
#4125 = ORIENTED_EDGE ( 'NONE', *, *, #31913, .T. ) ;
#4126 = CARTESIAN_POINT ( 'NONE',  ( -89.58953762381671027, -23.48783264082478439, -1.443836473390063713 ) ) ;
#4128 = ADVANCED_FACE ( 'NONE', ( #18100 ), #72899, .T. ) ;
#4127 = CARTESIAN_POINT ( 'NONE',  ( -49.58282627629191808, -25.26264116536357562, 6.816471629502625973 ) ) ;
#4129 = CARTESIAN_POINT ( 'NONE',  ( 26.73860345374794178, -1.477225279485574028, 19.84760796525321780 ) ) ;
#4130 = CARTESIAN_POINT ( 'NONE',  ( -21.01389645921736360, -2.595061309317715281, 11.49999999999999645 ) ) ;
#4131 = VECTOR ( 'NONE', #52772, 1000.000000000000000 ) ;
#4132 = CARTESIAN_POINT ( 'NONE',  ( -19.06252244145942498, 11.34236556261432405, 11.49999999999998934 ) ) ;
#4133 = EDGE_CURVE ( 'NONE', #81499, #82077, #4878, .T. ) ;
#4134 = CARTESIAN_POINT ( 'NONE',  ( 18.07347782881280907, 9.871946371954690491, -1.500000000000002220 ) ) ;
#4135 = ORIENTED_EDGE ( 'NONE', *, *, #31925, .F. ) ;
#4136 = LINE ( 'NONE', #26964, #45818 ) ;
#4137 = ORIENTED_EDGE ( 'NONE', *, *, #99840, .T. ) ;
#4138 = PLANE ( 'NONE',  #67344 ) ;
#4139 = EDGE_CURVE ( 'NONE', #24485, #7104, #74380, .T. ) ;
#4140 = CARTESIAN_POINT ( 'NONE',  ( -50.52287095715006160, -23.47596703998600631, 11.44779298504229104 ) ) ;
#4141 = ORIENTED_EDGE ( 'NONE', *, *, #65545, .T. ) ;
#4142 = EDGE_LOOP ( 'NONE', ( #60180, #79891, #545, #99105 ) ) ;
#4143 = ORIENTED_EDGE ( 'NONE', *, *, #27740, .F. ) ;
#4144 = DIRECTION ( 'NONE',  ( 1.000000000000000000, 0.000000000000000000, 0.000000000000000000 ) ) ;
#4145 = CARTESIAN_POINT ( 'NONE',  ( -28.56161880046136758, -23.57756926196503855, 11.05961558438220926 ) ) ;
#4146 = CARTESIAN_POINT ( 'NONE',  ( 14.74815398954873835, -3.719725396296209574, -28.39563063676373389 ) ) ;
#4147 = CARTESIAN_POINT ( 'NONE',  ( -8.119355292522030254, -19.11072509857415369, -1.500000000000002220 ) ) ;
#4149 = EDGE_CURVE ( 'NONE', #89671, #89470, #81503, .T. ) ;
#4148 = CARTESIAN_POINT ( 'NONE',  ( 20.57166443188586769, -7.073620337204646447, 11.49999999999999645 ) ) ;
#4150 = ORIENTED_EDGE ( 'NONE', *, *, #71672, .F. ) ;
#4151 = CARTESIAN_POINT ( 'NONE',  ( -6.660000000000001030, 0.000000000000000000, 0.000000000000000000 ) ) ;
#4152 = CARTESIAN_POINT ( 'NONE',  ( -115.5143242223860653, -24.83618233451450408, 1.606449574219536824 ) ) ;
#4153 = CARTESIAN_POINT ( 'NONE',  ( -14.39434090420295220, 17.20869321163716492, 11.49999999999998934 ) ) ;
#4154 = CARTESIAN_POINT ( 'NONE',  ( -33.58953762381673158, -24.64965694238406613, 8.947790433994663672 ) ) ;
#4155 = DIRECTION ( 'NONE',  ( 0.000000000000000000, -1.000000000000000000, 0.000000000000000000 ) ) ;
#4156 = ORIENTED_EDGE ( 'NONE', *, *, #81969, .F. ) ;
#4157 = CARTESIAN_POINT ( 'NONE',  ( -61.52287095715007581, -23.48783264082476308, -1.443836473390092356 ) ) ;
#4158 = DIRECTION ( 'NONE',  ( -1.000000000000000000, -0.000000000000000000, -0.000000000000000000 ) ) ;
#4159 = EDGE_LOOP ( 'NONE', ( #44449, #40971, #10628, #75618 ) ) ;
#4160 = VERTEX_POINT ( 'NONE', #66797 ) ;
#4161 = CARTESIAN_POINT ( 'NONE',  ( -69.62287095715005592, -24.35013146730203459, 9.818937971375111928 ) ) ;
#4162 = CC_DESIGN_PERSON_AND_ORGANIZATION_ASSIGNMENT ( #30655, #77803, ( #34420 ) ) ;
#4163 = EDGE_LOOP ( 'NONE', ( #2096, #85260, #54188, #12523 ) ) ;
#4164 = VECTOR ( 'NONE', #1261, 1000.000000000000000 ) ;
#4165 = CARTESIAN_POINT ( 'NONE',  ( -21.25539211000977957, 0.9166567589900279645, -1.500000000000002220 ) ) ;
#4166 = VERTEX_POINT ( 'NONE', #97716 ) ;
#4167 = CARTESIAN_POINT ( 'NONE',  ( -88.56233851268359558, -23.48783264082476663, -1.443836473390093467 ) ) ;
#4168 = CARTESIAN_POINT ( 'NONE',  ( -6.661741538832703036, 20.79550341630197607, 11.49999999999998934 ) ) ;
#4169 = CARTESIAN_POINT ( 'NONE',  ( -38.52287095715006870, -24.64965694238406613, 8.947790433994205372 ) ) ;
#4170 = CARTESIAN_POINT ( 'NONE',  ( -19.30582015231555104, -11.89196067722419237, -1.500000000000002220 ) ) ;
#4171 = CARTESIAN_POINT ( 'NONE',  ( -112.5562042904834072, -24.65952944569304961, 1.056160979905706565 ) ) ;
#4172 = VECTOR ( 'NONE', #89910, 1000.000000000000000 ) ;
#4173 = DIRECTION ( 'NONE',  ( -3.773278334453079618E-23, 0.9999999999976377785, 2.173523156925978705E-06 ) ) ;
#4174 = CARTESIAN_POINT ( 'NONE',  ( -3.281320334969873631, 21.64054093270537393, -1.500000000000002220 ) ) ;
#4175 = CARTESIAN_POINT ( 'NONE',  ( 6.763596848542221984, -6.376774720514426065, 21.40271460634751577 ) ) ;
#4176 = VERTEX_POINT ( 'NONE', #80495 ) ;
#4177 = CARTESIAN_POINT ( 'NONE',  ( 25.02738304948465853, 5.067934468345774768, -9.480319778648102158 ) ) ;
#4178 = DIRECTION ( 'NONE',  ( -1.000000000000000000, -0.000000000000000000, -0.000000000000000000 ) ) ;
#4179 = AXIS2_PLACEMENT_3D ( 'NONE', #81109, #3501, #49187 ) ;
#4180 = AXIS2_PLACEMENT_3D ( 'NONE', #71005, #2492, #1495 ) ;
#4181 = ORIENTED_EDGE ( 'NONE', *, *, #95955, .T. ) ;
#4182 = DIRECTION ( 'NONE',  ( 0.000000000000000000, 1.000000000000000000, -0.000000000000000000 ) ) ;
#4183 = ORIENTED_EDGE ( 'NONE', *, *, #42918, .F. ) ;
#4184 = CARTESIAN_POINT ( 'NONE',  ( 30.53060340732035982, -4.594240983522013266, 19.84760796525321425 ) ) ;
#4185 = CARTESIAN_POINT ( 'NONE',  ( -30.63911803361059683, -23.78088414657023719, -0.9709657327914291702 ) ) ;
#4186 = CARTESIAN_POINT ( 'NONE',  ( -0.06837171988653999166, -21.26218376953697486, -1.500000000000002220 ) ) ;
#4187 = DIRECTION ( 'NONE',  ( 0.000000000000000000, 0.000000000000000000, 1.000000000000000000 ) ) ;
#4188 = CARTESIAN_POINT ( 'NONE',  ( -27.08002768120591242, -24.97064435294952389, 2.428018831443120806 ) ) ;
#4189 = CARTESIAN_POINT ( 'NONE',  ( -85.58227612371159410, -24.92564183028979130, 1.928384488918251982 ) ) ;
#4190 = DIRECTION ( 'NONE',  ( -1.000000000000000000, -3.773278334444167020E-23, -8.201307811038811694E-29 ) ) ;
#4191 = CARTESIAN_POINT ( 'NONE',  ( -79.62287095715004170, -23.72773821059535848, 11.05748984161097681 ) ) ;
#4192 = ORIENTED_EDGE ( 'NONE', *, *, #19918, .F. ) ;
#4193 = CARTESIAN_POINT ( 'NONE',  ( 18.95637782189878706, 4.751392969308117387, 11.49999999999999645 ) ) ;
#4194 = CARTESIAN_POINT ( 'NONE',  ( -99.36664296761678372, -25.31172790992623689, 4.689206871853577319 ) ) ;
#4195 = EDGE_CURVE ( 'NONE', #11900, #54673, #40757, .T. ) ;
#4196 = CARTESIAN_POINT ( 'NONE',  ( -27.79920052361254079, -24.64785536601324978, 8.250242701940406320 ) ) ;
#4197 = ORIENTED_EDGE ( 'NONE', *, *, #32957, .T. ) ;
#4198 = CARTESIAN_POINT ( 'NONE',  ( -71.62287095715005592, -29.50250786944525672, 11.44777988621623699 ) ) ;
#4199 = CARTESIAN_POINT ( 'NONE',  ( -99.53504363246379683, -25.31439613239528441, 5.566583519096571564 ) ) ;
#4200 = CARTESIAN_POINT ( 'NONE',  ( -51.62287095715005592, -23.48783264082478084, -1.443836473390070596 ) ) ;
#4201 = CARTESIAN_POINT ( 'NONE',  ( -80.55728237399675606, -25.03156060684649731, 7.562285999033727890 ) ) ;
#4202 = CARTESIAN_POINT ( 'NONE',  ( -5.193715590271882121, 18.98282465337476665, -1.500000000000002220 ) ) ;
#4203 = VERTEX_POINT ( 'NONE', #88617 ) ;
#4204 = EDGE_CURVE ( 'NONE', #1307, #36594, #62505, .T. ) ;
#4205 = CARTESIAN_POINT ( 'NONE',  ( -5.366453405989236813, 0.000000000000000000, 0.000000000000000000 ) ) ;
#4206 = CARTESIAN_POINT ( 'NONE',  ( 3.025806405283164136, -5.876774720514420736, 20.84867811309776542 ) ) ;
#4207 = ADVANCED_FACE ( 'NONE', ( #42456 ), #27715, .F. ) ;
#4208 = PERSON_AND_ORGANIZATION_ROLE ( 'classification_officer' ) ;
#4209 = EDGE_LOOP ( 'NONE', ( #89853, #44560, #96420, #94817 ) ) ;
#4210 = LINE ( 'NONE', #82323, #79172 ) ;
#4211 = DIRECTION ( 'NONE',  ( 1.000000000000000000, 3.773278334444167608E-23, 8.201307833595939069E-29 ) ) ;
#4212 = CARTESIAN_POINT ( 'NONE',  ( -55.60865610405180348, -23.85016227208578954, -0.8807180028928371929 ) ) ;
#4213 = CARTESIAN_POINT ( 'NONE',  ( -118.6277876297057929, -23.73766607897671221, -1.055555164236448684 ) ) ;
#4214 = CARTESIAN_POINT ( 'NONE',  ( -79.91782308976125648, -25.27183487616304447, 3.712349674769177543 ) ) ;
#4215 = B_SPLINE_CURVE_WITH_KNOTS ( 'NONE', 3,
 ( #33255, #2826, #33765, #64748, #78422, #95665 ),
 .UNSPECIFIED., .F., .F.,
 ( 4, 2, 4 ),
 ( 0.000000000000000000, 0.001380901958385388545, 0.002761803916770777089 ),
 .UNSPECIFIED. ) ;
#4216 = DIRECTION ( 'NONE',  ( 0.000000000000000000, 1.000000000000000000, 0.000000000000000000 ) ) ;
#4217 = CARTESIAN_POINT ( 'NONE',  ( -79.52287095715003318, -23.73907113216989728, -1.053371485793251905 ) ) ;
#4218 = CARTESIAN_POINT ( 'NONE',  ( 14.81759351585047391, 13.34335055255382052, -1.500000000000002220 ) ) ;
#4219 = ADVANCED_FACE ( 'NONE', ( #4385 ), #14943, .T. ) ;
#4220 = CARTESIAN_POINT ( 'NONE',  ( -0.04029912359210763989, -22.52829617641010174, 1.476849900881732625 ) ) ;
#4221 = CARTESIAN_POINT ( 'NONE',  ( 3.219775368129482285, -19.64489633315863770, -1.500000000000002220 ) ) ;
#4222 = EDGE_LOOP ( 'NONE', ( #71909, #90635, #30018, #33362 ) ) ;
#4223 = PLANE ( 'NONE',  #11887 ) ;
#4224 = AXIS2_PLACEMENT_3D ( 'NONE', #90568, #21539, #27184 ) ;
#4225 = DIRECTION ( 'NONE',  ( 0.000000000000000000, 0.000000000000000000, 1.000000000000000000 ) ) ;
#4226 = LINE ( 'NONE', #95569, #43080 ) ;
#4227 = CARTESIAN_POINT ( 'NONE',  ( 7.822518687475809251, -6.376774720513926908, -28.18023264526767591 ) ) ;
#4228 = CARTESIAN_POINT ( 'NONE',  ( -37.52287095715006870, -23.47593901973090524, -1.443836447538997314 ) ) ;
#4229 = CARTESIAN_POINT ( 'NONE',  ( -7.603582339867426043, -5.876774720514417183, 19.86545874326176175 ) ) ;
#4230 = CARTESIAN_POINT ( 'NONE',  ( -51.29572949068491994, -25.25925092192675336, 3.940762572495089877 ) ) ;
#4231 = VECTOR ( 'NONE', #20082, 1000.000000000000000 ) ;
#4232 = ORIENTED_EDGE ( 'NONE', *, *, #24748, .F. ) ;
#4233 = CARTESIAN_POINT ( 'NONE',  ( -46.52287095715007581, -23.48783264082477018, -1.443836473390096797 ) ) ;
#4235 = VECTOR ( 'NONE', #45100, 1000.000000000000114 ) ;
#4234 = DIRECTION ( 'NONE',  ( -3.773278334444166432E-23, 1.000000000000000000, 0.000000000000000000 ) ) ;
#4236 = ORIENTED_EDGE ( 'NONE', *, *, #66303, .T. ) ;
#4237 = VECTOR ( 'NONE', #27548, 1000.000000000000000 ) ;
#4238 = CARTESIAN_POINT ( 'NONE',  ( 15.69265952521009488, -12.80212094623039576, -1.500000000000002220 ) ) ;
#4239 = ADVANCED_FACE ( 'NONE', ( #67791 ), #99997, .T. ) ;
#4240 = CARTESIAN_POINT ( 'NONE',  ( -122.5906892859157296, -23.96119346886880663, -0.6495511937832028071 ) ) ;
#4241 = CIRCLE ( 'NONE', #60965, 1.306876713926001354 ) ;
#4242 = CARTESIAN_POINT ( 'NONE',  ( -117.6228709571500559, -29.50248528299804818, 1.056150453629045360 ) ) ;
#4243 = VECTOR ( 'NONE', #57659, 1000.000000000000000 ) ;
#4244 = DIRECTION ( 'NONE',  ( -1.000000000000000000, 5.782411586589363555E-16, 0.000000000000000000 ) ) ;
#4245 = EDGE_LOOP ( 'NONE', ( #81772, #48382, #5113, #11906 ) ) ;
#4247 = EDGE_CURVE ( 'NONE', #10125, #59687, #57317, .T. ) ;
#4246 = CARTESIAN_POINT ( 'NONE',  ( -78.94303308397304875, -25.27645460285955181, 5.977536667781793156 ) ) ;
#4248 = CARTESIAN_POINT ( 'NONE',  ( -2.104002878010082789, -6.376774720514410077, 19.15289935703627222 ) ) ;
#4249 = CARTESIAN_POINT ( 'NONE',  ( 12.85705330080557829, 15.37097598829428513, -1.500000000000002220 ) ) ;
#4250 = CARTESIAN_POINT ( 'NONE',  ( 8.881738082190086203, 19.07353979602852689, 11.49999999999999645 ) ) ;
#4251 = CARTESIAN_POINT ( 'NONE',  ( 30.54789914928607786, 0.2637885907592373291, 23.75907673500034178 ) ) ;
#4252 = FACE_OUTER_BOUND ( 'NONE', #72560, .T. ) ;
#4253 = CARTESIAN_POINT ( 'NONE',  ( -19.90388773112789167, 9.559999800501117306, -1.500000000000002220 ) ) ;
#4254 = ADVANCED_FACE ( 'NONE', ( #74869 ), #5371, .T. ) ;
#4255 = CARTESIAN_POINT ( 'NONE',  ( -2.701720430790308214, 0.3587747205144061202, -28.90526747363640681 ) ) ;
#4256 = EDGE_CURVE ( 'NONE', #13507, #59016, #5710, .T. ) ;
#4257 = CARTESIAN_POINT ( 'NONE',  ( -34.52287095715006160, -23.47593901973090169, -1.443836447538997314 ) ) ;
#4258 = DIRECTION ( 'NONE',  ( 0.000000000000000000, 1.000000000000000000, -0.000000000000000000 ) ) ;
#4259 = ORIENTED_EDGE ( 'NONE', *, *, #66341, .T. ) ;
#4260 = FACE_OUTER_BOUND ( 'NONE', #62954, .T. ) ;
#4261 = CARTESIAN_POINT ( 'NONE',  ( -31.52200039736317905, -23.48783264082477018, -1.443836473390079256 ) ) ;
#4262 = ORIENTED_EDGE ( 'NONE', *, *, #94255, .F. ) ;
#4263 = ORIENTED_EDGE ( 'NONE', *, *, #37712, .T. ) ;
#4264 = LINE ( 'NONE', #96113, #34053 ) ;
#4265 = CARTESIAN_POINT ( 'NONE',  ( -72.52287095715007581, -23.48786465467241058, 11.44779295918254647 ) ) ;
#4266 = DIRECTION ( 'NONE',  ( -0.000000000000000000, 2.173523156925979552E-06, -0.9999999999976378895 ) ) ;
#4267 = CARTESIAN_POINT ( 'NONE',  ( 13.11803791274172681, -15.88952355948706341, -1.500000000000002220 ) ) ;
#4268 = CARTESIAN_POINT ( 'NONE',  ( 13.04721882220160012, 17.14300067834640373, 11.49999999999999645 ) ) ;
#4269 = ORIENTED_EDGE ( 'NONE', *, *, #44279, .T. ) ;
#4270 = DIRECTION ( 'NONE',  ( 0.000000000000000000, -2.173523156925979552E-06, 0.9999999999976378895 ) ) ;
#4271 = DIRECTION ( 'NONE',  ( 0.000000000000000000, 0.000000000000000000, -1.000000000000000000 ) ) ;
#4272 = VECTOR ( 'NONE', #62106, 1000.000000000000000 ) ;
#4273 = FACE_OUTER_BOUND ( 'NONE', #52947, .T. ) ;
#4274 = CARTESIAN_POINT ( 'NONE',  ( -19.39139147909919458, -11.06001032434818576, -1.500000000000002220 ) ) ;
#4275 = LINE ( 'NONE', #96123, #38371 ) ;
#4276 = DIRECTION ( 'NONE',  ( -3.773278334453079030E-23, 0.9999999999976377785, 2.173523156925979128E-06 ) ) ;
#4277 = EDGE_LOOP ( 'NONE', ( #61982, #70823, #62189, #19666 ) ) ;
#4278 = CARTESIAN_POINT ( 'NONE',  ( -43.52287095715006160, -24.65952944569304606, 1.056160979905691910 ) ) ;
#4279 = CARTESIAN_POINT ( 'NONE',  ( 3.362030615038681169, -5.876774720514424288, 21.34376340489846413 ) ) ;
#4280 = CARTESIAN_POINT ( 'NONE',  ( 19.93353245626563819, -6.116835970281883306, 11.49999999999998934 ) ) ;
#4281 = EDGE_LOOP ( 'NONE', ( #96717, #61180, #94863, #96240 ) ) ;
#4283 = VERTEX_POINT ( 'NONE', #41705 ) ;
#4282 = CARTESIAN_POINT ( 'NONE',  ( 15.32643653063178668, -3.582999323269832725, -27.14485409495428314 ) ) ;
#4284 = ADVANCED_FACE ( 'NONE', ( #7858 ), #30698, .T. ) ;
#4285 = ORIENTED_EDGE ( 'NONE', *, *, #88332, .F. ) ;
#4286 = CARTESIAN_POINT ( 'NONE',  ( -100.5441709467755800, -25.00182538069147142, 7.747789668545045139 ) ) ;
#4287 = CARTESIAN_POINT ( 'NONE',  ( -13.19772682967519195, -16.48504770976277101, -1.500000000000002220 ) ) ;
#4288 = ORIENTED_EDGE ( 'NONE', *, *, #64688, .T. ) ;
#4289 = CARTESIAN_POINT ( 'NONE',  ( -114.6228709571500701, -23.47596703998600631, 11.44779298504227860 ) ) ;
#4290 = CARTESIAN_POINT ( 'NONE',  ( -49.30576173963486752, -25.30390373665932913, 5.218538515028145142 ) ) ;
#4291 = CARTESIAN_POINT ( 'NONE',  ( -120.5543829380116989, -24.40133493613049964, 9.663955038902800609 ) ) ;
#4292 = EDGE_CURVE ( 'NONE', #90746, #28117, #65053, .T. ) ;
#4293 = CARTESIAN_POINT ( 'NONE',  ( -81.26889613615777819, -25.31615098280113685, 4.442621364743881252 ) ) ;
#4294 = DIRECTION ( 'NONE',  ( 0.000000000000000000, -2.173523156925980399E-06, 0.9999999999976378895 ) ) ;
#4295 = CARTESIAN_POINT ( 'NONE',  ( -15.83346750871019992, -14.79491179806518630, -1.500000000000002220 ) ) ;
#4296 = CARTESIAN_POINT ( 'NONE',  ( -81.47155790579010670, -25.12224225815649348, 6.336855834686440758 ) ) ;
#4298 = ORIENTED_EDGE ( 'NONE', *, *, #92745, .F. ) ;
#4297 = CARTESIAN_POINT ( 'NONE',  ( 19.02167141253037030, -11.55642654327076535, 11.49999999999999645 ) ) ;
#4299 = CARTESIAN_POINT ( 'NONE',  ( -72.62287095715005592, -23.73934037231756733, 11.05740245334329153 ) ) ;
#4300 = CARTESIAN_POINT ( 'NONE',  ( 0.4325450954222598288, 2.349999999999997868, 2.877919977996277362E-16 ) ) ;
#4301 = DIRECTION ( 'NONE',  ( 1.000000000000000000, 0.000000000000000000, 0.000000000000000000 ) ) ;
#4302 = ORIENTED_EDGE ( 'NONE', *, *, #8115, .F. ) ;
#4303 = EDGE_CURVE ( 'NONE', #87149, #18629, #39306, .T. ) ;
#4304 = EDGE_CURVE ( 'NONE', #31114, #24140, #93087, .T. ) ;
#4305 = VECTOR ( 'NONE', #46008, 1000.000000000000000 ) ;
#4307 = ORIENTED_EDGE ( 'NONE', *, *, #24780, .F. ) ;
#4306 = CARTESIAN_POINT ( 'NONE',  ( -19.77875734969026311, 5.356774720514425603, 27.31649921512899937 ) ) ;
#4308 = ORIENTED_EDGE ( 'NONE', *, *, #66413, .T. ) ;
#4309 = CARTESIAN_POINT ( 'NONE',  ( -74.62287095715005592, -29.50247984919015209, -1.443849546365055359 ) ) ;
#4310 = DIRECTION ( 'NONE',  ( -0.000000000000000000, 1.000000000000000000, -0.000000000000000000 ) ) ;
#4311 = CARTESIAN_POINT ( 'NONE',  ( 16.04662828278931741, -3.608091531752042336, -27.86986495919489215 ) ) ;
#4312 = AXIS2_PLACEMENT_3D ( 'NONE', #70618, #85842, #47790 ) ;
#4313 = CARTESIAN_POINT ( 'NONE',  ( -35.52287095715006870, -23.47593901973090169, -1.443836447538997092 ) ) ;
#4314 = LINE ( 'NONE', #35266, #11762 ) ;
#4315 = ORIENTED_EDGE ( 'NONE', *, *, #4133, .F. ) ;
#4316 = VECTOR ( 'NONE', #60309, 1000.000000000000114 ) ;
#4317 = CARTESIAN_POINT ( 'NONE',  ( -69.52287095715006160, -24.50216790748203977, 0.6166512839542548363 ) ) ;
#4318 = CARTESIAN_POINT ( 'NONE',  ( 16.82713599508461400, -14.87465808564757808, -1.500000000000002220 ) ) ;
#4319 = AXIS2_PLACEMENT_3D ( 'NONE', #25092, #26103, #9874 ) ;
#4320 = EDGE_CURVE ( 'NONE', #19978, #30322, #65055, .T. ) ;
#4321 = VERTEX_POINT ( 'NONE', #69769 ) ;
#4322 = CARTESIAN_POINT ( 'NONE',  ( -100.2508004467732974, -25.04457302488155079, 7.556254356173342401 ) ) ;
#4323 = CARTESIAN_POINT ( 'NONE',  ( -101.6339336904412249, -23.73791477778911485, 11.05961554403170233 ) ) ;
#4324 = CARTESIAN_POINT ( 'NONE',  ( 9.405830370894557646, 5.356774720514425603, -24.99732136569351226 ) ) ;
#4325 = DIRECTION ( 'NONE',  ( -3.773278334453080206E-23, 0.9999999999976377785, 2.173523156925979975E-06 ) ) ;
#4326 = AXIS2_PLACEMENT_3D ( 'NONE', #68863, #30290, #53653 ) ;
#4327 = CARTESIAN_POINT ( 'NONE',  ( -130.5728709571501156, -25.30559561715418582, 6.147794833475641596 ) ) ;
#4328 = CARTESIAN_POINT ( 'NONE',  ( -11.77723790057865116, -15.68276428244051779, 11.49999999999998934 ) ) ;
#4329 = CARTESIAN_POINT ( 'NONE',  ( 8.971512145086521173, -7.528487854913501920, 4.500000000000000888 ) ) ;
#4330 = VERTEX_POINT ( 'NONE', #62666 ) ;
#4331 = CARTESIAN_POINT ( 'NONE',  ( 7.253797376210795456, 20.28272692992397808, 11.49999999999998934 ) ) ;
#4332 = CARTESIAN_POINT ( 'NONE',  ( -75.58953762381671027, -25.00182538069145011, 7.747789668545099317 ) ) ;
#4333 = CARTESIAN_POINT ( 'NONE',  ( -81.28341456819592281, -25.31572684435573706, 5.143804157612075656 ) ) ;
#4334 = CARTESIAN_POINT ( 'NONE',  ( -81.52287095715006160, -24.64965694238408034, 8.947790433994198267 ) ) ;
#4335 = CARTESIAN_POINT ( 'NONE',  ( 31.02038118199824268, -5.152774720514427642, -4.893189986691015569 ) ) ;
#4336 = CARTESIAN_POINT ( 'NONE',  ( 7.334040449947802465, -21.76207178258647090, -1.500000000000002220 ) ) ;
#4337 = EDGE_CURVE ( 'NONE', #22003, #43651, #51243, .T. ) ;
#4338 = EDGE_CURVE ( 'NONE', #1176, #5085, #10572, .T. ) ;
#4339 = DATE_AND_TIME ( #42903, #60286 ) ;
#4340 = PLANE ( 'NONE',  #27263 ) ;
#4341 = CARTESIAN_POINT ( 'NONE',  ( -49.54104479505958381, -24.34968618360933590, 0.1864209137778799485 ) ) ;
#4342 = CARTESIAN_POINT ( 'NONE',  ( 19.67429046578372365, -4.105084037421226739, 11.49999999999999645 ) ) ;
#4343 = DIRECTION ( 'NONE',  ( -1.000000000000000000, 7.960204194457801640E-17, 0.000000000000000000 ) ) ;
#4344 = CARTESIAN_POINT ( 'NONE',  ( -32.48282705711311280, -24.51419770103159834, 9.386484678747182286 ) ) ;
#4345 = CARTESIAN_POINT ( 'NONE',  ( -28.84663072490566194, -0.3587747205144265483, 28.73989617533406715 ) ) ;
#4346 = CARTESIAN_POINT ( 'NONE',  ( -113.5562042904833788, -23.48783264082479150, -1.443836473390060160 ) ) ;
#4347 = B_SPLINE_CURVE_WITH_KNOTS ( 'NONE', 3,
 ( #64406, #55276, #40547, #32928, #31423, #62380, #17698, #23291, #93819, #23801, #54775, #85711, #16190, #47159 ),
 .UNSPECIFIED., .F., .F.,
 ( 4, 2, 2, 2, 2, 2, 4 ),
 ( 0.000000000000000000, 0.0001869308316361848311, 0.0003738616632723696623, 0.0007477233265447393246, 0.001121584989817109041, 0.001308515821453293737, 0.001495446653089478649 ),
 .UNSPECIFIED. ) ;
#4348 = CARTESIAN_POINT ( 'NONE',  ( -28.98875734969026396, 5.965225279485572685, 2.362022800118626531 ) ) ;
#4349 = CARTESIAN_POINT ( 'NONE',  ( -16.82575997001036328, 10.57904039763333159, -1.500000000000002220 ) ) ;
#4350 = EDGE_CURVE ( 'NONE', #29179, #84363, #15406, .T. ) ;
#4351 = CARTESIAN_POINT ( 'NONE',  ( -94.52287095715006160, -23.47596703998600631, 11.44779298504228393 ) ) ;
#4352 = CARTESIAN_POINT ( 'NONE',  ( -13.19171355488933983, -14.64934158388261665, -1.500000000000002220 ) ) ;
#4353 = CIRCLE ( 'NONE', #43247, 253.2618649670780826 ) ;
#4354 = CARTESIAN_POINT ( 'NONE',  ( 16.15056352287345476, -3.622774720514426949, -27.77856273171767398 ) ) ;
#4355 = EDGE_CURVE ( 'NONE', #69249, #49812, #11726, .T. ) ;
#4356 = DESIGN_CONTEXT ( 'detailed design', #10995, 'design' ) ;
#4357 = CARTESIAN_POINT ( 'NONE',  ( -125.6228709571501838, -24.82576562982393398, 8.398263435472967942 ) ) ;
#4358 = DIRECTION ( 'NONE',  ( -0.8246584009594635223, 0.5656310827093757876, 0.000000000000000000 ) ) ;
#4359 = CARTESIAN_POINT ( 'NONE',  ( 17.37421522561336928, 11.14841987994331696, 11.49999999999999645 ) ) ;
#4360 = AXIS2_PLACEMENT_3D ( 'NONE', #48752, #86789, #47742 ) ;
#4362 = B_SPLINE_CURVE_WITH_KNOTS ( 'NONE', 3,
 ( #637, #86379, #8758, #61053 ),
 .UNSPECIFIED., .F., .F.,
 ( 4, 4 ),
 ( 0.000000000000000000, 0.0001000000000000028644 ),
 .UNSPECIFIED. ) ;
#4361 = DIRECTION ( 'NONE',  ( 0.000000000000000000, -1.000000000000000000, 0.000000000000000000 ) ) ;
#4363 = CARTESIAN_POINT ( 'NONE',  ( 22.61563695565308407, -1.323143620866313208, 11.49999999999999645 ) ) ;
#4364 = VERTEX_POINT ( 'NONE', #28952 ) ;
#4365 = CARTESIAN_POINT ( 'NONE',  ( -1.036876607668611117, -5.876774720514417183, 20.14881673916291405 ) ) ;
#4366 = DIRECTION ( 'NONE',  ( 0.000000000000000000, -0.000000000000000000, 1.000000000000000000 ) ) ;
#4367 = CARTESIAN_POINT ( 'NONE',  ( -26.47413879005073056, -24.93063536979281380, 7.801149312106798739 ) ) ;
#4368 = CARTESIAN_POINT ( 'NONE',  ( -2.702089344534958304, -6.376774720514413630, 19.72789237585158162 ) ) ;
#4369 = ORIENTED_EDGE ( 'NONE', *, *, #65661, .F. ) ;
#4370 = CIRCLE ( 'NONE', #49800, 251.9358649670780892 ) ;
#4371 = ORIENTED_EDGE ( 'NONE', *, *, #32218, .T. ) ;
#4372 = EDGE_CURVE ( 'NONE', #43974, #61226, #74714, .T. ) ;
#4373 = CARTESIAN_POINT ( 'NONE',  ( -30.57287095715006231, -23.48210175247266562, -1.443836490256470428 ) ) ;
#4374 = CARTESIAN_POINT ( 'NONE',  ( -22.32109313027335062, -5.015931025267754251, 11.49999999999998934 ) ) ;
#4375 = CARTESIAN_POINT ( 'NONE',  ( -74.62287095715002749, -23.73907113216991860, -1.053371485793227480 ) ) ;
#4376 = CARTESIAN_POINT ( 'NONE',  ( -8.857468890034409625, -19.66367526556523870, -1.500000000000002220 ) ) ;
#4377 = FACE_OUTER_BOUND ( 'NONE', #481, .T. ) ;
#4378 = DIRECTION ( 'NONE',  ( -3.773278334453080206E-23, 0.9999999999976377785, 2.173523156925979975E-06 ) ) ;
#4379 = CARTESIAN_POINT ( 'NONE',  ( -19.74168752133572724, 10.86179948771369297, 11.49999999999999645 ) ) ;
#4380 = EDGE_LOOP ( 'NONE', ( #22061, #91754, #10612, #10485 ) ) ;
#4381 = CARTESIAN_POINT ( 'NONE',  ( 0.000000000000000000, 0.000000000000000000, 4.450000000000000178 ) ) ;
#4382 = CARTESIAN_POINT ( 'NONE',  ( 19.49364837986538745, 10.19379059548657551, 11.49999999999998934 ) ) ;
#4383 = AXIS2_PLACEMENT_3D ( 'NONE', #79861, #33700, #10355 ) ;
#4384 = LINE ( 'NONE', #58661, #21940 ) ;
#4385 = FACE_OUTER_BOUND ( 'NONE', #83513, .T. ) ;
#4386 = VERTEX_POINT ( 'NONE', #67041 ) ;
#4387 = FACE_OUTER_BOUND ( 'NONE', #33731, .T. ) ;
#4388 = CARTESIAN_POINT ( 'NONE',  ( -97.62287095715005592, -29.50250243563736774, 8.947779886222138046 ) ) ;
#4389 = ORIENTED_EDGE ( 'NONE', *, *, #95271, .T. ) ;
#4390 = VECTOR ( 'NONE', #95261, 1000.000000000000114 ) ;
#4391 = FACE_OUTER_BOUND ( 'NONE', #11163, .T. ) ;
#4392 = ORIENTED_EDGE ( 'NONE', *, *, #25073, .F. ) ;
#4393 = ORIENTED_EDGE ( 'NONE', *, *, #60214, .F. ) ;
#4394 = ORIENTED_EDGE ( 'NONE', *, *, #95900, .F. ) ;
#4395 = CARTESIAN_POINT ( 'NONE',  ( -80.51244414166535535, -25.03284467579916495, 7.563174216508125269 ) ) ;
#4396 = CARTESIAN_POINT ( 'NONE',  ( -89.40841769935767047, -29.50249917535260380, 7.447779886225679213 ) ) ;
#4397 = DIRECTION ( 'NONE',  ( 0.000000000000000000, -1.000000000000000000, 0.000000000000000000 ) ) ;
#4398 = CARTESIAN_POINT ( 'NONE',  ( 16.53694760393551988, -11.94906295602464397, -1.500000000000002220 ) ) ;
#4399 = EDGE_LOOP ( 'NONE', ( #22097, #14597, #15336, #18356 ) ) ;
#4400 = CARTESIAN_POINT ( 'NONE',  ( -71.43540103747046999, -25.13480990690564454, 7.034471417043156372 ) ) ;
#4401 = CARTESIAN_POINT ( 'NONE',  ( -29.56144366762476849, -23.65480093107256820, 11.05961561336856391 ) ) ;
#4402 = CARTESIAN_POINT ( 'NONE',  ( -97.52287095715006160, -24.64898659630367916, 1.056161002820829697 ) ) ;
#4403 = CARTESIAN_POINT ( 'NONE',  ( -70.34543693012690824, -25.03149849800392346, 7.563174219434074530 ) ) ;
#4404 = ORIENTED_EDGE ( 'NONE', *, *, #90288, .F. ) ;
#4405 = CARTESIAN_POINT ( 'NONE',  ( -28.88251580808842789, -24.76881010668045136, 2.994894255481803658 ) ) ;
#4406 = CARTESIAN_POINT ( 'NONE',  ( -87.92287095715005307, -23.47593901973090169, -1.443836447538996870 ) ) ;
#4407 = ORIENTED_EDGE ( 'NONE', *, *, #91288, .T. ) ;
#4408 = CARTESIAN_POINT ( 'NONE',  ( 5.906898857431191807, -19.90033995357616092, 11.49999999999998934 ) ) ;
#4409 = VERTEX_POINT ( 'NONE', #52300 ) ;
#4411 = ORIENTED_EDGE ( 'NONE', *, *, #21402, .T. ) ;
#4410 = DIRECTION ( 'NONE',  ( -0.000000000000000000, 1.000000000000000000, -0.000000000000000000 ) ) ;
#4412 = ADVANCED_FACE ( 'NONE', ( #21324 ), #88872, .F. ) ;
#4413 = B_SPLINE_CURVE_WITH_KNOTS ( 'NONE', 3,
 ( #79439, #93153, #1332, #63237 ),
 .UNSPECIFIED., .F., .F.,
 ( 4, 4 ),
 ( 0.000000000000000000, 9.999999999997510880E-05 ),
 .UNSPECIFIED. ) ;
#4414 = CARTESIAN_POINT ( 'NONE',  ( -90.52380231474226946, -25.23397913219354649, 6.409327625488845825 ) ) ;
#4415 = CARTESIAN_POINT ( 'NONE',  ( 5.085443162053245203, -3.316774720514426456, -27.56355752155217331 ) ) ;
#4416 = VERTEX_POINT ( 'NONE', #59408 ) ;
#4417 = ORIENTED_EDGE ( 'NONE', *, *, #94440, .F. ) ;
#4418 = CARTESIAN_POINT ( 'NONE',  ( -11.64875734969026233, 0.3587747205144265483, 31.02402280011862246 ) ) ;
#4419 = B_SPLINE_CURVE_WITH_KNOTS ( 'NONE', 3,
 ( #54350, #78155, #94400, #17277, #23366, #54851 ),
 .UNSPECIFIED., .F., .F.,
 ( 4, 2, 4 ),
 ( 0.000000000000000000, 0.001380764517854768218, 0.002761529035709536437 ),
 .UNSPECIFIED. ) ;
#4420 = CARTESIAN_POINT ( 'NONE',  ( -98.62287095715005592, -23.48786465467241769, 11.44779295918254292 ) ) ;
#4421 = CARTESIAN_POINT ( 'NONE',  ( 22.02124265030973760, -5.356774720514425603, 16.20402280011862217 ) ) ;
#4422 = CARTESIAN_POINT ( 'NONE',  ( -70.65140973383547873, -25.31201598237044337, 5.348842032383912759 ) ) ;
#4424 = VERTEX_POINT ( 'NONE', #66557 ) ;
#4423 = CARTESIAN_POINT ( 'NONE',  ( 14.84500176111689207, -16.38379996218902335, 11.49999999999999645 ) ) ;
#4425 = CARTESIAN_POINT ( 'NONE',  ( -108.5571772755274651, -23.73766607897671221, -1.055555164236429144 ) ) ;
#4426 = CARTESIAN_POINT ( 'NONE',  ( -20.05226876979747530, -10.47825485868949613, -1.500000000000002220 ) ) ;
#4427 = EDGE_CURVE ( 'NONE', #52058, #61887, #51736, .T. ) ;
#4428 = AXIS2_PLACEMENT_3D ( 'NONE', #41235, #48856, #72190 ) ;
#4429 = EDGE_CURVE ( 'NONE', #76857, #4511, #36559, .T. ) ;
#4430 = EDGE_CURVE ( 'NONE', #66916, #64607, #3218, .T. ) ;
#4432 = ORIENTED_EDGE ( 'NONE', *, *, #70652, .T. ) ;
#4431 = CARTESIAN_POINT ( 'NONE',  ( -115.5895802679274595, -24.52399227489127043, 9.353111116836528183 ) ) ;
#4433 = ORIENTED_EDGE ( 'NONE', *, *, #64498, .T. ) ;
#4434 = EDGE_CURVE ( 'NONE', #14844, #26747, #35909, .T. ) ;
#4435 = AXIS2_PLACEMENT_3D ( 'NONE', #8922, #22630, #55111 ) ;
#4436 = CARTESIAN_POINT ( 'NONE',  ( -10.11875734969026119, -3.519249775642004696, 30.51402280011862445 ) ) ;
#4437 = CARTESIAN_POINT ( 'NONE',  ( -78.62287095715005592, -24.33927499327853994, 9.819080762295810061 ) ) ;
#4438 = ORIENTED_EDGE ( 'NONE', *, *, #20775, .T. ) ;
#4439 = CARTESIAN_POINT ( 'NONE',  ( -15.68702345270385834, -14.21367052863537417, 11.49999999999998934 ) ) ;
#4440 = CARTESIAN_POINT ( 'NONE',  ( 5.359050311451609261, -5.876774720514419847, 21.05346524168807676 ) ) ;
#4441 = CARTESIAN_POINT ( 'NONE',  ( -80.62287095715002749, -23.85229601348994777, 10.88205029486208986 ) ) ;
#4442 = CARTESIAN_POINT ( 'NONE',  ( -9.338385371603758145, -20.21602636099808237, -1.500000000000002220 ) ) ;
#4443 = CARTESIAN_POINT ( 'NONE',  ( -46.62287095715004170, -23.72747288104441665, -1.053458166803663110 ) ) ;
#4444 = EDGE_CURVE ( 'NONE', #90864, #27723, #95212, .T. ) ;
#4445 = ORIENTED_EDGE ( 'NONE', *, *, #51520, .T. ) ;
#4446 = CARTESIAN_POINT ( 'NONE',  ( -66.22287095715007865, -23.47593901973090524, -1.443836447538997980 ) ) ;
#4447 = CARTESIAN_POINT ( 'NONE',  ( -104.5895376238167245, -23.47593901973091235, -1.443836447539001089 ) ) ;
#4448 = VECTOR ( 'NONE', #99985, 1000.000000000000000 ) ;
#4449 = CARTESIAN_POINT ( 'NONE',  ( -103.5228709571500616, -24.50321055353803956, 9.387540953477515160 ) ) ;
#4450 = CARTESIAN_POINT ( 'NONE',  ( -44.62287095715004881, -23.47596703998600631, 11.44779298504227505 ) ) ;
#4451 = EDGE_CURVE ( 'NONE', #51313, #86, #13719, .T. ) ;
#4452 = CARTESIAN_POINT ( 'NONE',  ( 9.662506626059768067, -16.94115208737379774, -1.500000000000002220 ) ) ;
#4453 = CARTESIAN_POINT ( 'NONE',  ( -9.048234560742015375, 19.43086790383670603, -1.500000000000002220 ) ) ;
#4454 = CARTESIAN_POINT ( 'NONE',  ( -1.122631020312409245, -5.876774720514411854, 19.41635569784906679 ) ) ;
#4455 = FACE_OUTER_BOUND ( 'NONE', #80543, .T. ) ;
#4456 = DIRECTION ( 'NONE',  ( -3.773278334453079618E-23, 0.9999999999976377785, 2.173523156925979975E-06 ) ) ;
#4457 = CARTESIAN_POINT ( 'NONE',  ( -22.55118551311790753, 3.560990644294375063, -1.500000000000002220 ) ) ;
#4458 = EDGE_CURVE ( 'NONE', #34695, #70182, #27471, .T. ) ;
#4459 = VECTOR ( 'NONE', #50190, 1000.000000000000114 ) ;
#4460 = PERSON_AND_ORGANIZATION ( #70597, #27821 ) ;
#4461 = CARTESIAN_POINT ( 'NONE',  ( -106.5222054324230356, -23.48786465467241769, 11.44779295918253403 ) ) ;
#4462 = DIRECTION ( 'NONE',  ( 7.904402583950632871E-14, 0.000000000000000000, -1.000000000000000000 ) ) ;
#4463 = CARTESIAN_POINT ( 'NONE',  ( -3.169371320753151977, 19.67850563098683736, 11.49999999999999645 ) ) ;
#4464 = CARTESIAN_POINT ( 'NONE',  ( -104.5495398974881169, -24.51314013834316086, 0.6176544820404171743 ) ) ;
#4465 = AXIS2_PLACEMENT_3D ( 'NONE', #52978, #5794, #20508 ) ;
#4466 = CARTESIAN_POINT ( 'NONE',  ( -39.62886954152041596, -24.51419770103158413, 9.386484678747189392 ) ) ;
#4467 = CARTESIAN_POINT ( 'NONE',  ( -48.64594432017239711, -23.96119346886880663, -0.6495511937831938143 ) ) ;
#4468 = ORIENTED_EDGE ( 'NONE', *, *, #27568, .T. ) ;
#4469 = CARTESIAN_POINT ( 'NONE',  ( -45.62287095715004881, -29.50247984919015209, -1.443849546365058689 ) ) ;
#4470 = CARTESIAN_POINT ( 'NONE',  ( -31.21619930677465504, -25.31600595412499644, 6.101236642668423471 ) ) ;
#4471 = ADVANCED_FACE ( 'NONE', ( #73638 ), #75124, .F. ) ;
#4472 = CARTESIAN_POINT ( 'NONE',  ( -10.76533847658563126, -18.86179312034942868, 11.49999999999998934 ) ) ;
#4473 = CARTESIAN_POINT ( 'NONE',  ( -5.023036858974361252, -6.376774720514410077, 19.14743589743590846 ) ) ;
#4474 = CARTESIAN_POINT ( 'NONE',  ( -0.4769873229303308038, -19.55164744950295841, -1.500000000000002220 ) ) ;
#4475 = CARTESIAN_POINT ( 'NONE',  ( -55.55110250455299337, -24.15602025860896518, 10.28564288303535257 ) ) ;
#4476 = EDGE_CURVE ( 'NONE', #86005, #84008, #62621, .T. ) ;
#4477 = ORIENTED_EDGE ( 'NONE', *, *, #33366, .T. ) ;
#4478 = APPROVAL_STATUS ( 'not_yet_approved' ) ;
#4479 = CARTESIAN_POINT ( 'NONE',  ( -89.62287095715004170, -23.47596703998600631, 11.44779298504227860 ) ) ;
#4480 = CARTESIAN_POINT ( 'NONE',  ( -16.87313589883980214, -11.49665204554024989, 11.49999999999999645 ) ) ;
#4481 = CARTESIAN_POINT ( 'NONE',  ( -53.01255352321339842, -2.682774720514426559, 35.59556822165056644 ) ) ;
#4482 = CARTESIAN_POINT ( 'NONE',  ( 10.54059822343757880, -5.876774720514426953, 22.82308057603841078 ) ) ;
#4483 = ORIENTED_EDGE ( 'NONE', *, *, #8647, .T. ) ;
#4484 = CARTESIAN_POINT ( 'NONE',  ( -53.52287095715006870, -23.47596703998600631, 11.44779298504229104 ) ) ;
#4485 = DIRECTION ( 'NONE',  ( 0.9822594791677485837, 0.000000000000000000, -0.1875268396392987258 ) ) ;
#4486 = DIRECTION ( 'NONE',  ( -0.000000000000000000, 0.000000000000000000, -1.000000000000000000 ) ) ;
#4487 = APPLICATION_CONTEXT ( 'configuration controlled 3d designs of mechanical parts and assemblies' ) ;
#4488 = CARTESIAN_POINT ( 'NONE',  ( -67.52287095715006160, -23.47596703998600631, 11.44779298504228748 ) ) ;
#4489 = ORIENTED_EDGE ( 'NONE', *, *, #26293, .F. ) ;
#4490 = CARTESIAN_POINT ( 'NONE',  ( 5.771117285127500551, -6.376774720514417183, 20.39900056875960388 ) ) ;
#4491 = VECTOR ( 'NONE', #13376, 1000.000000000000114 ) ;
#4492 = CARTESIAN_POINT ( 'NONE',  ( 22.26416322464526232, -5.798680748638591176, 11.49999999999999645 ) ) ;
#4493 = CARTESIAN_POINT ( 'NONE',  ( -22.77908990650604792, -0.06651829912971220227, -1.500000000000002220 ) ) ;
#4494 = CARTESIAN_POINT ( 'NONE',  ( -110.5103923454349939, -25.00182538069147142, 7.747789668545045139 ) ) ;
#4496 = B_SPLINE_SURFACE_WITH_KNOTS ( 'NONE', 3, 3, ( 
 ( #37821, #61675, #23070, #14469 ),
 ( #69269, #76856, #100185, #13975 ),
 ( #76365, #37334, #46430, #7863 ),
 ( #68278, #45451, #54060, #77361 ),
 ( #30704, #91105, #38809, #99208 ),
 ( #83487, #70268, #14972, #61179 ),
 ( #93092, #15965, #21580, #53563 ) ),
 .UNSPECIFIED., .F., .F., .F.,
 ( 4, 3, 4 ),
 ( 4, 4 ),
 ( 0.7945040050992246972, 0.8970133687736505657, 0.9995227324480763231 ),
 ( 0.5796412921291099751, 0.5809216175690411488 ),
 .UNSPECIFIED. ) ;
#4495 = B_SPLINE_CURVE_WITH_KNOTS ( 'NONE', 3,
 ( #76729, #53431, #36698, #53929, #21946, #52931 ),
 .UNSPECIFIED., .F., .F.,
 ( 4, 2, 4 ),
 ( 0.000000000000000000, 0.001380901958385385509, 0.002761803916770771018 ),
 .UNSPECIFIED. ) ;
#4497 = CARTESIAN_POINT ( 'NONE',  ( -36.62287095715005592, -29.50250786944525672, 11.44777988621624232 ) ) ;
#4498 = DIRECTION ( 'NONE',  ( 0.000000000000000000, -1.000000000000000000, 0.000000000000000000 ) ) ;
#4499 = CARTESIAN_POINT ( 'NONE',  ( -70.52287095715007581, -24.15431212366388891, -0.2830839119429260364 ) ) ;
#4500 = CARTESIAN_POINT ( 'NONE',  ( -110.5975878789654274, -23.48783264082476663, -1.443836473390091690 ) ) ;
#4501 = CARTESIAN_POINT ( 'NONE',  ( -21.08706934527708654, 5.832127334627817739, 11.49999999999998934 ) ) ;
#4502 = CARTESIAN_POINT ( 'NONE',  ( 4.784292611718075072, 3.316774720514426456, -25.54547254883186014 ) ) ;
#4503 = CARTESIAN_POINT ( 'NONE',  ( -0.02075734969026423599, -6.475225279485573360, -0.08597719988137648983 ) ) ;
#4504 = CARTESIAN_POINT ( 'NONE',  ( -120.6228709571500701, -24.82558206586149652, 1.605769216559631341 ) ) ;
#4505 = CARTESIAN_POINT ( 'NONE',  ( -58.53812816766490101, -24.51314013834315020, 0.6176544820404091807 ) ) ;
#4506 = ORIENTED_EDGE ( 'NONE', *, *, #100335, .F. ) ;
#4507 = CARTESIAN_POINT ( 'NONE',  ( 3.609400094169940676, -20.08663944828865766, -1.500000000000002220 ) ) ;
#4508 = ORIENTED_EDGE ( 'NONE', *, *, #71674, .T. ) ;
#4509 = ORIENTED_EDGE ( 'NONE', *, *, #62263, .F. ) ;
#4510 = ORIENTED_EDGE ( 'NONE', *, *, #33159, .T. ) ;
#4511 = VERTEX_POINT ( 'NONE', #19342 ) ;
#4512 = CARTESIAN_POINT ( 'NONE',  ( 22.92345266703080142, -2.467471440992916154, -1.500000000000002220 ) ) ;
#4513 = CARTESIAN_POINT ( 'NONE',  ( -80.52287095715006160, -25.00158670708909625, 2.256160236439166411 ) ) ;
#4514 = CARTESIAN_POINT ( 'NONE',  ( 11.17094659993960803, -16.83544227557131023, -1.500000000000002220 ) ) ;
#4515 = ORIENTED_EDGE ( 'NONE', *, *, #29755, .T. ) ;
#4516 = CARTESIAN_POINT ( 'NONE',  ( -98.62287095715005592, -24.64965695001469115, 8.947790433994178727 ) ) ;
#4517 = AXIS2_PLACEMENT_3D ( 'NONE', #38624, #54365, #23896 ) ;
#4518 = CARTESIAN_POINT ( 'NONE',  ( -34.52287095715006160, -24.64965694238575011, 8.947790433994207149 ) ) ;
#4519 = LINE ( 'NONE', #35467, #65932 ) ;
#4520 = CARTESIAN_POINT ( 'NONE',  ( -53.50784545873391096, -23.96169478059712787, 10.65365249895718591 ) ) ;
#4522 = ORIENTED_EDGE ( 'NONE', *, *, #6230, .T. ) ;
#4521 = CARTESIAN_POINT ( 'NONE',  ( 2.027878592902508270, 21.29203748114955985, 11.49999999999999645 ) ) ;
#4523 = CARTESIAN_POINT ( 'NONE',  ( 6.026614999332422182E-17, -23.47593901973084485, -1.443836476861628304 ) ) ;
#4524 = ORIENTED_EDGE ( 'NONE', *, *, #89345, .F. ) ;
#4525 = CARTESIAN_POINT ( 'NONE',  ( 2.321567282091853812, -22.14299765706108403, -1.500000000000002220 ) ) ;
#4526 = CARTESIAN_POINT ( 'NONE',  ( -13.01863806243235899, 16.06808769575019014, -1.500000000000002220 ) ) ;
#4527 = AXIS2_PLACEMENT_3D ( 'NONE', #90989, #13859, #52439 ) ;
#4528 = VERTEX_POINT ( 'NONE', #96468 ) ;
#4529 = CARTESIAN_POINT ( 'NONE',  ( -55.62287095715005592, -29.50250786944525672, 11.44777988621623876 ) ) ;
#4530 = ORIENTED_EDGE ( 'NONE', *, *, #10138, .T. ) ;
#4531 = EDGE_CURVE ( 'NONE', #98739, #60599, #51298, .T. ) ;
#4532 = CARTESIAN_POINT ( 'NONE',  ( -81.52287095715009002, -23.73907113217678955, -1.053371485781112282 ) ) ;
#4533 = CIRCLE ( 'NONE', #40158, 1.700000000000000178 ) ;
#4534 = ORIENTED_EDGE ( 'NONE', *, *, #96856, .T. ) ;
#4536 = EDGE_CURVE ( 'NONE', #75736, #27742, #82735, .T. ) ;
#4535 = CARTESIAN_POINT ( 'NONE',  ( 6.620851319379956301, 6.475225279485576024, -27.30756699305372592 ) ) ;
#4537 = CARTESIAN_POINT ( 'NONE',  ( 15.12549221760053086, 14.48511125727034177, -1.500000000000002220 ) ) ;
#4538 = CARTESIAN_POINT ( 'NONE',  ( -16.24880213243413607, 14.73142910551002238, 11.49999999999999645 ) ) ;
#4539 = EDGE_CURVE ( 'NONE', #99974, #4160, #26958, .T. ) ;
#4540 = FACE_OUTER_BOUND ( 'NONE', #97206, .T. ) ;
#4541 = CARTESIAN_POINT ( 'NONE',  ( -15.68175098440391402, -16.16561365185589594, -1.500000000000002220 ) ) ;
#4542 = EDGE_CURVE ( 'NONE', #74051, #97749, #42703, .T. ) ;
#4543 = CARTESIAN_POINT ( 'NONE',  ( 0.8316226063609513108, 20.92010288561657205, 11.49999999999998934 ) ) ;
#4544 = CARTESIAN_POINT ( 'NONE',  ( -89.40841769935767047, -25.11033443737731474, 2.832404817301930056 ) ) ;
#4545 = CARTESIAN_POINT ( 'NONE',  ( 5.654871928786437074, -6.376774720514420736, 20.64717925217163952 ) ) ;
#4546 = EDGE_CURVE ( 'NONE', #32133, #11978, #72217, .T. ) ;
#4547 = CARTESIAN_POINT ( 'NONE',  ( -119.5556264641217723, -23.96169478059714564, 10.65365249895717170 ) ) ;
#4548 = CARTESIAN_POINT ( 'NONE',  ( 1.175186991919848989, 5.965225279485572685, 28.89597625626659649 ) ) ;
#4549 = ORIENTED_EDGE ( 'NONE', *, *, #32492, .F. ) ;
#4550 = ORIENTED_EDGE ( 'NONE', *, *, #12541, .F. ) ;
#4551 = VERTEX_POINT ( 'NONE', #7113 ) ;
#4552 = FACE_OUTER_BOUND ( 'NONE', #85461, .T. ) ;
#4553 = ORIENTED_EDGE ( 'NONE', *, *, #55894, .T. ) ;
#4554 = CARTESIAN_POINT ( 'NONE',  ( 9.988417798295188277, 18.97302403871600518, -1.500000000000002220 ) ) ;
#4555 = CARTESIAN_POINT ( 'NONE',  ( 0.1309051665272248643, -6.376774720514413630, 19.34190049657482291 ) ) ;
#4556 = ORIENTED_EDGE ( 'NONE', *, *, #97384, .F. ) ;
#4557 = CARTESIAN_POINT ( 'NONE',  ( -16.00611555608923098, 13.71732778110762219, 11.49999999999998934 ) ) ;
#4558 = CARTESIAN_POINT ( 'NONE',  ( -100.2210274182397711, -25.19675915012271616, 3.305962695313816813 ) ) ;
#4559 = CARTESIAN_POINT ( 'NONE',  ( 2.591664760199015927, -6.376774720514417183, 20.15921530338947321 ) ) ;
#4560 = CARTESIAN_POINT ( 'NONE',  ( -87.62287095715009855, -24.34917612406837506, 0.1852690917426670081 ) ) ;
#4561 = CARTESIAN_POINT ( 'NONE',  ( -8.676776695296464226, 18.57322330470350735, 0.000000000000000000 ) ) ;
#4562 = CARTESIAN_POINT ( 'NONE',  ( -100.5228709571500616, -24.99132157543084531, 2.256160258750667502 ) ) ;
#4563 = CARTESIAN_POINT ( 'NONE',  ( 6.025212951983072607, -21.27585971943098642, -1.500000000000002220 ) ) ;
#4564 = CARTESIAN_POINT ( 'NONE',  ( -110.2929128916653525, -25.14264220134206695, 6.986250900936242125 ) ) ;
#4565 = CARTESIAN_POINT ( 'NONE',  ( -3.108425644221024520, -6.376774720514415407, 20.25188360057253334 ) ) ;
#4566 = CARTESIAN_POINT ( 'NONE',  ( -63.55620429048337883, -23.47593901973091235, -1.443836447539007972 ) ) ;
#4567 = B_SPLINE_CURVE_WITH_KNOTS ( 'NONE', 3,
 ( #37542, #99428, #68001, #97443 ),
 .UNSPECIFIED., .F., .F.,
 ( 4, 4 ),
 ( 0.000000000000000000, 1.000000000000000000 ),
 .UNSPECIFIED. ) ;
#4568 = CARTESIAN_POINT ( 'NONE',  ( -62.63696707577763334, -24.15620529776627379, 10.23563542870660825 ) ) ;
#4569 = ADVANCED_FACE ( 'NONE', ( #37065 ), #22322, .F. ) ;
#4570 = VERTEX_POINT ( 'NONE', #29444 ) ;
#4571 = CARTESIAN_POINT ( 'NONE',  ( 32.42932432802503939, 6.376774720514426953, -0.2107846672978405389 ) ) ;
#4572 = CARTESIAN_POINT ( 'NONE',  ( 7.684279652734260502, -19.92951104315265809, -1.500000000000002220 ) ) ;
#4573 = CARTESIAN_POINT ( 'NONE',  ( -76.52287095715007581, -29.50248528299804818, 1.056150453629038477 ) ) ;
#4574 = CARTESIAN_POINT ( 'NONE',  ( -49.88696936683380301, -25.25978491487771649, 3.590542621692356384 ) ) ;
#4575 = CARTESIAN_POINT ( 'NONE',  ( -64.54879172121601982, -24.15620529776628445, 10.23563542870660115 ) ) ;
#4576 = CARTESIAN_POINT ( 'NONE',  ( -68.55620429048339304, -23.48783264082478084, -1.443836473390067265 ) ) ;
#4577 = CARTESIAN_POINT ( 'NONE',  ( 18.79633983808273712, -12.56333175589740847, -1.500000000000002220 ) ) ;
#4578 = B_SPLINE_SURFACE_WITH_KNOTS ( 'NONE', 3, 3, ( 
 ( #38424, #31309, #62278, #23688 ),
 ( #54662, #16080, #47050, #70378 ),
 ( #87608, #70889, #72390, #87098 ),
 ( #39926, #47552, #78473, #71388 ),
 ( #1380, #8973, #31820, #80484 ),
 ( #48048, #62789, #49056, #93704 ),
 ( #2375, #86598, #78978, #57177 ) ),
 .UNSPECIFIED., .F., .F., .F.,
 ( 4, 3, 4 ),
 ( 4, 4 ),
 ( 0.0004766839783820824798, 0.1029713700210898031, 0.2054660560637975308 ),
 ( 0.3395803806953949788, 0.3407497870151264818 ),
 .UNSPECIFIED. ) ;
#4579 = DIRECTION ( 'NONE',  ( 0.000000000000000000, 0.9999999999976377785, 2.173523156925979975E-06 ) ) ;
#4580 = ORIENTED_EDGE ( 'NONE', *, *, #91840, .F. ) ;
#4581 = CARTESIAN_POINT ( 'NONE',  ( 4.653726706778644306, -5.876774720514415407, 20.04674869880385302 ) ) ;
#4582 = DIRECTION ( 'NONE',  ( -3.773278334453079618E-23, 0.9999999999976377785, 2.173523156925979975E-06 ) ) ;
#4583 = CARTESIAN_POINT ( 'NONE',  ( 16.04393857186779115, -11.51807295290239885, 11.49999999999999645 ) ) ;
#4584 = CARTESIAN_POINT ( 'NONE',  ( 0.7395552074414002419, -5.331939213628640317, 9.000000000000000000 ) ) ;
#4585 = CARTESIAN_POINT ( 'NONE',  ( -67.59731535907285149, -23.96119346886880308, -0.6495511937832114668 ) ) ;
#4586 = VERTEX_POINT ( 'NONE', #75609 ) ;
#4587 = DIRECTION ( 'NONE',  ( -0.9890158633619158257, -0.1478094111296165691, -0.000000000000000000 ) ) ;
#4588 = CARTESIAN_POINT ( 'NONE',  ( -29.74701180552300883, -24.60094371313986983, 3.841292727239494109 ) ) ;
#4589 = CARTESIAN_POINT ( 'NONE',  ( -101.1692196971220312, -25.17353295164373250, 6.877671026811838395 ) ) ;
#4590 = CARTESIAN_POINT ( 'NONE',  ( 14.26105141482337935, -16.23293960606763520, -1.500000000000002220 ) ) ;
#4591 = CARTESIAN_POINT ( 'NONE',  ( -49.10457154551148307, -25.27518131127733270, 3.999772247467727304 ) ) ;
#4592 = VECTOR ( 'NONE', #19048, 1000.000000000000227 ) ;
#4593 = CARTESIAN_POINT ( 'NONE',  ( 11.20917403917954225, 15.81763734437701885, -1.500000000000002220 ) ) ;
#4594 = DIRECTION ( 'NONE',  ( 0.000000000000000000, 0.000000000000000000, 1.000000000000000000 ) ) ;
#4595 = CARTESIAN_POINT ( 'NONE',  ( -97.55620429048340725, -23.47596703998600631, 11.44779298504227683 ) ) ;
#4596 = ADVANCED_FACE ( 'NONE', ( #45190 ), #44924, .T. ) ;
#4597 = CARTESIAN_POINT ( 'NONE',  ( 16.35176858736616978, 11.14859404531058473, 11.49999999999998934 ) ) ;
#4598 = ORIENTED_EDGE ( 'NONE', *, *, #8683, .F. ) ;
#4599 = CARTESIAN_POINT ( 'NONE',  ( 19.34776771173714849, 6.126202725962671458, 11.49999999999999645 ) ) ;
#4600 = CARTESIAN_POINT ( 'NONE',  ( 13.02836919244612623, 3.777199458296179646, -28.16488413836729521 ) ) ;
#4601 = EDGE_CURVE ( 'NONE', #74060, #14845, #30224, .T. ) ;
#4602 = AXIS2_PLACEMENT_3D ( 'NONE', #24858, #32478, #9135 ) ;
#4603 = CARTESIAN_POINT ( 'NONE',  ( 5.766314450391940127, -5.876774720514423400, 21.17177008079512035 ) ) ;
#4604 = ORIENTED_EDGE ( 'NONE', *, *, #83320, .T. ) ;
#4605 = DIRECTION ( 'NONE',  ( -1.000000000000000000, -3.773278334444167608E-23, -8.201307833595939069E-29 ) ) ;
#4606 = CARTESIAN_POINT ( 'NONE',  ( -108.8968792378191921, -25.06732983082694943, 7.447789526168955732 ) ) ;
#4607 = CARTESIAN_POINT ( 'NONE',  ( -123.5228709571500616, -29.50247984919015209, -1.443849546365046699 ) ) ;
#4608 = VECTOR ( 'NONE', #89946, 1000.000000000000000 ) ;
#4609 = CARTESIAN_POINT ( 'NONE',  ( -95.62287095715002749, -23.85196035786901092, -0.8779234886474903687 ) ) ;
#4610 = B_SPLINE_CURVE_WITH_KNOTS ( 'NONE', 3,
 ( #31848, #87636, #62816, #10500 ),
 .UNSPECIFIED., .F., .F.,
 ( 4, 4 ),
 ( 0.8203717318505863165, 0.8293781631227020723 ),
 .UNSPECIFIED. ) ;
#4611 = LINE ( 'NONE', #89833, #86767 ) ;
#4612 = CARTESIAN_POINT ( 'NONE',  ( 7.608091486120485136, 18.53616061196756704, -1.500000000000002220 ) ) ;
#4613 = DIRECTION ( 'NONE',  ( -0.9978940991575084851, -0.000000000000000000, -0.06486421869277853025 ) ) ;
#4614 = ORIENTED_EDGE ( 'NONE', *, *, #57654, .F. ) ;
#4615 = CARTESIAN_POINT ( 'NONE',  ( -32.62287095715004170, -23.73934037231755667, 11.05740245334329508 ) ) ;
#4616 = DIRECTION ( 'NONE',  ( -0.000000000000000000, -1.000000000000000000, -0.000000000000000000 ) ) ;
#4617 = CARTESIAN_POINT ( 'NONE',  ( -76.62287095715007013, -29.50247984919015209, -1.443849546365053582 ) ) ;
#4618 = CARTESIAN_POINT ( 'NONE',  ( 27.86270917940689174, -5.965225279485572685, 29.49402280011862487 ) ) ;
#4619 = DIRECTION ( 'NONE',  ( 0.7512896232465891000, 0.000000000000000000, 0.6599726524652351767 ) ) ;
#4620 = CARTESIAN_POINT ( 'NONE',  ( -50.78612140924919771, -25.12100811749006724, 7.112893600995336740 ) ) ;
#4621 = ORIENTED_EDGE ( 'NONE', *, *, #5912, .T. ) ;
#4622 = CARTESIAN_POINT ( 'NONE',  ( -20.07547297788957152, 3.163885811906596679, -1.500000000000002220 ) ) ;
#4623 = EDGE_LOOP ( 'NONE', ( #59326, #40610, #84625, #66666 ) ) ;
#4624 = CARTESIAN_POINT ( 'NONE',  ( 2.319610639010541764, -22.79860127089448696, -1.500000000000002220 ) ) ;
#4625 = CARTESIAN_POINT ( 'NONE',  ( 29.77147767949870882, 6.376774720514427841, 26.15915692125050995 ) ) ;
#4626 = VERTEX_POINT ( 'NONE', #85235 ) ;
#4627 = CARTESIAN_POINT ( 'NONE',  ( -49.74369414166532266, -25.30543060587212167, 4.940877950953177944 ) ) ;
#4628 = CARTESIAN_POINT ( 'NONE',  ( -50.16062266432883376, -25.26264174977159271, 7.085347539999360400 ) ) ;
#4629 = CARTESIAN_POINT ( 'NONE',  ( -117.5228709571500758, -23.48786465467241769, 11.44779295918253759 ) ) ;
#4630 = CARTESIAN_POINT ( 'NONE',  ( -6.347832186973104029, -20.24257907634199682, 11.49999999999999645 ) ) ;
#4631 = ORIENTED_EDGE ( 'NONE', *, *, #29196, .T. ) ;
#4632 = CARTESIAN_POINT ( 'NONE',  ( -21.91529987491217923, -3.391794311424265018, 11.49999999999998934 ) ) ;
#4633 = B_SPLINE_CURVE_WITH_KNOTS ( 'NONE', 3,
 ( #42536, #42036, #73968, #43524 ),
 .UNSPECIFIED., .F., .F.,
 ( 4, 4 ),
 ( 0.000000000000000000, 9.999999999993348899E-05 ),
 .UNSPECIFIED. ) ;
#4634 = CARTESIAN_POINT ( 'NONE',  ( 10.47388184937329214, 17.72644800832989986, -1.500000000000002220 ) ) ;
#4635 = ORIENTED_EDGE ( 'NONE', *, *, #28569, .F. ) ;
#4636 = ORIENTED_EDGE ( 'NONE', *, *, #56225, .F. ) ;
#4637 = CARTESIAN_POINT ( 'NONE',  ( 6.944081373883786767, -6.376774720514424288, 21.27829155525578031 ) ) ;
#4638 = CARTESIAN_POINT ( 'NONE',  ( -50.52287095715006160, -24.99156044556120193, 7.747789690856173195 ) ) ;
#4639 = ORIENTED_EDGE ( 'NONE', *, *, #25265, .T. ) ;
#4641 = ORIENTED_EDGE ( 'NONE', *, *, #88047, .F. ) ;
#4640 = EDGE_CURVE ( 'NONE', #30940, #24715, #37163, .T. ) ;
#4642 = EDGE_LOOP ( 'NONE', ( #58103, #79505, #82496, #6564, #64310, #12909, #4407, #15201 ) ) ;
#4643 = CARTESIAN_POINT ( 'NONE',  ( -20.27875734969026311, 5.356774720514425603, 24.00402280011862288 ) ) ;
#4644 = CARTESIAN_POINT ( 'NONE',  ( -28.50259040100463181, -23.79745624473767762, 10.65365253163527193 ) ) ;
#4645 = CARTESIAN_POINT ( 'NONE',  ( 15.37486457892753400, -3.577890193782784500, -28.28298033016822899 ) ) ;
#4646 = CARTESIAN_POINT ( 'NONE',  ( 19.63682106917175929, 6.691539877478525966, -1.500000000000002220 ) ) ;
#4647 = CARTESIAN_POINT ( 'NONE',  ( 5.343276940429747768, -21.04383479052346217, 11.49999999999999645 ) ) ;
#4648 = VERTEX_POINT ( 'NONE', #76115 ) ;
#4649 = EDGE_CURVE ( 'NONE', #73442, #420, #55332, .T. ) ;
#4650 = CARTESIAN_POINT ( 'NONE',  ( -70.62287095715005592, -24.99156045073392463, 7.747789690856161648 ) ) ;
#4651 = CARTESIAN_POINT ( 'NONE',  ( -119.6228709571500417, -24.66019654487199730, 8.947790411086121054 ) ) ;
#4652 = CARTESIAN_POINT ( 'NONE',  ( 21.09243369641204069, 7.689775423913054908, 11.49999999999998934 ) ) ;
#4653 = VECTOR ( 'NONE', #58754, 1000.000000000000114 ) ;
#4654 = EDGE_CURVE ( 'NONE', #36107, #17029, #8046, .T. ) ;
#4655 = CARTESIAN_POINT ( 'NONE',  ( 30.73873608389078527, -2.297196155479623414, 24.67598410064775294 ) ) ;
#4656 = CARTESIAN_POINT ( 'NONE',  ( -34.92287095715006018, -23.47596703998600276, 11.44779298504227683 ) ) ;
#4657 = ORIENTED_EDGE ( 'NONE', *, *, #33502, .T. ) ;
#4658 = CARTESIAN_POINT ( 'NONE',  ( -98.52287095715006160, -23.47596703998600631, 11.44779298504228215 ) ) ;
#4659 = CARTESIAN_POINT ( 'NONE',  ( -41.46611000704998418, -25.27828342519987359, 4.188173683033348915 ) ) ;
#4660 = EDGE_CURVE ( 'NONE', #89884, #94148, #79125, .T. ) ;
#4661 = ORIENTED_EDGE ( 'NONE', *, *, #52630, .T. ) ;
#4662 = ADVANCED_FACE ( 'NONE', ( #56320 ), #95856, .T. ) ;
#4663 = ORIENTED_EDGE ( 'NONE', *, *, #74985, .F. ) ;
#4664 = CARTESIAN_POINT ( 'NONE',  ( -46.64014493302430253, -24.15620529776627379, 10.23563542870660825 ) ) ;
#4665 = ORIENTED_EDGE ( 'NONE', *, *, #77473, .T. ) ;
#4666 = CARTESIAN_POINT ( 'NONE',  ( 17.95810460983813783, 11.44545274529666479, -1.500000000000002220 ) ) ;
#4667 = EDGE_LOOP ( 'NONE', ( #64096, #75030, #66816, #87741 ) ) ;
#4668 = PLANE ( 'NONE',  #8947 ) ;
#4669 = CARTESIAN_POINT ( 'NONE',  ( 8.107222467604051630, 20.28165043084963060, -1.500000000000002220 ) ) ;
#4670 = FACE_OUTER_BOUND ( 'NONE', #34109, .T. ) ;
#4671 = CARTESIAN_POINT ( 'NONE',  ( -1.179572987637725889, 22.66035800735570049, 11.49999999999998934 ) ) ;
#4672 = AXIS2_PLACEMENT_3D ( 'NONE', #89717, #49668, #11090 ) ;
#4673 = CARTESIAN_POINT ( 'NONE',  ( -40.55984193903805846, -25.18430871972357465, 3.296901506826879658 ) ) ;
#4674 = CARTESIAN_POINT ( 'NONE',  ( -28.98875734969026396, 5.965225279485572685, -0.08597719988137648983 ) ) ;
#4675 = CARTESIAN_POINT ( 'NONE',  ( 6.821863743248424150, 20.85434273413645911, -1.500000000000002220 ) ) ;
#4676 = CARTESIAN_POINT ( 'NONE',  ( 3.787259615384621192, -6.376774720514426065, 21.48076923076922640 ) ) ;
#4677 = ORIENTED_EDGE ( 'NONE', *, *, #29638, .F. ) ;
#4678 = ADVANCED_FACE ( 'NONE', ( #16724 ), #10118, .F. ) ;
#4679 = CARTESIAN_POINT ( 'NONE',  ( 29.67488939790761648, -5.972177877498852538, 27.69255262365155801 ) ) ;
#4680 = CARTESIAN_POINT ( 'NONE',  ( -110.3346797185884327, -29.50249014687182836, 3.293933732389337621 ) ) ;
#4681 = ORIENTED_EDGE ( 'NONE', *, *, #40955, .F. ) ;
#4682 = CARTESIAN_POINT ( 'NONE',  ( -30.60135620917391108, -24.67298148219492759, 8.885272145915891429 ) ) ;
#4683 = B_SPLINE_CURVE_WITH_KNOTS ( 'NONE', 3,
 ( #73401, #43941, #82985, #44447, #74874, #67796 ),
 .UNSPECIFIED., .F., .F.,
 ( 4, 2, 4 ),
 ( 6.389872268825926790E-06, 0.001387607747329055096, 0.002768825622389284574 ),
 .UNSPECIFIED. ) ;
#4684 = CARTESIAN_POINT ( 'NONE',  ( -128.5228709571500758, -23.47596703998600631, 11.44779298504227683 ) ) ;
#4685 = CARTESIAN_POINT ( 'NONE',  ( -30.62897883088349005, -24.04641872041738893, -0.4716817114508958242 ) ) ;
#4686 = CARTESIAN_POINT ( 'NONE',  ( 4.782327729912362990, -20.71560727227588927, 11.49999999999998934 ) ) ;
#4687 = CARTESIAN_POINT ( 'NONE',  ( -112.5880318784174534, -24.51314013834317151, 0.6176544820404282765 ) ) ;
#4688 = CARTESIAN_POINT ( 'NONE',  ( -26.09735693242928534, -24.75186533036128367, 4.864566394564080021 ) ) ;
#4689 = CARTESIAN_POINT ( 'NONE',  ( 5.202077965628057576, 2.038091937962834166, 2.869745073849996442E-16 ) ) ;
#4690 = CARTESIAN_POINT ( 'NONE',  ( -129.5228709571499905, -23.48783264082477729, -1.443836473390079700 ) ) ;
#4691 = DIRECTION ( 'NONE',  ( -3.773278334453080206E-23, 0.9999999999976377785, 2.173523156925979975E-06 ) ) ;
#4692 = ORIENTED_EDGE ( 'NONE', *, *, #61961, .F. ) ;
#4693 = CARTESIAN_POINT ( 'NONE',  ( 14.99095386781537975, 12.61000069877385421, 11.49999999999999645 ) ) ;
#4694 = CARTESIAN_POINT ( 'NONE',  ( -42.92287095715004597, -23.47593901973090169, -1.443836447538997980 ) ) ;
#4695 = CARTESIAN_POINT ( 'NONE',  ( -28.42960646346242015, -24.73443543797376520, 8.111062014341033688 ) ) ;
#4696 = EDGE_CURVE ( 'NONE', #98343, #60391, #45621, .T. ) ;
#4697 = ORIENTED_EDGE ( 'NONE', *, *, #6536, .T. ) ;
#4698 = LINE ( 'NONE', #35648, #16572 ) ;
#4699 = CARTESIAN_POINT ( 'NONE',  ( -99.30030995969208618, -25.31470181650071183, 5.154044150389992751 ) ) ;
#4700 = DIRECTION ( 'NONE',  ( 0.000000000000000000, -2.173523156925979552E-06, 0.9999999999976378895 ) ) ;
#4701 = CARTESIAN_POINT ( 'NONE',  ( 0.1645010273463760886, 0.3687607960183654776, 1.417169167140628794 ) ) ;
#4702 = CARTESIAN_POINT ( 'NONE',  ( 5.252985061998082017, 18.97096265210048571, -1.500000000000002220 ) ) ;
#4703 = ORIENTED_EDGE ( 'NONE', *, *, #67950, .T. ) ;
#4704 = CARTESIAN_POINT ( 'NONE',  ( 33.61456970919601872, 6.376774720514426953, -11.35828564741663627 ) ) ;
#4705 = DIRECTION ( 'NONE',  ( 0.000000000000000000, 0.000000000000000000, 1.000000000000000000 ) ) ;
#4706 = PERSON_AND_ORGANIZATION ( #70597, #27821 ) ;
#4707 = ADVANCED_FACE ( 'NONE', ( #48704 ), #98237, .T. ) ;
#4708 = ORIENTED_EDGE ( 'NONE', *, *, #34887, .F. ) ;
#4709 = CARTESIAN_POINT ( 'NONE',  ( 8.971512145086501633, -1.000000000000000000, 3.746884140868835367 ) ) ;
#4710 = CARTESIAN_POINT ( 'NONE',  ( -45.62287095715004881, -24.83620972994591725, 8.398175272781360334 ) ) ;
#4711 = FACE_OUTER_BOUND ( 'NONE', #67913, .T. ) ;
#4712 = CARTESIAN_POINT ( 'NONE',  ( -84.55620429048340725, -23.47596703998600631, 11.44779298504227683 ) ) ;
#4713 = FACE_OUTER_BOUND ( 'NONE', #66376, .T. ) ;
#4714 = AXIS2_PLACEMENT_3D ( 'NONE', #59667, #27211, #58165 ) ;
#4715 = AXIS2_PLACEMENT_3D ( 'NONE', #50924, #43803, #34696 ) ;
#4716 = CARTESIAN_POINT ( 'NONE',  ( -128.6228709571500417, -29.50247984919015209, -1.443849546365044922 ) ) ;
#4717 = CARTESIAN_POINT ( 'NONE',  ( -107.5944960464543243, -23.73766607897672642, -1.055555164236427590 ) ) ;
#4718 = CARTESIAN_POINT ( 'NONE',  ( 1.593314845114734535, -19.89410510517485164, -1.500000000000002220 ) ) ;
#4719 = ADVANCED_FACE ( 'NONE', ( #78610, #40075 ), #64443, .F. ) ;
#4720 = DIRECTION ( 'NONE',  ( -0.000000000000000000, -1.000000000000000000, -0.000000000000000000 ) ) ;
#4721 = CARTESIAN_POINT ( 'NONE',  ( -0.07405751743314503699, -22.09126723942814863, 0.2209411766731599891 ) ) ;
#4722 = EDGE_LOOP ( 'NONE', ( #83104, #17806, #68796, #28133 ) ) ;
#4723 = AXIS2_PLACEMENT_3D ( 'NONE', #6512, #76005, #21221 ) ;
#4724 = DIRECTION ( 'NONE',  ( 0.7071067811865442421, 0.000000000000000000, -0.7071067811865507924 ) ) ;
#4725 = CARTESIAN_POINT ( 'NONE',  ( 13.91401389203221406, 3.316774720514426456, 158.0376437107427137 ) ) ;
#4726 = CARTESIAN_POINT ( 'NONE',  ( 10.86431179148764770, -6.376774720514934991, -28.05678185045468709 ) ) ;
#4727 = CARTESIAN_POINT ( 'NONE',  ( -124.6622648968966871, -25.28354030677812148, 5.756449734795270778 ) ) ;
#4728 = CARTESIAN_POINT ( 'NONE',  ( -81.63689468831775287, -23.96119346886881019, -0.6495511937831893734 ) ) ;
#4729 = VECTOR ( 'NONE', #35434, 1000.000000000000000 ) ;
#4730 = CARTESIAN_POINT ( 'NONE',  ( -26.09825697877282735, -24.96875754738233866, 4.795748209963784703 ) ) ;
#4731 = CC_DESIGN_DATE_AND_TIME_ASSIGNMENT ( #34918, #1090, ( #19830 ) ) ;
#4732 = CARTESIAN_POINT ( 'NONE',  ( -88.62287095715004170, -24.64898659630367916, 1.056161002820827921 ) ) ;
#4733 = ORIENTED_EDGE ( 'NONE', *, *, #82537, .F. ) ;
#4734 = CARTESIAN_POINT ( 'NONE',  ( 30.53060340732036693, -4.484471217129241793, -4.073950328685796762 ) ) ;
#4735 = CARTESIAN_POINT ( 'NONE',  ( 6.371704462700114924, -6.376774720514427841, 21.83798798526824214 ) ) ;
#4736 = ORIENTED_EDGE ( 'NONE', *, *, #24661, .T. ) ;
#4737 = AXIS2_PLACEMENT_3D ( 'NONE', #42573, #51169, #82115 ) ;
#4738 = CARTESIAN_POINT ( 'NONE',  ( -9.806399893892750796, 17.69452640759178408, -1.500000000000002220 ) ) ;
#4739 = CARTESIAN_POINT ( 'NONE',  ( -2.169994883066378222, 10.75358048763950869, 3.549999999999999822 ) ) ;
#4740 = CARTESIAN_POINT ( 'NONE',  ( 282.9764569301858046, -2.682774720514426559, 20.79159422840526616 ) ) ;
#4741 = CARTESIAN_POINT ( 'NONE',  ( -25.92875734969025814, -5.356774720514425603, 26.43402280011862615 ) ) ;
#4742 = ORIENTED_EDGE ( 'NONE', *, *, #80825, .F. ) ;
#4743 = CARTESIAN_POINT ( 'NONE',  ( -78.97891443407796430, -25.30125878307690357, 5.600169338922809104 ) ) ;
#4744 = DIRECTION ( 'NONE',  ( 0.000000000000000000, -0.9999999999976377785, -2.173523156925979128E-06 ) ) ;
#4745 = CARTESIAN_POINT ( 'NONE',  ( -10.42242239376218116, -17.14354752861867937, -1.500000000000002220 ) ) ;
#4746 = CARTESIAN_POINT ( 'NONE',  ( -2.129267666952235682, 20.92775224702969439, 11.49999999999999645 ) ) ;
#4747 = CARTESIAN_POINT ( 'NONE',  ( -116.4728709571500360, -25.40558663563427189, 5.000950442582703381 ) ) ;
#4748 = CARTESIAN_POINT ( 'NONE',  ( -70.57978950566615595, -24.92592662359561118, 8.075495903017998245 ) ) ;
#4749 = CARTESIAN_POINT ( 'NONE',  ( -16.08457400211760913, 15.13120210334024662, -1.500000000000002220 ) ) ;
#4750 = CARTESIAN_POINT ( 'NONE',  ( -40.31138024738270786, -25.31589329286174817, 5.079523608772094967 ) ) ;
#4751 = CARTESIAN_POINT ( 'NONE',  ( -71.30457154551150722, -25.25559839591754496, 6.209207386190694677 ) ) ;
#4752 = CARTESIAN_POINT ( 'NONE',  ( -50.40445135320380388, -25.27344759577556843, 3.293942924311254572 ) ) ;
#4753 = ORIENTED_EDGE ( 'NONE', *, *, #88211, .F. ) ;
#4754 = CARTESIAN_POINT ( 'NONE',  ( -89.81226385320383088, -29.50249691823240994, 6.409318347766594037 ) ) ;
#4755 = B_SPLINE_SURFACE_WITH_KNOTS ( 'NONE', 3, 3, ( 
 ( #62778, #31299, #62266, #96212 ),
 ( #33297, #64789, #33807, #10970 ),
 ( #25183, #80978, #42439, #17577 ),
 ( #88103, #40423, #48549, #18572 ),
 ( #57165, #49047, #65782, #25690 ),
 ( #88599, #9967, #71380, #49546 ),
 ( #56160, #19071, #57657, #64283 ) ),
 .UNSPECIFIED., .F., .F., .F.,
 ( 4, 3, 4 ),
 ( 4, 4 ),
 ( 0.0004766839783822500432, 0.1029713700210897753, 0.2054660560637973088 ),
 ( 0.3295778362189659139, 0.3307426273830550989 ),
 .UNSPECIFIED. ) ;
#4756 = CARTESIAN_POINT ( 'NONE',  ( -31.62287095715006657, -24.34917612406837506, 0.1852690917426561001 ) ) ;
#4757 = VERTEX_POINT ( 'NONE', #31957 ) ;
#4758 = ORIENTED_EDGE ( 'NONE', *, *, #13788, .F. ) ;
#4759 = DIRECTION ( 'NONE',  ( -0.000000000000000000, 2.173523156925979552E-06, -0.9999999999976378895 ) ) ;
#4760 = LINE ( 'NONE', #66687, #16211 ) ;
#4761 = CARTESIAN_POINT ( 'NONE',  ( -89.62287095714999907, -23.96127896941631619, -0.6493128931037825957 ) ) ;
#4762 = CARTESIAN_POINT ( 'NONE',  ( -19.39287000742378453, 6.875061630626206011, -1.500000000000002220 ) ) ;
#4763 = CARTESIAN_POINT ( 'NONE',  ( -21.33164055427280914, -3.227942221655450972, 11.49999999999999645 ) ) ;
#4764 = ORIENTED_EDGE ( 'NONE', *, *, #91347, .T. ) ;
#4765 = LINE ( 'NONE', #96118, #38057 ) ;
#4766 = CARTESIAN_POINT ( 'NONE',  ( 3.176458874063931681, 0.3587747205143967943, -28.85257003503889806 ) ) ;
#4767 = CARTESIAN_POINT ( 'NONE',  ( -97.52287095715010423, -23.48783264082477018, -1.443836473390087027 ) ) ;
#4768 = CARTESIAN_POINT ( 'NONE',  ( 20.23429811176546167, 9.490607074118958764, -1.500000000000002220 ) ) ;
#4769 = CARTESIAN_POINT ( 'NONE',  ( 32.53346577320676403, -1.682774720514426114, -11.93731717363829681 ) ) ;
#4770 = FACE_OUTER_BOUND ( 'NONE', #63705, .T. ) ;
#4771 = ORIENTED_EDGE ( 'NONE', *, *, #23500, .T. ) ;
#4772 = CYLINDRICAL_SURFACE ( 'NONE', #35577, 28.96799999999999642 ) ;
#4773 = CARTESIAN_POINT ( 'NONE',  ( -51.66770628948501098, -25.28171047118814840, 4.239413304054294507 ) ) ;
#4774 = EDGE_CURVE ( 'NONE', #99954, #24488, #62929, .T. ) ;
#4775 = CARTESIAN_POINT ( 'NONE',  ( 16.07097863352054290, 13.35096362007907622, 11.49999999999998934 ) ) ;
#4776 = EDGE_CURVE ( 'NONE', #60884, #63331, #22581, .T. ) ;
#4777 = ORIENTED_EDGE ( 'NONE', *, *, #20848, .T. ) ;
#4779 = ORIENTED_EDGE ( 'NONE', *, *, #52740, .T. ) ;
#4778 = CARTESIAN_POINT ( 'NONE',  ( -92.55620429048339304, -24.65952944569304606, 1.056160979905701680 ) ) ;
#4780 = VERTEX_POINT ( 'NONE', #33960 ) ;
#4781 = CARTESIAN_POINT ( 'NONE',  ( -100.5540350906619409, -24.15602025860896163, 10.28564288303535790 ) ) ;
#4782 = CARTESIAN_POINT ( 'NONE',  ( -18.69274626484788371, 9.848020819832786543, -1.500000000000002220 ) ) ;
#4783 = ORIENTED_EDGE ( 'NONE', *, *, #16436, .F. ) ;
#4784 = CARTESIAN_POINT ( 'NONE',  ( -91.52287095715010423, -24.66019654487199730, 8.947790411086115725 ) ) ;
#4785 = CARTESIAN_POINT ( 'NONE',  ( -102.6228709571500275, -23.95044443724990657, 10.65354141964649592 ) ) ;
#4786 = CARTESIAN_POINT ( 'NONE',  ( -61.52287095715006160, -23.48786465467241058, 11.44779295918254824 ) ) ;
#4787 = AXIS2_PLACEMENT_3D ( 'NONE', #17343, #48304, #71639 ) ;
#4788 = CARTESIAN_POINT ( 'NONE',  ( -76.54257616626556171, -24.51419770103157347, 9.386484678747176957 ) ) ;
#4789 = CARTESIAN_POINT ( 'NONE',  ( 7.275731542451676859, -5.876774720514415407, 20.06332870126568224 ) ) ;
#4790 = CARTESIAN_POINT ( 'NONE',  ( -21.76810506448615712, 0.6044244127108716613, -1.500000000000002220 ) ) ;
#4791 = CARTESIAN_POINT ( 'NONE',  ( -80.83723253079826065, -25.24759792921647872, 7.046395315168356710 ) ) ;
#4793 = ORIENTED_EDGE ( 'NONE', *, *, #4654, .T. ) ;
#4792 = CARTESIAN_POINT ( 'NONE',  ( 22.20884612314100792, -2.053178116692622623, 11.49999999999999645 ) ) ;
#4794 = ADVANCED_FACE ( 'NONE', ( #32966 ), #29504, .T. ) ;
#4795 = CARTESIAN_POINT ( 'NONE',  ( -19.77875734969026311, -5.356774720514426491, 27.45402280011862217 ) ) ;
#4796 = CARTESIAN_POINT ( 'NONE',  ( -20.27875734969026311, 7.743225279485574042, 24.00402280011862288 ) ) ;
#4797 = CARTESIAN_POINT ( 'NONE',  ( -36.62287095715005592, -23.48786465467240347, 11.44779295918255180 ) ) ;
#4798 = ORIENTED_EDGE ( 'NONE', *, *, #2142, .T. ) ;
#4799 = AXIS2_PLACEMENT_3D ( 'NONE', #88391, #2666, #9253 ) ;
#4801 = ORIENTED_EDGE ( 'NONE', *, *, #57917, .F. ) ;
#4800 = CARTESIAN_POINT ( 'NONE',  ( -40.62287095715005592, -23.48783264082478084, -1.443836473390072817 ) ) ;
#4802 = AXIS2_PLACEMENT_3D ( 'NONE', #74244, #96092, #57543 ) ;
#4803 = ORIENTED_EDGE ( 'NONE', *, *, #40787, .F. ) ;
#4804 = AXIS2_PLACEMENT_3D ( 'NONE', #83098, #62662, #55547 ) ;
#4805 = CARTESIAN_POINT ( 'NONE',  ( -95.58953762381672448, -24.99156044556120193, 7.747789690856343725 ) ) ;
#4806 = CARTESIAN_POINT ( 'NONE',  ( -86.55620429048336462, -23.47596703998600631, 11.44779298504227683 ) ) ;
#4807 = CARTESIAN_POINT ( 'NONE',  ( -49.65643811812167741, -25.31518051169904027, 4.891465044530135309 ) ) ;
#4808 = VECTOR ( 'NONE', #62200, 1000.000000000000114 ) ;
#4809 = CARTESIAN_POINT ( 'NONE',  ( -35.52287095715006870, -24.91544648472619627, 1.928969306349232582 ) ) ;
#4810 = CARTESIAN_POINT ( 'NONE',  ( -66.52287095715006160, -23.47596703998600631, 11.44779298504228748 ) ) ;
#4811 = ORIENTED_EDGE ( 'NONE', *, *, #60333, .F. ) ;
#4812 = CARTESIAN_POINT ( 'NONE',  ( -18.22047185089115828, 6.579378235550767506, 11.49999999999999645 ) ) ;
#4813 = DIRECTION ( 'NONE',  ( 4.335561085774420994E-16, 0.000000000000000000, -1.000000000000000000 ) ) ;
#4814 = ORIENTED_EDGE ( 'NONE', *, *, #40684, .F. ) ;
#4815 = CARTESIAN_POINT ( 'NONE',  ( 3.160575456146155204, -5.876774720514408301, 18.86877352677795372 ) ) ;
#4816 = CARTESIAN_POINT ( 'NONE',  ( 2.677564053859940341, -6.376774720514406525, 19.16116138973293559 ) ) ;
#4817 = CARTESIAN_POINT ( 'NONE',  ( -102.6228709571500133, -23.96127896941632685, -0.6493128931037813745 ) ) ;
#4818 = CARTESIAN_POINT ( 'NONE',  ( -48.52287095715006160, -29.50250243563736774, 8.947779886222146928 ) ) ;
#4819 = EDGE_CURVE ( 'NONE', #65087, #69040, #26198, .T. ) ;
#4820 = CARTESIAN_POINT ( 'NONE',  ( -15.04504930077994196, -12.58455232801425794, -1.500000000000002220 ) ) ;
#4821 = CARTESIAN_POINT ( 'NONE',  ( -116.5228709571500616, -24.65952944569305316, 1.056160979905705899 ) ) ;
#4822 = EDGE_LOOP ( 'NONE', ( #40471, #35218, #4197, #47443 ) ) ;
#4823 = CARTESIAN_POINT ( 'NONE',  ( -7.189238790567602067, -20.27908067168375794, 11.49999999999998934 ) ) ;
#4824 = CARTESIAN_POINT ( 'NONE',  ( 21.57151214508649772, 3.625915217019311583E-15, -1.699999999999999956 ) ) ;
#4825 = CARTESIAN_POINT ( 'NONE',  ( -81.28341456819592281, -25.30394797635934978, 5.143804183213717351 ) ) ;
#4826 = CARTESIAN_POINT ( 'NONE',  ( -40.67672227337696000, -23.48783264082477018, -1.443836473390102570 ) ) ;
#4827 = CARTESIAN_POINT ( 'NONE',  ( 8.071512145086501278, -1.000000000000004441, 1.702924846563847311E-15 ) ) ;
#4828 = CARTESIAN_POINT ( 'NONE',  ( -5.582908757718670678, 22.30220962497079285, -1.500000000000002220 ) ) ;
#4829 = ADVANCED_FACE ( 'NONE', ( #26848 ), #58311, .F. ) ;
#4830 = PERSON_AND_ORGANIZATION ( #70597, #27821 ) ;
#4831 = FACE_OUTER_BOUND ( 'NONE', #28425, .T. ) ;
#4832 = FACE_OUTER_BOUND ( 'NONE', #20359, .T. ) ;
#4833 = CARTESIAN_POINT ( 'NONE',  ( -18.21026628907936029, 8.684577975296603469, 11.49999999999999645 ) ) ;
#4834 = CARTESIAN_POINT ( 'NONE',  ( -101.6228709571500559, -24.64898659630368627, 1.056161002820829697 ) ) ;
#4835 = DIRECTION ( 'NONE',  ( 0.000000000000000000, 0.000000000000000000, -1.000000000000000000 ) ) ;
#4836 = CARTESIAN_POINT ( 'NONE',  ( -4.141439336867657417, -5.876774720514418071, 20.56083401959468304 ) ) ;
#4837 = DIRECTION ( 'NONE',  ( -2.205762779227727030E-17, 9.949552925324065630E-17, 1.000000000000000000 ) ) ;
#4838 = DIRECTION ( 'NONE',  ( 0.000000000000000000, 0.000000000000000000, 1.000000000000000000 ) ) ;
#4839 = CARTESIAN_POINT ( 'NONE',  ( -19.55781625546462976, 3.520333346782119843, -1.500000000000002220 ) ) ;
#4840 = CARTESIAN_POINT ( 'NONE',  ( -113.5917735524323575, -23.96119346886881374, -0.6495511937832029181 ) ) ;
#4841 = CARTESIAN_POINT ( 'NONE',  ( 2.412641546452875208, 19.58572291230954221, -1.500000000000002220 ) ) ;
#4842 = CARTESIAN_POINT ( 'NONE',  ( -42.49248349598780550, -24.34968618360933590, 0.1864209137778841952 ) ) ;
#4843 = DIRECTION ( 'NONE',  ( 0.000000000000000000, 1.000000000000000000, -0.000000000000000000 ) ) ;
#4844 = CYLINDRICAL_SURFACE ( 'NONE', #84782, 2.249999999999998668 ) ;
#4845 = CARTESIAN_POINT ( 'NONE',  ( 4.906390264955167169, 20.09725327650800608, 11.49999999999999645 ) ) ;
#4846 = CARTESIAN_POINT ( 'NONE',  ( 7.477175500793984853, -6.376774720514417183, 20.66439772633092176 ) ) ;
#4847 = VECTOR ( 'NONE', #16656, 1000.000000000000114 ) ;
#4848 = EDGE_CURVE ( 'NONE', #13991, #56450, #75558, .T. ) ;
#4849 = CARTESIAN_POINT ( 'NONE',  ( 30.93898937471034216, 4.884441105398384941, -1.603546260404424606 ) ) ;
#4850 = EDGE_CURVE ( 'NONE', #80, #17025, #89749, .T. ) ;
#4851 = CARTESIAN_POINT ( 'NONE',  ( 5.572475817582897228, 21.94689365879375131, 11.49999999999999645 ) ) ;
#4852 = ORIENTED_EDGE ( 'NONE', *, *, #28818, .F. ) ;
#4853 = LINE ( 'NONE', #81977, #12221 ) ;
#4854 = CARTESIAN_POINT ( 'NONE',  ( 30.63451081005166543, 4.279369518130740069, 28.08236555530620038 ) ) ;
#4855 = VECTOR ( 'NONE', #55433, 1000.000000000000000 ) ;
#4856 = B_SPLINE_CURVE_WITH_KNOTS ( 'NONE', 3,
 ( #50875, #12286, #49888, #80820 ),
 .UNSPECIFIED., .F., .F.,
 ( 4, 4 ),
 ( 0.000000000000000000, 9.999999999997510880E-05 ),
 .UNSPECIFIED. ) ;
#4857 = CARTESIAN_POINT ( 'NONE',  ( -60.55620429048339304, -23.47593901973091235, -1.443836447539007972 ) ) ;
#4858 = CARTESIAN_POINT ( 'NONE',  ( 32.88562546571903056, 5.965225279485572685, -5.083907541707159972 ) ) ;
#4859 = ADVANCED_FACE ( 'NONE', ( #3520 ), #43082, .T. ) ;
#4860 = VECTOR ( 'NONE', #89035, 1000.000000000000000 ) ;
#4861 = ORIENTED_EDGE ( 'NONE', *, *, #63900, .T. ) ;
#4862 = ORIENTED_EDGE ( 'NONE', *, *, #92201, .F. ) ;
#4863 = CARTESIAN_POINT ( 'NONE',  ( -100.4426124108961176, -25.12298712672051337, 7.101635559041870494 ) ) ;
#4864 = CARTESIAN_POINT ( 'NONE',  ( 5.898633191892585614, -22.09092271590295198, 11.49999999999998934 ) ) ;
#4865 = CARTESIAN_POINT ( 'NONE',  ( 2.230654205607476293, -6.505213034913026604E-16, -0.1647943925233646134 ) ) ;
#4866 = VECTOR ( 'NONE', #28348, 1000.000000000000000 ) ;
#4867 = CARTESIAN_POINT ( 'NONE',  ( 0.7969447072908428797, -21.54811710690876225, -1.500000000000002220 ) ) ;
#4868 = CARTESIAN_POINT ( 'NONE',  ( -113.5904876474596534, -24.15620529776628800, 10.23563542870659582 ) ) ;
#4869 = CARTESIAN_POINT ( 'NONE',  ( -99.16166289166535819, -29.50249453179804249, 5.311361616999957569 ) ) ;
#4870 = B_SPLINE_CURVE_WITH_KNOTS ( 'NONE', 3,
 ( #23645, #49011, #11434, #18047, #26666, #79944 ),
 .UNSPECIFIED., .F., .F.,
 ( 4, 2, 4 ),
 ( 0.000000000000000000, 0.001380764517854766700, 0.002761529035709533401 ),
 .UNSPECIFIED. ) ;
#4871 = CARTESIAN_POINT ( 'NONE',  ( -5.199590022849982063, -21.90925200621149571, 11.49999999999999645 ) ) ;
#4872 = ORIENTED_EDGE ( 'NONE', *, *, #71817, .F. ) ;
#4873 = CIRCLE ( 'NONE', #61598, 0.3000000000000016542 ) ;
#4874 = CARTESIAN_POINT ( 'NONE',  ( -12.84880425037203011, -5.965225279485592225, -26.59900746623528534 ) ) ;
#4875 = CARTESIAN_POINT ( 'NONE',  ( 19.92286461850947887, -9.344431347164146473, -1.500000000000002220 ) ) ;
#4877 = CARTESIAN_POINT ( 'NONE',  ( -111.5158263670924725, -24.34968618360933945, 0.1864209137778883862 ) ) ;
#4876 = AXIS2_PLACEMENT_3D ( 'NONE', #17911, #86914, #95531 ) ;
#4878 = LINE ( 'NONE', #49065, #28178 ) ;
#4879 = ORIENTED_EDGE ( 'NONE', *, *, #44154, .F. ) ;
#4880 = FACE_OUTER_BOUND ( 'NONE', #20010, .T. ) ;
#4881 = CARTESIAN_POINT ( 'NONE',  ( -111.6228709571500559, -23.47593901973091235, -1.443836447538999312 ) ) ;
#4882 = ORIENTED_EDGE ( 'NONE', *, *, #55562, .F. ) ;
#4883 = CARTESIAN_POINT ( 'NONE',  ( -77.62287095715005592, -24.33832256526968862, 0.1851278514119851781 ) ) ;
#4884 = ORIENTED_EDGE ( 'NONE', *, *, #52048, .T. ) ;
#4885 = EDGE_CURVE ( 'NONE', #44866, #18999, #81636, .T. ) ;
#4886 = ORIENTED_EDGE ( 'NONE', *, *, #52235, .F. ) ;
#4887 = EDGE_CURVE ( 'NONE', #57623, #21668, #96858, .T. ) ;
#4888 = CARTESIAN_POINT ( 'NONE',  ( -65.52287095715011844, -24.82558206586142902, 1.605769216559445711 ) ) ;
#4889 = CARTESIAN_POINT ( 'NONE',  ( -42.52287095715005449, -29.50250243563736774, 8.947779886222148704 ) ) ;
#4890 = CARTESIAN_POINT ( 'NONE',  ( -57.60487000211600872, -23.73766607897670866, -1.055555164236458454 ) ) ;
#4891 = CARTESIAN_POINT ( 'NONE',  ( -15.55180764702766716, 13.24544322234432414, -1.500000000000002220 ) ) ;
#4892 = ORIENTED_EDGE ( 'NONE', *, *, #85333, .F. ) ;
#4893 = CARTESIAN_POINT ( 'NONE',  ( -128.5228709571500758, -23.47596703998600631, 11.44779298504227683 ) ) ;
#4894 = CARTESIAN_POINT ( 'NONE',  ( -115.6228709571500559, -24.99156045073393173, 7.747789690856161648 ) ) ;
#4895 = CARTESIAN_POINT ( 'NONE',  ( -105.5848504283774218, -25.00158670708910691, 2.256160236439218369 ) ) ;
#4896 = CARTESIAN_POINT ( 'NONE',  ( -71.70841769935766763, -25.03149551985922017, 6.192981911745003565 ) ) ;
#4897 = VERTEX_POINT ( 'NONE', #44072 ) ;
#4898 = CARTESIAN_POINT ( 'NONE',  ( -123.2228709571500502, -23.47593901973090524, -1.443836447538996426 ) ) ;
#4899 = CARTESIAN_POINT ( 'NONE',  ( -86.58953762381672448, -23.48786465467241413, 11.44779295918254469 ) ) ;
#4900 = ORIENTED_EDGE ( 'NONE', *, *, #96045, .T. ) ;
#4901 = CARTESIAN_POINT ( 'NONE',  ( 10.19739565540945492, -18.13666118385682680, 11.49999999999998934 ) ) ;
#4902 = EDGE_CURVE ( 'NONE', #31312, #83417, #33381, .T. ) ;
#4903 = EDGE_LOOP ( 'NONE', ( #81792, #24502, #73472, #71560 ) ) ;
#4905 = ORIENTED_EDGE ( 'NONE', *, *, #17942, .F. ) ;
#4904 = CARTESIAN_POINT ( 'NONE',  ( -39.49573010990816613, -25.29496779178032284, 4.491406335818826534 ) ) ;
#4906 = EDGE_CURVE ( 'NONE', #64208, #29097, #97361, .T. ) ;
#4907 = CARTESIAN_POINT ( 'NONE',  ( -68.52287095715006160, -23.47596703998600631, 11.44779298504228748 ) ) ;
#4908 = CARTESIAN_POINT ( 'NONE',  ( -115.5228709571500190, -24.62226745350438506, 0.9660975649728118508 ) ) ;
#4909 = ORIENTED_EDGE ( 'NONE', *, *, #44345, .T. ) ;
#4910 = EDGE_LOOP ( 'NONE', ( #12098, #31468, #8888, #17356 ) ) ;
#4911 = B_SPLINE_CURVE_WITH_KNOTS ( 'NONE', 3,
 ( #67423, #97848, #28851, #44576 ),
 .UNSPECIFIED., .F., .F.,
 ( 4, 4 ),
 ( 0.000000000000000000, 0.0001000000000000167422 ),
 .UNSPECIFIED. ) ;
#4912 = CARTESIAN_POINT ( 'NONE',  ( -68.62287095715005592, -29.50247984919015209, -1.443849546365055359 ) ) ;
#4913 = CARTESIAN_POINT ( 'NONE',  ( -64.52287095715006160, -23.73934037231756022, 11.05740245334328975 ) ) ;
#4914 = FACE_OUTER_BOUND ( 'NONE', #19401, .T. ) ;
#4915 = CARTESIAN_POINT ( 'NONE',  ( -43.66335654702338331, -23.48786465467240347, 11.44779295918255180 ) ) ;
#4917 = ORIENTED_EDGE ( 'NONE', *, *, #54639, .T. ) ;
#4916 = CARTESIAN_POINT ( 'NONE',  ( 11.82310115920509830, 18.66461490495635545, 11.49999999999999645 ) ) ;
#4918 = ADVANCED_FACE ( 'NONE', ( #58799 ), #35965, .T. ) ;
#4919 = B_SPLINE_CURVE_WITH_KNOTS ( 'NONE', 3,
 ( #27922, #89329, #44151, #27432 ),
 .UNSPECIFIED., .F., .F.,
 ( 4, 4 ),
 ( 0.000000000000000000, 9.999999999998900014E-05 ),
 .UNSPECIFIED. ) ;
#4920 = CARTESIAN_POINT ( 'NONE',  ( -108.5923759227193699, -23.96119346886881374, -0.6495511937831862648 ) ) ;
#4921 = CARTESIAN_POINT ( 'NONE',  ( 8.141615846073909424, -21.09679883994429161, -1.500000000000002220 ) ) ;
#4922 = ADVANCED_FACE ( 'NONE', ( #45081 ), #46078, .T. ) ;
#4924 = VERTEX_POINT ( 'NONE', #75502 ) ;
#4923 = CARTESIAN_POINT ( 'NONE',  ( -115.5143227195287068, -24.83644354573579349, 8.397322867130096569 ) ) ;
#4925 = ORIENTED_EDGE ( 'NONE', *, *, #89907, .F. ) ;
#4926 = DIRECTION ( 'NONE',  ( 0.000000000000000000, 2.173523156925980399E-06, -0.9999999999976378895 ) ) ;
#4927 = AXIS2_PLACEMENT_3D ( 'NONE', #89375, #95987, #19845 ) ;
#4928 = CARTESIAN_POINT ( 'NONE',  ( -57.59299408741310344, -24.15620529776628089, 10.23563542870660470 ) ) ;
#4929 = ORIENTED_EDGE ( 'NONE', *, *, #6030, .F. ) ;
#4930 = DIRECTION ( 'NONE',  ( -3.773278334453079030E-23, 0.9999999999976377785, 2.173523156925979128E-06 ) ) ;
#4931 = CARTESIAN_POINT ( 'NONE',  ( -18.06118310651259407, 13.05043149098080058, -1.500000000000002220 ) ) ;
#4932 = DIRECTION ( 'NONE',  ( 3.773278334444167608E-23, -1.000000000000000000, 0.000000000000000000 ) ) ;
#4933 = ORIENTED_EDGE ( 'NONE', *, *, #84338, .T. ) ;
#4934 = CARTESIAN_POINT ( 'NONE',  ( -42.52287095715005449, -24.65952944569303895, 1.056160979905691910 ) ) ;
#4935 = FACE_OUTER_BOUND ( 'NONE', #49117, .T. ) ;
#4936 = PLANE ( 'NONE',  #64163 ) ;
#4937 = DIRECTION ( 'NONE',  ( 1.000000000000000000, 0.000000000000000000, -0.000000000000000000 ) ) ;
#4938 = B_SPLINE_CURVE_WITH_KNOTS ( 'NONE', 3,
 ( #87057, #79945, #48009, #9933, #9427, #17547 ),
 .UNSPECIFIED., .F., .F.,
 ( 4, 2, 4 ),
 ( 6.391158118975500541E-06, 0.001387004593080798072, 0.002767618028042620644 ),
 .UNSPECIFIED. ) ;
#4939 = CIRCLE ( 'NONE', #56817, 130.7884398600581335 ) ;
#4940 = CARTESIAN_POINT ( 'NONE',  ( -18.23695082634099407, 6.967386181637144738, 11.49999999999998934 ) ) ;
#4941 = CARTESIAN_POINT ( 'NONE',  ( -16.73372362409233105, 13.38858591273363174, -1.500000000000002220 ) ) ;
#4942 = CARTESIAN_POINT ( 'NONE',  ( -0.9988807608215116707, -5.876774720514410077, 19.30497968945844889 ) ) ;
#4943 = LINE ( 'NONE', #80565, #60078 ) ;
#4944 = CARTESIAN_POINT ( 'NONE',  ( -34.52287095715008292, -24.33832256527048088, 0.1851278514138537667 ) ) ;
#4945 = CARTESIAN_POINT ( 'NONE',  ( -4.374245501123523283, 22.36648047097513725, -1.500000000000002220 ) ) ;
#4946 = VECTOR ( 'NONE', #13039, 1000.000000000000227 ) ;
#4947 = EDGE_CURVE ( 'NONE', #72299, #9262, #37461, .T. ) ;
#4948 = VECTOR ( 'NONE', #26791, 1000.000000000000000 ) ;
#4949 = CARTESIAN_POINT ( 'NONE',  ( 30.53060340732037048, 2.682774720514426559, -2.322449884495168870 ) ) ;
#4950 = CARTESIAN_POINT ( 'NONE',  ( 13.91401389203221406, -0.3587747205144265483, 158.0376437107427137 ) ) ;
#4951 = CARTESIAN_POINT ( 'NONE',  ( 10.26108024787556516, -17.11367029881254709, 11.49999999999999645 ) ) ;
#4952 = CARTESIAN_POINT ( 'NONE',  ( -8.160000000000000142, -9.652339641703484574, 1.628518864987183790 ) ) ;
#4953 = CARTESIAN_POINT ( 'NONE',  ( -6.660000000000001030, -9.572916487583201572, -0.7764348688322061376 ) ) ;
#4954 = CARTESIAN_POINT ( 'NONE',  ( -57.22287095715007865, -23.47596703998600276, 11.44779298504227860 ) ) ;
#4955 = VERTEX_POINT ( 'NONE', #90744 ) ;
#4956 = CARTESIAN_POINT ( 'NONE',  ( -97.52287095715006160, -29.50250243563736774, 8.947779886222138046 ) ) ;
#4957 = CARTESIAN_POINT ( 'NONE',  ( -124.5228709571500616, -24.65952944569305316, 1.056160979905705899 ) ) ;
#4958 = CARTESIAN_POINT ( 'NONE',  ( 12.82194709444435077, -17.51738216156474337, 11.49999999999998934 ) ) ;
#4959 = PLANE ( 'NONE',  #23682 ) ;
#4960 = CARTESIAN_POINT ( 'NONE',  ( -19.08498223313328168, 4.104482590468319536, -1.500000000000002220 ) ) ;
#4961 = DIRECTION ( 'NONE',  ( -0.000000000000000000, -1.000000000000000000, -0.000000000000000000 ) ) ;
#4962 = ORIENTED_EDGE ( 'NONE', *, *, #15618, .T. ) ;
#4963 = PERSON_AND_ORGANIZATION ( #65778, #50715 ) ;
#4964 = CARTESIAN_POINT ( 'NONE',  ( 19.24418710706453339, -0.5000000000000000000, 2.346898003627108320 ) ) ;
#4965 = CARTESIAN_POINT ( 'NONE',  ( -6.584652030910324250, 19.34213596296284265, 11.49999999999999645 ) ) ;
#4966 = DIRECTION ( 'NONE',  ( -3.773278334453079618E-23, 0.9999999999976377785, 2.173523156925979975E-06 ) ) ;
#4967 = LINE ( 'NONE', #6963, #59438 ) ;
#4968 = ADVANCED_FACE ( 'NONE', ( #68409 ), #74847, .T. ) ;
#4969 = ORIENTED_EDGE ( 'NONE', *, *, #27648, .F. ) ;
#4970 = CARTESIAN_POINT ( 'NONE',  ( 31.41423154468143153, 2.682774720514426559, -0.3119954678742140053 ) ) ;
#4971 = PLANE ( 'NONE',  #72115 ) ;
#4972 = DIRECTION ( 'NONE',  ( 2.209838822900391329E-16, 1.000000000000000000, -0.000000000000000000 ) ) ;
#4973 = CARTESIAN_POINT ( 'NONE',  ( -61.62287095715008434, -24.50216790748098816, 0.6166512839513755839 ) ) ;
#4974 = EDGE_LOOP ( 'NONE', ( #70293, #99122, #52309, #56768 ) ) ;
#4975 = EDGE_CURVE ( 'NONE', #31243, #34608, #80016, .T. ) ;
#4976 = CARTESIAN_POINT ( 'NONE',  ( -52.52287095715006870, -24.65952944569303895, 1.056160979905693686 ) ) ;
#4977 = EDGE_CURVE ( 'NONE', #31248, #65701, #41849, .T. ) ;
#4978 = ADVANCED_FACE ( 'NONE', ( #71921 ), #5179, .T. ) ;
#4979 = CARTESIAN_POINT ( 'NONE',  ( 14.37299948674089123, 17.95305339730678185, 11.49999999999999645 ) ) ;
#4980 = CARTESIAN_POINT ( 'NONE',  ( 9.298244000614250382, 20.81247324795305431, -1.500000000000002220 ) ) ;
#4981 = CARTESIAN_POINT ( 'NONE',  ( 0.1645010273463760886, -1.417169167140626573, 0.3687607960183696965 ) ) ;
#4982 = LINE ( 'NONE', #44044, #23697 ) ;
#4983 = DIRECTION ( 'NONE',  ( -1.000000000000000000, -8.503546450866701308E-16, 0.000000000000000000 ) ) ;
#4984 = EDGE_CURVE ( 'NONE', #75656, #54879, #57660, .T. ) ;
#4985 = CARTESIAN_POINT ( 'NONE',  ( -74.52287095715003318, -23.73934037231756022, 11.05740245334328975 ) ) ;
#4986 = CARTESIAN_POINT ( 'NONE',  ( -110.5487009423575842, -24.92564183028978775, 1.928384488918252204 ) ) ;
#4987 = VECTOR ( 'NONE', #56965, 1000.000000000000000 ) ;
#4988 = CARTESIAN_POINT ( 'NONE',  ( -9.857428550561325054, -19.57614489166009264, 11.49999999999998934 ) ) ;
#4989 = DIRECTION ( 'NONE',  ( -3.773278334453079618E-23, 0.9999999999976377785, 2.173523156925979975E-06 ) ) ;
#4990 = DIRECTION ( 'NONE',  ( -3.773278334453079618E-23, 0.9999999999976377785, 2.173523156925979975E-06 ) ) ;
#4991 = CARTESIAN_POINT ( 'NONE',  ( -120.6228709571500275, -24.91544648472626378, 1.928969306349428425 ) ) ;
#4992 = DIRECTION ( 'NONE',  ( 1.000000000000000000, -3.639832272653110612E-15, 0.000000000000000000 ) ) ;
#4993 = VERTEX_POINT ( 'NONE', #33844 ) ;
#4994 = CARTESIAN_POINT ( 'NONE',  ( 20.14718400222343320, -3.498931157112906476, 11.49999999999998934 ) ) ;
#4995 = ORIENTED_EDGE ( 'NONE', *, *, #1253, .F. ) ;
#4996 = ORIENTED_EDGE ( 'NONE', *, *, #63895, .T. ) ;
#4997 = ORIENTED_EDGE ( 'NONE', *, *, #37112, .T. ) ;
#4998 = ORIENTED_EDGE ( 'NONE', *, *, #100417, .F. ) ;
#4999 = EDGE_CURVE ( 'NONE', #63613, #67301, #26733, .T. ) ;
#5000 = CARTESIAN_POINT ( 'NONE',  ( 21.75825945658488436, -7.631246777643061030, -1.500000000000002220 ) ) ;
#5001 = CARTESIAN_POINT ( 'NONE',  ( -61.49891124310355650, -24.34968618360933945, 0.1864209137778810865 ) ) ;
#5002 = CARTESIAN_POINT ( 'NONE',  ( 15.52975653788041122, 12.98207780544785628, -1.500000000000002220 ) ) ;
#5003 = EDGE_LOOP ( 'NONE', ( #39447, #76144, #93489, #83106, #65818 ) ) ;
#5004 = CARTESIAN_POINT ( 'NONE',  ( -97.62287095715004170, -23.73907113216991505, -1.053371485793224371 ) ) ;
#5005 = DIRECTION ( 'NONE',  ( -0.000000000000000000, 1.000000000000000000, -0.000000000000000000 ) ) ;
#5006 = CARTESIAN_POINT ( 'NONE',  ( -51.62287095715004881, -24.50321055353805022, 9.387540953477534700 ) ) ;
#5007 = CARTESIAN_POINT ( 'NONE',  ( -53.55342350921662842, -23.96169478059712787, 10.65365249895718591 ) ) ;
#5009 = ORIENTED_EDGE ( 'NONE', *, *, #80073, .T. ) ;
#5008 = CARTESIAN_POINT ( 'NONE',  ( -6.767052838139933080, -20.26514109264706676, 11.49999999999999645 ) ) ;
#5010 = CARTESIAN_POINT ( 'NONE',  ( -62.62287095715004881, -29.50247984919015209, -1.443849546365056913 ) ) ;
#5011 = VECTOR ( 'NONE', #68536, 1000.000000000000000 ) ;
#5012 = VERTEX_POINT ( 'NONE', #88640 ) ;
#5013 = CARTESIAN_POINT ( 'NONE',  ( 11.91227609878784399, -18.80521639033699799, -1.500000000000002220 ) ) ;
#5014 = CARTESIAN_POINT ( 'NONE',  ( -10.41657757243416604, 17.86655067824183618, -1.500000000000002220 ) ) ;
#5015 = EDGE_CURVE ( 'NONE', #45647, #56694, #97242, .T. ) ;
#5016 = ORIENTED_EDGE ( 'NONE', *, *, #23171, .F. ) ;
#5017 = EDGE_CURVE ( 'NONE', #32090, #62563, #42969, .T. ) ;
#5018 = CARTESIAN_POINT ( 'NONE',  ( -28.48670877496179799, -24.18537698610731113, 0.1864216068622559508 ) ) ;
#5019 = ORIENTED_EDGE ( 'NONE', *, *, #94146, .T. ) ;
#5020 = CARTESIAN_POINT ( 'NONE',  ( -25.92875734969026169, -5.356774720514426491, 24.50402280011861933 ) ) ;
#5021 = ORIENTED_EDGE ( 'NONE', *, *, #23347, .F. ) ;
#5022 = CARTESIAN_POINT ( 'NONE',  ( -18.74228827200876779, -9.293929619069025705, -1.500000000000002220 ) ) ;
#5023 = CARTESIAN_POINT ( 'NONE',  ( -21.49438740719132923, 4.340694165963498996, 11.49999999999999645 ) ) ;
#5024 = EDGE_CURVE ( 'NONE', #89889, #29980, #56413, .T. ) ;
#5025 = CARTESIAN_POINT ( 'NONE',  ( -37.54584601135314159, -24.15620529776627379, 10.23563542870660825 ) ) ;
#5026 = CARTESIAN_POINT ( 'NONE',  ( -15.53634343318938704, 16.32316209468629253, -1.500000000000002220 ) ) ;
#5027 = CARTESIAN_POINT ( 'NONE',  ( 19.98859412959824411, 6.261702723725245612, 11.49999999999998934 ) ) ;
#5028 = ADVANCED_FACE ( 'NONE', ( #90128 ), #58682, .T. ) ;
#5029 = CARTESIAN_POINT ( 'NONE',  ( -106.6228709571500559, -23.47596703998600631, 11.44779298504227860 ) ) ;
#5030 = CARTESIAN_POINT ( 'NONE',  ( -119.5910506408271914, -23.96169478059714564, 10.65365249895717170 ) ) ;
#5031 = DIRECTION ( 'NONE',  ( 0.000000000000000000, -0.9999999999976377785, -2.173523156925979975E-06 ) ) ;
#5032 = ORIENTED_EDGE ( 'NONE', *, *, #41304, .F. ) ;
#5033 = EDGE_CURVE ( 'NONE', #3088, #46475, #36975, .T. ) ;
#5034 = ORIENTED_EDGE ( 'NONE', *, *, #3762, .T. ) ;
#5035 = ORIENTED_EDGE ( 'NONE', *, *, #83780, .F. ) ;
#5036 = LINE ( 'NONE', #52218, #14171 ) ;
#5037 = CARTESIAN_POINT ( 'NONE',  ( -11.48222599368078889, -18.13851731312990267, -1.500000000000002220 ) ) ;
#5038 = ADVANCED_FACE ( 'NONE', ( #34351 ), #37623, .T. ) ;
#5039 = CARTESIAN_POINT ( 'NONE',  ( -42.62287095715004881, -29.50247984919015209, -1.443849546365060466 ) ) ;
#5040 = ORIENTED_EDGE ( 'NONE', *, *, #38473, .F. ) ;
#5041 = CARTESIAN_POINT ( 'NONE',  ( 15.50021099394596646, 14.30638080151107694, -1.500000000000002220 ) ) ;
#5042 = CARTESIAN_POINT ( 'NONE',  ( -70.30743594849178635, -25.23380821724332534, 3.513009940249934182 ) ) ;
#5043 = DIRECTION ( 'NONE',  ( -1.000000000000000000, -0.000000000000000000, -0.000000000000000000 ) ) ;
#5044 = CARTESIAN_POINT ( 'NONE',  ( -50.60039650190779525, -24.15602025860895452, 10.28564288303536856 ) ) ;
#5045 = CARTESIAN_POINT ( 'NONE',  ( 9.016989526679575206, 3.316774720514426900, -27.05137190084761301 ) ) ;
#5046 = CARTESIAN_POINT ( 'NONE',  ( -99.17216252687966005, -25.23367668196706504, 3.679805935859953081 ) ) ;
#5047 = CARTESIAN_POINT ( 'NONE',  ( -22.12685673520133989, -0.1325007643398395663, -1.500000000000002220 ) ) ;
#5048 = DIRECTION ( 'NONE',  ( 0.000000000000000000, 2.173523156925980399E-06, -0.9999999999976378895 ) ) ;
#5049 = B_SPLINE_CURVE_WITH_KNOTS ( 'NONE', 3,
 ( #16655, #1452, #8047, #38997 ),
 .UNSPECIFIED., .F., .F.,
 ( 4, 4 ),
 ( 0.000000000000000000, 0.001418231214350569244 ),
 .UNSPECIFIED. ) ;
#5050 = CARTESIAN_POINT ( 'NONE',  ( -56.52287095715009002, -23.72773821059536203, 11.05748984161097503 ) ) ;
#5051 = CARTESIAN_POINT ( 'NONE',  ( -41.86646858058957577, -25.31624481711344643, 4.347423942039069900 ) ) ;
#5052 = B_SPLINE_CURVE_WITH_KNOTS ( 'NONE', 3,
 ( #63867, #71462, #1950, #1449 ),
 .UNSPECIFIED., .F., .F.,
 ( 4, 4 ),
 ( 0.2789617571284340736, 0.2799625041691996552 ),
 .UNSPECIFIED. ) ;
#5053 = CARTESIAN_POINT ( 'NONE',  ( -100.5908750829490117, -24.40034930558990567, 0.3402023900116026844 ) ) ;
#5054 = B_SPLINE_CURVE_WITH_KNOTS ( 'NONE', 3,
 ( #60242, #68839, #59739, #5436, #84055, #14034, #5932, #36885 ),
 .UNSPECIFIED., .F., .F.,
 ( 4, 2, 2, 4 ),
 ( 6.384118678621298445E-06, 0.002007151183507261457, 0.003007534715921583376, 0.004007918248335905730 ),
 .UNSPECIFIED. ) ;
#5055 = CARTESIAN_POINT ( 'NONE',  ( 12.02608574658498597, -17.65016651952024063, 11.49999999999998934 ) ) ;
#5056 = CARTESIAN_POINT ( 'NONE',  ( -70.25323322593359876, -25.04378563015144010, 7.559868539947981247 ) ) ;
#5057 = DIRECTION ( 'NONE',  ( -3.773278334453079618E-23, 0.9999999999976377785, 2.173523156925979975E-06 ) ) ;
#5058 = AXIS2_PLACEMENT_3D ( 'NONE', #17680, #87697, #78559 ) ;
#5059 = FACE_OUTER_BOUND ( 'NONE', #27478, .T. ) ;
#5060 = CARTESIAN_POINT ( 'NONE',  ( -8.599999999999997868, 24.84999999999999787, 2.100000000000000089 ) ) ;
#5061 = CARTESIAN_POINT ( 'NONE',  ( 21.95517018727266390, 5.574673621280945568, -1.500000000000002220 ) ) ;
#5062 = EDGE_LOOP ( 'NONE', ( #28717, #23049, #49464, #40104 ) ) ;
#5063 = CARTESIAN_POINT ( 'NONE',  ( -109.9228709571500673, -23.47593901973090524, -1.443836447538996426 ) ) ;
#5064 = CARTESIAN_POINT ( 'NONE',  ( -69.62287095715005592, -23.47593901973091235, -1.443836447539006196 ) ) ;
#5065 = CARTESIAN_POINT ( 'NONE',  ( -17.00503767097633556, -9.977476526402845991, 11.49999999999999645 ) ) ;
#5066 = DIRECTION ( 'NONE',  ( -0.9952638024365005887, -0.000000000000000000, -0.09721092304694052555 ) ) ;
#5067 = CARTESIAN_POINT ( 'NONE',  ( -59.62287095715007723, -23.47596703998600276, 11.44779298504227683 ) ) ;
#5068 = ORIENTED_EDGE ( 'NONE', *, *, #14290, .T. ) ;
#5069 = CARTESIAN_POINT ( 'NONE',  ( 14.85605547803280402, -2.682774720514425670, -27.37236044627089271 ) ) ;
#5070 = CARTESIAN_POINT ( 'NONE',  ( -0.3244794670026781014, -9.612687562450236811, -9.000000000000000000 ) ) ;
#5071 = PLANE ( 'NONE',  #83853 ) ;
#5072 = CARTESIAN_POINT ( 'NONE',  ( 11.61936018155104833, -18.21891831228114356, -1.500000000000002220 ) ) ;
#5073 = CARTESIAN_POINT ( 'NONE',  ( -27.38110673051268762, -24.78324009960318364, 7.572115309721827003 ) ) ;
#5074 = CARTESIAN_POINT ( 'NONE',  ( 8.665315094346039970, 17.34094453737590769, -1.500000000000002220 ) ) ;
#5075 = CARTESIAN_POINT ( 'NONE',  ( -10.22357262723052784, -3.975302591317960044, 29.38944064375215248 ) ) ;
#5076 = CARTESIAN_POINT ( 'NONE',  ( -80.51244414166535535, -25.04307398257883577, 7.563174194274490780 ) ) ;
#5077 = CARTESIAN_POINT ( 'NONE',  ( 19.60560811685724403, 2.727087469661350738, 11.49999999999998934 ) ) ;
#5078 = VECTOR ( 'NONE', #18547, 1000.000000000000000 ) ;
#5079 = VERTEX_POINT ( 'NONE', #66815 ) ;
#5080 = AXIS2_PLACEMENT_3D ( 'NONE', #10062, #18174, #17672 ) ;
#5081 = CARTESIAN_POINT ( 'NONE',  ( -20.27173212042777806, -0.06527795377243154895, 11.49999999999999645 ) ) ;
#5082 = CARTESIAN_POINT ( 'NONE',  ( -119.5228709571500758, -23.48786465467241769, 11.44779295918253759 ) ) ;
#5083 = CARTESIAN_POINT ( 'NONE',  ( 6.251785340501501587, -5.876774720514423400, 21.46941214867599612 ) ) ;
#5084 = ADVANCED_FACE ( 'NONE', ( #97736 ), #51573, .T. ) ;
#5085 = VERTEX_POINT ( 'NONE', #2914 ) ;
#5086 = DIRECTION ( 'NONE',  ( 1.000000000000000000, 0.000000000000000000, 0.000000000000000000 ) ) ;
#5087 = CARTESIAN_POINT ( 'NONE',  ( -88.52287095715006160, -23.48786465467241769, 11.44779295918254292 ) ) ;
#5088 = CARTESIAN_POINT ( 'NONE',  ( -44.62287095715007013, -24.34917612406837861, 0.1852690917426601802 ) ) ;
#5089 = EDGE_CURVE ( 'NONE', #57696, #14282, #38327, .T. ) ;
#5090 = LINE ( 'NONE', #52770, #81326 ) ;
#5091 = DIRECTION ( 'NONE',  ( -0.000000000000000000, 1.000000000000000000, 0.000000000000000000 ) ) ;
#5092 = CARTESIAN_POINT ( 'NONE',  ( 16.02535498940104830, 12.03463022438520191, -1.500000000000002220 ) ) ;
#5093 = EDGE_CURVE ( 'NONE', #94029, #18132, #13955, .T. ) ;
#5094 = DIRECTION ( 'NONE',  ( 0.7512896232465891000, 0.000000000000000000, 0.6599726524652351767 ) ) ;
#5095 = ORIENTED_EDGE ( 'NONE', *, *, #74807, .T. ) ;
#5096 = EDGE_CURVE ( 'NONE', #42079, #42444, #43208, .T. ) ;
#5097 = EDGE_CURVE ( 'NONE', #44273, #17897, #49665, .T. ) ;
#5098 = CARTESIAN_POINT ( 'NONE',  ( 22.02124265030973760, -4.543225279485573864, 16.20402280011862217 ) ) ;
#5099 = DIRECTION ( 'NONE',  ( -3.773278334453079618E-23, 0.9999999999976377785, 2.173523156925978705E-06 ) ) ;
#5100 = CARTESIAN_POINT ( 'NONE',  ( -67.52287095715006160, -23.48786465467241769, 11.44779295918254647 ) ) ;
#5101 = EDGE_CURVE ( 'NONE', #5695, #5245, #18819, .T. ) ;
#5102 = DIRECTION ( 'NONE',  ( -1.000000000000000000, -3.773278334444167608E-23, -8.201307833595939069E-29 ) ) ;
#5103 = PLANE ( 'NONE',  #62467 ) ;
#5104 = AXIS2_PLACEMENT_3D ( 'NONE', #41875, #33240, #72819 ) ;
#5105 = CARTESIAN_POINT ( 'NONE',  ( -14.11974515630795501, -17.41659395067913962, 11.49999999999999645 ) ) ;
#5106 = CARTESIAN_POINT ( 'NONE',  ( -49.26475614252912294, -25.23256535379771037, 6.480020017899467355 ) ) ;
#5107 = VERTEX_POINT ( 'NONE', #74887 ) ;
#5108 = CARTESIAN_POINT ( 'NONE',  ( 18.28078834835902455, 8.925752885971231620, 11.49999999999998934 ) ) ;
#5109 = ORIENTED_EDGE ( 'NONE', *, *, #81874, .T. ) ;
#5110 = EDGE_CURVE ( 'NONE', #39996, #100298, #91612, .T. ) ;
#5111 = CARTESIAN_POINT ( 'NONE',  ( -6.529369910325518944, -22.02198592821369516, 11.49999999999998934 ) ) ;
#5112 = CARTESIAN_POINT ( 'NONE',  ( -11.16000000000000014, -10.15233964170348457, 0.003711184059992174607 ) ) ;
#5113 = ORIENTED_EDGE ( 'NONE', *, *, #96784, .T. ) ;
#5114 = DIRECTION ( 'NONE',  ( -0.000000000000000000, -1.000000000000000000, -0.000000000000000000 ) ) ;
#5115 = CARTESIAN_POINT ( 'NONE',  ( 32.45853543194704116, 5.965225279485572685, 9.169203677920338080 ) ) ;
#5116 = ADVANCED_FACE ( 'NONE', ( #5390 ), #68791, .F. ) ;
#5117 = CARTESIAN_POINT ( 'NONE',  ( -38.62287095715005592, -24.66019654487199020, 8.947790411086137041 ) ) ;
#5119 = ORIENTED_EDGE ( 'NONE', *, *, #44571, .F. ) ;
#5118 = CARTESIAN_POINT ( 'NONE',  ( -21.08002519818654363, -2.465602145356518893, 11.49999999999999645 ) ) ;
#5120 = B_SPLINE_CURVE_WITH_KNOTS ( 'NONE', 3,
 ( #24965, #33088, #49330, #47815, #39188, #1140 ),
 .UNSPECIFIED., .F., .F.,
 ( 4, 2, 4 ),
 ( 1.570755371634111329E-05, 0.001396183895866087103, 0.002776660238015833410 ),
 .UNSPECIFIED. ) ;
#5121 = VERTEX_POINT ( 'NONE', #22092 ) ;
#5122 = CARTESIAN_POINT ( 'NONE',  ( -14.74362065938029076, 16.57599527146691898, -1.500000000000002220 ) ) ;
#5123 = VECTOR ( 'NONE', #41404, 1000.000000000000000 ) ;
#5124 = CARTESIAN_POINT ( 'NONE',  ( 10.47388184937329214, 17.72644800832989986, 11.49999999999998934 ) ) ;
#5125 = ORIENTED_EDGE ( 'NONE', *, *, #74861, .T. ) ;
#5126 = VERTEX_POINT ( 'NONE', #67808 ) ;
#5127 = CARTESIAN_POINT ( 'NONE',  ( 5.184553252003285984, 5.965225279485572685, -28.06387035751381731 ) ) ;
#5128 = CARTESIAN_POINT ( 'NONE',  ( -82.62287095715005592, -29.50248528299804818, 1.056150453629038477 ) ) ;
#5129 = ORIENTED_EDGE ( 'NONE', *, *, #84043, .T. ) ;
#5130 = ORIENTED_EDGE ( 'NONE', *, *, #85027, .F. ) ;
#5131 = ORIENTED_EDGE ( 'NONE', *, *, #68220, .F. ) ;
#5132 = DIRECTION ( 'NONE',  ( -3.773278334444167608E-23, 1.000000000000000000, 0.000000000000000000 ) ) ;
#5133 = CARTESIAN_POINT ( 'NONE',  ( -28.57183748306234250, -23.32756358287736376, 11.44779300624184160 ) ) ;
#5134 = CARTESIAN_POINT ( 'NONE',  ( 30.53060340732035982, -1.682774720514426114, -1.272392034746785860 ) ) ;
#5135 = CARTESIAN_POINT ( 'NONE',  ( -12.26507114386991226, -16.75673120704366426, -1.500000000000002220 ) ) ;
#5136 = CARTESIAN_POINT ( 'NONE',  ( 15.29254711327534899, -15.47666941828629739, 11.49999999999999645 ) ) ;
#5137 = ORIENTED_EDGE ( 'NONE', *, *, #1504, .F. ) ;
#5138 = CARTESIAN_POINT ( 'NONE',  ( -100.6399447160575420, -25.18730714472780718, 3.310768607064317415 ) ) ;
#5139 = LOCAL_TIME ( 0, 54, 15.00000000000000000, #23667 ) ;
#5140 = CARTESIAN_POINT ( 'NONE',  ( -37.55620429048340014, -24.66019654487198665, 8.947790411086135265 ) ) ;
#5141 = FACE_OUTER_BOUND ( 'NONE', #45197, .T. ) ;
#5142 = CARTESIAN_POINT ( 'NONE',  ( -22.40390758644239710, -1.035154934579901820, -1.500000000000002220 ) ) ;
#5143 = EDGE_CURVE ( 'NONE', #82230, #13329, #10376, .T. ) ;
#5144 = LINE ( 'NONE', #36096, #93475 ) ;
#5145 = CARTESIAN_POINT ( 'NONE',  ( -65.59841495659875932, -24.15503026093916006, -0.2815557561904380446 ) ) ;
#5146 = ORIENTED_EDGE ( 'NONE', *, *, #41140, .F. ) ;
#5147 = CARTESIAN_POINT ( 'NONE',  ( -71.27031559404676386, -25.31598477088890320, 4.985721588723864173 ) ) ;
#5148 = VECTOR ( 'NONE', #75199, 1000.000000000000000 ) ;
#5149 = CARTESIAN_POINT ( 'NONE',  ( -95.52287095715006160, -24.99156044556203327, 7.747789690856173195 ) ) ;
#5150 = LOCAL_TIME ( 0, 54, 15.00000000000000000, #67855 ) ;
#5151 = VERTEX_POINT ( 'NONE', #76870 ) ;
#5152 = EDGE_LOOP ( 'NONE', ( #71179, #74921, #81521, #63344 ) ) ;
#5153 = EDGE_CURVE ( 'NONE', #78417, #60824, #69689, .T. ) ;
#5154 = CARTESIAN_POINT ( 'NONE',  ( -99.52318946800619415, -25.30202668977020863, 5.579290425899357864 ) ) ;
#5155 = EDGE_LOOP ( 'NONE', ( #9423, #27310, #68711, #72820 ) ) ;
#5156 = CARTESIAN_POINT ( 'NONE',  ( 4.979423480801214552, 20.69870207611912605, -1.500000000000002220 ) ) ;
#5157 = ORIENTED_EDGE ( 'NONE', *, *, #55762, .T. ) ;
#5158 = PLANE ( 'NONE',  #41485 ) ;
#5159 = CARTESIAN_POINT ( 'NONE',  ( 16.32745387341675780, -14.53119815553504068, -1.500000000000002220 ) ) ;
#5160 = DIRECTION ( 'NONE',  ( 0.000000000000000000, -2.173523156925979552E-06, 0.9999999999976378895 ) ) ;
#5161 = CARTESIAN_POINT ( 'NONE',  ( 13.52301212282245935, 18.22803923376396540, -1.500000000000002220 ) ) ;
#5162 = FACE_OUTER_BOUND ( 'NONE', #92728, .T. ) ;
#5163 = DIRECTION ( 'NONE',  ( 0.000000000000000000, 0.000000000000000000, -1.000000000000000000 ) ) ;
#5164 = CARTESIAN_POINT ( 'NONE',  ( -13.81295463269534096, 17.03802364079049525, -1.500000000000002220 ) ) ;
#5165 = CARTESIAN_POINT ( 'NONE',  ( -87.58567460725342357, -24.51314013834317151, 0.6176544820404251679 ) ) ;
#5166 = EDGE_LOOP ( 'NONE', ( #2813, #43689, #51577, #67542 ) ) ;
#5167 = CARTESIAN_POINT ( 'NONE',  ( 29.59852343658945983, -4.673870278164355518, 28.90818992718861224 ) ) ;
#5168 = CARTESIAN_POINT ( 'NONE',  ( -121.6228709571500417, -23.47593901973091235, -1.443836447538997536 ) ) ;
#5169 = EDGE_LOOP ( 'NONE', ( #44368, #96460, #91645, #20830 ) ) ;
#5170 = CARTESIAN_POINT ( 'NONE',  ( -84.51766182033699693, -23.73791477778912551, 11.05961554403170766 ) ) ;
#5171 = CARTESIAN_POINT ( 'NONE',  ( -41.62287095715007013, -24.51283580621364422, 0.6167428607019734832 ) ) ;
#5172 = CARTESIAN_POINT ( 'NONE',  ( -20.43740209601095614, -23.59208382403500437, 0.3010598746230517819 ) ) ;
#5173 = CARTESIAN_POINT ( 'NONE',  ( -18.64022381217131397, 10.26305532446727753, 11.49999999999998934 ) ) ;
#5174 = CARTESIAN_POINT ( 'NONE',  ( -98.50756231633036464, -24.66019654487200086, 8.947790411086115725 ) ) ;
#5175 = CARTESIAN_POINT ( 'NONE',  ( -26.55847933594999333, -24.75186106919953488, 2.904080373301505702 ) ) ;
#5176 = CARTESIAN_POINT ( 'NONE',  ( -75.62287095715005592, -29.50250786944525672, 11.44777988621623521 ) ) ;
#5177 = CARTESIAN_POINT ( 'NONE',  ( -33.62373644273809958, -24.65952944569304606, 1.056160979905695907 ) ) ;
#5178 = CIRCLE ( 'NONE', #45674, 3.570000000000003837 ) ;
#5179 = B_SPLINE_SURFACE_WITH_KNOTS ( 'NONE', 3, 1, ( 
 ( #24719, #32847 ),
 ( #93731, #54690 ),
 ( #1904, #63316 ),
 ( #72421, #70916 ),
 ( #71413, #39955 ),
 ( #17112, #31339 ),
 ( #48080, #55198 ),
 ( #10501, #40961 ),
 ( #32340, #17619 ),
 ( #63823, #64326 ),
 ( #86128, #94736 ),
 ( #8507, #93230 ),
 ( #23720, #16109 ),
 ( #1406, #94234 ),
 ( #79514, #79006 ),
 ( #9504, #55700 ),
 ( #47080, #95243 ),
 ( #56705, #16604 ),
 ( #39458, #2405 ),
 ( #77995, #70408 ),
 ( #894, #48591 ),
 ( #47581, #56201 ),
 ( #25730, #87127 ) ),
 .UNSPECIFIED., .F., .F., .F.,
 ( 4, 1, 1, 1, 1, 1, 1, 1, 1, 1, 1, 1, 1, 1, 1, 1, 1, 1, 1, 1, 4 ),
 ( 2, 2 ),
 ( 0.000000000000000000, 0.07330213563861354142, 0.1422863278392666464, 0.2062532954491644865, 0.2660167794074391745, 0.3216117904407559402, 0.3725324599732942055, 0.4194969815799879376, 0.4623979521337304721, 0.5028252778726873817, 0.5414888117388608757, 0.5790338027738967108, 0.6151434188814435267, 0.6502976044497242869, 0.6849123758493420588, 0.7187008999567505718, 0.7521889702416487689, 0.8172453813748596918, 0.8791167514140035832, 0.9396133806889377382, 1.000000000000000000 ),
 ( 0.000000000000000000, 1.000000000000000000 ),
 .UNSPECIFIED. ) ;
#5180 = CARTESIAN_POINT ( 'NONE',  ( -117.5222355272872221, -23.48786465467241769, 11.44779295918253581 ) ) ;
#5181 = ORIENTED_EDGE ( 'NONE', *, *, #40669, .F. ) ;
#5182 = CARTESIAN_POINT ( 'NONE',  ( 19.50827032651345405, -1.201405007418623994, 11.49999999999999645 ) ) ;
#5183 = CARTESIAN_POINT ( 'NONE',  ( 8.160000000000000142, 2.939152317953647106E-16, -2.399999999999999911 ) ) ;
#5184 = CARTESIAN_POINT ( 'NONE',  ( -68.58953762381672448, -24.64898659630367916, 1.056161002820382722 ) ) ;
#5185 = ORIENTED_EDGE ( 'NONE', *, *, #91117, .T. ) ;
#5186 = DIRECTION ( 'NONE',  ( 0.000000000000000000, 0.000000000000000000, -1.000000000000000000 ) ) ;
#5187 = CARTESIAN_POINT ( 'NONE',  ( -99.30277203926080176, -25.25095956454628521, 6.024134243369381636 ) ) ;
#5188 = CARTESIAN_POINT ( 'NONE',  ( -26.12253190299266237, -24.72833061199699500, 7.423757303530043927 ) ) ;
#5189 = CARTESIAN_POINT ( 'NONE',  ( -40.62287095715006302, -24.62285846362214414, 9.038163152653526211 ) ) ;
#5190 = CARTESIAN_POINT ( 'NONE',  ( -19.47062899137607772, 3.135797168518691169, 11.49999999999998934 ) ) ;
#5191 = ORIENTED_EDGE ( 'NONE', *, *, #72872, .F. ) ;
#5192 = AXIS2_PLACEMENT_3D ( 'NONE', #72122, #49792, #2611 ) ;
#5193 = LINE ( 'NONE', #13293, #296 ) ;
#5194 = CARTESIAN_POINT ( 'NONE',  ( 2.904244945035652670, -5.876774720514416295, 20.04207437776001299 ) ) ;
#5195 = B_SPLINE_CURVE_WITH_KNOTS ( 'NONE', 3,
 ( #48245, #24390, #64494, #93393 ),
 .UNSPECIFIED., .F., .F.,
 ( 4, 4 ),
 ( 0.000000000000000000, 1.000000000000000000 ),
 .UNSPECIFIED. ) ;
#5196 = EDGE_CURVE ( 'NONE', #51347, #80380, #25378, .T. ) ;
#5197 = APPROVAL_STATUS ( 'not_yet_approved' ) ;
#5198 = ORIENTED_EDGE ( 'NONE', *, *, #65771, .T. ) ;
#5199 = CARTESIAN_POINT ( 'NONE',  ( 4.967948717948723392, -6.376774720514415407, 20.00140224358974095 ) ) ;
#5200 = PLANE ( 'NONE',  #11784 ) ;
#5201 = CARTESIAN_POINT ( 'NONE',  ( -47.64621855144071105, -23.96119346886880663, -0.6495511937831951466 ) ) ;
#5202 = CARTESIAN_POINT ( 'NONE',  ( -118.5191058840536869, -24.15543982623907482, -0.2315651400026558782 ) ) ;
#5203 = CARTESIAN_POINT ( 'NONE',  ( -45.62287095715004881, -24.99156045073392463, 7.747789690856161648 ) ) ;
#5204 = EDGE_CURVE ( 'NONE', #642, #55321, #28520, .T. ) ;
#5205 = CARTESIAN_POINT ( 'NONE',  ( -99.62287095715008434, -24.51387760970723306, 9.387446482453400520 ) ) ;
#5206 = CARTESIAN_POINT ( 'NONE',  ( -107.5144731571734127, -24.34968618360934656, 0.1864209137778970737 ) ) ;
#5207 = CARTESIAN_POINT ( 'NONE',  ( -8.813339738934139689, -17.91118242276673911, -1.500000000000002220 ) ) ;
#5208 = EDGE_CURVE ( 'NONE', #896, #19866, #5519, .T. ) ;
#5209 = CARTESIAN_POINT ( 'NONE',  ( -71.52287095715006160, -23.47593901973090169, -1.443836447538996870 ) ) ;
#5211 = DIRECTION ( 'NONE',  ( -3.773278334453079030E-23, 0.9999999999976377785, 2.173523156925979128E-06 ) ) ;
#5210 = LOCAL_TIME ( 0, 54, 15.00000000000000000, #73363 ) ;
#5212 = ORIENTED_EDGE ( 'NONE', *, *, #52682, .T. ) ;
#5213 = CARTESIAN_POINT ( 'NONE',  ( -128.6228709571500417, -23.48786465467242479, 11.44779295918253403 ) ) ;
#5214 = CARTESIAN_POINT ( 'NONE',  ( 4.612744205187371271, -6.376774720514418959, 20.61169588237105188 ) ) ;
#5215 = EDGE_CURVE ( 'NONE', #46438, #67086, #55143, .T. ) ;
#5216 = VECTOR ( 'NONE', #32004, 1000.000000000000114 ) ;
#5217 = CC_DESIGN_APPROVAL ( #488, ( #68385 ) ) ;
#5218 = CARTESIAN_POINT ( 'NONE',  ( -80.64005565590667857, -24.15602025860896163, 10.28564288303536145 ) ) ;
#5219 = CARTESIAN_POINT ( 'NONE',  ( -49.62287095715007013, -24.35013146730203459, 9.818937971375108376 ) ) ;
#5220 = CARTESIAN_POINT ( 'NONE',  ( -81.49977361814643473, -24.65952944569304961, 1.056160979905703901 ) ) ;
#5221 = EDGE_CURVE ( 'NONE', #153, #32461, #17491, .T. ) ;
#5222 = CARTESIAN_POINT ( 'NONE',  ( 10.24059822343757808, -5.876774720514426953, 17.17691942396160698 ) ) ;
#5223 = CARTESIAN_POINT ( 'NONE',  ( -51.33061876479827390, -25.26280066856253015, 4.756068594975189079 ) ) ;
#5224 = VERTEX_POINT ( 'NONE', #93108 ) ;
#5225 = CARTESIAN_POINT ( 'NONE',  ( -37.62287095715006302, -24.50321055353804311, 9.387540953477531147 ) ) ;
#5226 = CARTESIAN_POINT ( 'NONE',  ( 6.132272708306365949, -5.876774720514423400, 21.80683391321003839 ) ) ;
#5227 = ORIENTED_EDGE ( 'NONE', *, *, #9170, .T. ) ;
#5228 = CARTESIAN_POINT ( 'NONE',  ( 10.87751022112437482, 17.06716278085755079, 11.49999999999998934 ) ) ;
#5229 = CARTESIAN_POINT ( 'NONE',  ( -43.58953762381671027, -23.48783264082477729, -1.443836473390071928 ) ) ;
#5230 = CARTESIAN_POINT ( 'NONE',  ( 13.74975846015576586, 6.475225279485573360, -27.72022515045486557 ) ) ;
#5231 = CARTESIAN_POINT ( 'NONE',  ( -109.6228709571500701, -23.72747288104441665, -1.053458166803660667 ) ) ;
#5232 = B_SPLINE_CURVE_WITH_KNOTS ( 'NONE', 3,
 ( #33288, #2866, #64275, #25681, #87589, #79966, #10452, #70360, #41415, #72371 ),
 .UNSPECIFIED., .F., .F.,
 ( 4, 2, 2, 2, 4 ),
 ( 8.673617379884034509E-19, 0.0001781668809738670191, 0.0003563337619477331708, 0.0007126675238954626552, 0.001425335047790923793 ),
 .UNSPECIFIED. ) ;
#5233 = ORIENTED_EDGE ( 'NONE', *, *, #82139, .F. ) ;
#5234 = CARTESIAN_POINT ( 'NONE',  ( -80.16754667335695217, -25.30573843112062349, 4.512742708063584907 ) ) ;
#5235 = CARTESIAN_POINT ( 'NONE',  ( -2.104002878010082789, -5.876774720514409189, 19.15289935703627222 ) ) ;
#5236 = CARTESIAN_POINT ( 'NONE',  ( -11.36185547594953249, 16.55520930037988592, -1.500000000000002220 ) ) ;
#5237 = CARTESIAN_POINT ( 'NONE',  ( 20.56459456670464547, 4.482388377596099538, 11.49999999999999645 ) ) ;
#5238 = CARTESIAN_POINT ( 'NONE',  ( -28.04258906917542404, -24.84821647549576795, 7.555446715630902865 ) ) ;
#5239 = CARTESIAN_POINT ( 'NONE',  ( -70.49291431472521197, -24.73531770709095312, 8.716586749053510275 ) ) ;
#5240 = CARTESIAN_POINT ( 'NONE',  ( -19.65368394218270254, -10.04821906498216499, -1.500000000000002220 ) ) ;
#5241 = FACE_OUTER_BOUND ( 'NONE', #57390, .T. ) ;
#5242 = AXIS2_PLACEMENT_3D ( 'NONE', #38361, #46480, #16016 ) ;
#5243 = DIRECTION ( 'NONE',  ( 0.000000000000000000, 0.000000000000000000, 1.000000000000000000 ) ) ;
#5244 = CARTESIAN_POINT ( 'NONE',  ( -64.62287095715007013, -23.47596703998600631, 11.44779298504227683 ) ) ;
#5245 = VERTEX_POINT ( 'NONE', #32210 ) ;
#5246 = CARTESIAN_POINT ( 'NONE',  ( -100.0333332052708926, -25.13022549009045292, 2.886596846642130565 ) ) ;
#5247 = CARTESIAN_POINT ( 'NONE',  ( -31.58668462884854478, -24.34968618360933590, 0.1864209137778850556 ) ) ;
#5248 = ORIENTED_EDGE ( 'NONE', *, *, #90467, .F. ) ;
#5249 = EDGE_LOOP ( 'NONE', ( #34872, #41207, #93473, #65946 ) ) ;
#5250 = PLANE ( 'NONE',  #25931 ) ;
#5251 = DIRECTION ( 'NONE',  ( -1.000000000000000000, -3.773278334444167608E-23, -8.201307837791369499E-29 ) ) ;
#5252 = CARTESIAN_POINT ( 'NONE',  ( -76.63010910783911811, -24.34968618360934300, 0.1864209137778859160 ) ) ;
#5253 = CARTESIAN_POINT ( 'NONE',  ( -1.637206367458305500, 20.51943892441452633, -1.500000000000002220 ) ) ;
#5254 = CARTESIAN_POINT ( 'NONE',  ( 13.05104812959431548, -17.15854754814989391, 11.49999999999999645 ) ) ;
#5255 = EDGE_LOOP ( 'NONE', ( #33093, #72521, #79588, #90524 ) ) ;
#5256 = CARTESIAN_POINT ( 'NONE',  ( -91.60160660209938044, -23.48783264082477018, -1.443836473390090802 ) ) ;
#5257 = CARTESIAN_POINT ( 'NONE',  ( -56.62287095715004881, -24.66019654487199020, 8.947790411086131712 ) ) ;
#5258 = CARTESIAN_POINT ( 'NONE',  ( -129.6228709571500417, -24.65952944569305316, 1.056160979905706121 ) ) ;
#5259 = CARTESIAN_POINT ( 'NONE',  ( 3.003370282714790562, 22.13870467353671856, -1.500000000000002220 ) ) ;
#5260 = CARTESIAN_POINT ( 'NONE',  ( -79.68206046389329344, -25.27875020210991863, 6.776761220936831087 ) ) ;
#5261 = CARTESIAN_POINT ( 'NONE',  ( -61.55620429048339304, -24.64898659630528854, 1.056161002820821260 ) ) ;
#5262 = ORIENTED_EDGE ( 'NONE', *, *, #82532, .F. ) ;
#5263 = DIRECTION ( 'NONE',  ( -0.7512896232465894331, 0.000000000000000000, -0.6599726524652348436 ) ) ;
#5264 = CARTESIAN_POINT ( 'NONE',  ( -59.62287095715004881, -29.50247984919015209, -1.443849546365056913 ) ) ;
#5265 = AXIS2_PLACEMENT_3D ( 'NONE', #19551, #42910, #1844 ) ;
#5266 = CARTESIAN_POINT ( 'NONE',  ( -17.14161228048114438, 11.91956482804130601, 11.49999999999998934 ) ) ;
#5267 = VERTEX_POINT ( 'NONE', #94108 ) ;
#5268 = ADVANCED_FACE ( 'NONE', ( #47450 ), #63697, .F. ) ;
#5270 = ORIENTED_EDGE ( 'NONE', *, *, #11720, .F. ) ;
#5269 = FACE_OUTER_BOUND ( 'NONE', #61727, .T. ) ;
#5271 = VERTEX_POINT ( 'NONE', #77376 ) ;
#5272 = CARTESIAN_POINT ( 'NONE',  ( -100.6244603630846512, -24.92592662359561118, 8.075495903017998245 ) ) ;
#5273 = CARTESIAN_POINT ( 'NONE',  ( -9.089321149825819290, -19.05894737874082168, -1.500000000000002220 ) ) ;
#5274 = EDGE_CURVE ( 'NONE', #71653, #4511, #89101, .T. ) ;
#5275 = ORIENTED_EDGE ( 'NONE', *, *, #26358, .T. ) ;
#5276 = CARTESIAN_POINT ( 'NONE',  ( -77.62287095715005592, -24.64898659630367916, 1.056161002820826145 ) ) ;
#5277 = CARTESIAN_POINT ( 'NONE',  ( -2.899999999999996803, 31.80000000000000071, 0.000000000000000000 ) ) ;
#5278 = LINE ( 'NONE', #35742, #49745 ) ;
#5279 = CARTESIAN_POINT ( 'NONE',  ( -76.58805659134553423, -24.35071581493543036, 9.817618358456028815 ) ) ;
#5280 = CARTESIAN_POINT ( 'NONE',  ( -89.52287095715006160, -29.50247984919015209, -1.443849546365051806 ) ) ;
#5281 = CARTESIAN_POINT ( 'NONE',  ( -19.00758693998263738, -10.61793046214600089, -1.500000000000002220 ) ) ;
#5282 = CARTESIAN_POINT ( 'NONE',  ( 9.315600972258339496, -6.376774720514426953, 28.35070303307545458 ) ) ;
#5284 = VERTEX_POINT ( 'NONE', #56070 ) ;
#5283 = CARTESIAN_POINT ( 'NONE',  ( -0.5504121640580519337, 22.28327991085032878, 11.49999999999999645 ) ) ;
#5285 = CARTESIAN_POINT ( 'NONE',  ( -57.52287095715004739, -23.96177878511308634, 10.65340807706330217 ) ) ;
#5286 = FACE_OUTER_BOUND ( 'NONE', #77334, .T. ) ;
#5287 = CARTESIAN_POINT ( 'NONE',  ( -31.58953762381672803, -24.64898659630367206, 1.056161002820377393 ) ) ;
#5288 = EDGE_LOOP ( 'NONE', ( #35843, #64085, #56963, #83818 ) ) ;
#5289 = ORIENTED_EDGE ( 'NONE', *, *, #3322, .T. ) ;
#5290 = VECTOR ( 'NONE', #89316, 1000.000000000000000 ) ;
#5291 = ORIENTED_EDGE ( 'NONE', *, *, #44620, .F. ) ;
#5292 = CC_DESIGN_APPROVAL ( #56877, ( #94066 ) ) ;
#5293 = CARTESIAN_POINT ( 'NONE',  ( 9.071512145086499501, -0.9000000000000000222, 3.687490859131163923 ) ) ;
#5294 = DIRECTION ( 'NONE',  ( -0.000000000000000000, 2.173523156925979552E-06, -0.9999999999976378895 ) ) ;
#5295 = CARTESIAN_POINT ( 'NONE',  ( 30.64109437917162637, -3.603390417177663174, 28.31981403122773955 ) ) ;
#5296 = B_SPLINE_CURVE_WITH_KNOTS ( 'NONE', 3,
 ( #54215, #27986, #61823, #36097, #97976, #59440 ),
 .UNSPECIFIED., .F., .F.,
 ( 4, 2, 4 ),
 ( 6.391158118972359742E-06, 0.001387004593080792651, 0.002767618028042612838 ),
 .UNSPECIFIED. ) ;
#5297 = DIRECTION ( 'NONE',  ( -3.773278334453079030E-23, 0.9999999999976377785, 2.173523156925979128E-06 ) ) ;
#5298 = CARTESIAN_POINT ( 'NONE',  ( -19.23900614489824079, 2.250179475969715348, -1.500000000000002220 ) ) ;
#5299 = LINE ( 'NONE', #58595, #21444 ) ;
#5300 = EDGE_LOOP ( 'NONE', ( #28980, #59107, #16887, #25208 ) ) ;
#5301 = CARTESIAN_POINT ( 'NONE',  ( 12.39309347844599252, 14.90900669795185252, 11.49999999999999645 ) ) ;
#5302 = CARTESIAN_POINT ( 'NONE',  ( -69.52287095715009002, -23.72747288104470442, -1.053458166803227014 ) ) ;
#5303 = CIRCLE ( 'NONE', #15005, 0.3000000000000016542 ) ;
#5304 = ORIENTED_EDGE ( 'NONE', *, *, #86725, .F. ) ;
#5305 = CARTESIAN_POINT ( 'NONE',  ( 3.051095722660301934, -6.376774720514410077, 19.07493897947323092 ) ) ;
#5306 = CARTESIAN_POINT ( 'NONE',  ( -116.6228709571500559, -29.50248528299804818, 1.056150453629045360 ) ) ;
#5307 = CARTESIAN_POINT ( 'NONE',  ( 11.16000000000000014, -10.15233964170348457, 0.003711184059992174607 ) ) ;
#5308 = CARTESIAN_POINT ( 'NONE',  ( -87.62287095715004170, -24.64965695001468404, 8.947790433994180503 ) ) ;
#5309 = CARTESIAN_POINT ( 'NONE',  ( 11.71876819965036809, 15.69520123712499249, 11.49999999999998934 ) ) ;
#5310 = B_SPLINE_SURFACE_WITH_KNOTS ( 'NONE', 3, 3, ( 
 ( #92517, #24507, #71197, #32122 ),
 ( #46352, #7785, #100107, #674 ),
 ( #16391, #15391, #62586, #46856 ),
 ( #53487, #7280, #63094, #53979 ),
 ( #84413, #85405, #32625, #69696 ),
 ( #93512, #62092, #63601, #47358 ),
 ( #84906, #78287, #31621, #94523 ) ),
 .UNSPECIFIED., .F., .F., .F.,
 ( 4, 3, 4 ),
 ( 4, 4 ),
 ( 0.0004766839783823226305, 0.1029713700210898170, 0.2054660560637973088 ),
 ( 0.3595854696482522206, 0.3607641062792684150 ),
 .UNSPECIFIED. ) ;
#5311 = CARTESIAN_POINT ( 'NONE',  ( -46.53515119466756289, -24.51314013834315020, 0.6176544820404062941 ) ) ;
#5312 = ORIENTED_EDGE ( 'NONE', *, *, #14124, .F. ) ;
#5313 = CARTESIAN_POINT ( 'NONE',  ( -19.35566633068252074, -9.524217769563914970, -1.500000000000002220 ) ) ;
#5314 = SPHERICAL_SURFACE ( 'NONE', #47992, 1.000000000000000000 ) ;
#5315 = CARTESIAN_POINT ( 'NONE',  ( -70.42265764498320380, -25.12219144110324720, 7.098707687581576664 ) ) ;
#5316 = CARTESIAN_POINT ( 'NONE',  ( -120.6228709571500417, -29.50249982740957577, 7.747779886224967605 ) ) ;
#5317 = CARTESIAN_POINT ( 'NONE',  ( -100.3381132846150052, -25.18439336221437941, 3.296131460420185011 ) ) ;
#5318 = CARTESIAN_POINT ( 'NONE',  ( -15.63304604236160067, -16.83380969201049382, -1.500000000000002220 ) ) ;
#5319 = VECTOR ( 'NONE', #8927, 1000.000000000000000 ) ;
#5320 = PERSON_AND_ORGANIZATION ( #70597, #27821 ) ;
#5321 = CARTESIAN_POINT ( 'NONE',  ( -11.16000000000000014, -10.15233964170348457, 0.003711184059992174607 ) ) ;
#5322 = CARTESIAN_POINT ( 'NONE',  ( -49.49801449864284564, -25.25249061358302782, 3.767456410489268936 ) ) ;
#5323 = CARTESIAN_POINT ( 'NONE',  ( -12.46103870137906711, 15.87156016069071462, 11.49999999999999645 ) ) ;
#5324 = CARTESIAN_POINT ( 'NONE',  ( -108.9585383990916796, -25.28814330945115785, 4.038060318331745613 ) ) ;
#5325 = CARTESIAN_POINT ( 'NONE',  ( -32.65887063574198379, -23.73791477778911485, 11.05961554403171299 ) ) ;
#5326 = PRODUCT ( 'Plastic Part 1', 'Plastic Part 1', '', ( #52878 ) ) ;
#5327 = ADVANCED_FACE ( 'NONE', ( #46447 ), #70786, .F. ) ;
#5328 = CARTESIAN_POINT ( 'NONE',  ( -4.358143420448500116, -5.876774720514413630, 19.75705121608222115 ) ) ;
#5329 = DIRECTION ( 'NONE',  ( -1.000000000000000000, 0.000000000000000000, -0.000000000000000000 ) ) ;
#5330 = LINE ( 'NONE', #37284, #18614 ) ;
#5331 = CARTESIAN_POINT ( 'NONE',  ( -7.150643268323968904, -18.52920452239153448, -1.500000000000002220 ) ) ;
#5332 = VECTOR ( 'NONE', #17495, 1000.000000000000000 ) ;
#5333 = EDGE_CURVE ( 'NONE', #94842, #70772, #45429, .T. ) ;
#5334 = CARTESIAN_POINT ( 'NONE',  ( -113.5554278171332925, -23.96119346886881019, -0.6495511937832028071 ) ) ;
#5335 = CARTESIAN_POINT ( 'NONE',  ( 18.95923836289803788, 5.684714004613049987, -1.500000000000002220 ) ) ;
#5336 = CARTESIAN_POINT ( 'NONE',  ( -126.6239566813304975, -24.35071581493544457, 9.817618358456011052 ) ) ;
#5337 = ADVANCED_FACE ( 'NONE', ( #31212 ), #23588, .T. ) ;
#5338 = B_SPLINE_CURVE_WITH_KNOTS ( 'NONE', 3,
 ( #12142, #50228, #33491, #41118, #66477, #3058 ),
 .UNSPECIFIED., .F., .F.,
 ( 4, 2, 4 ),
 ( 6.384118678608765745E-06, 0.001386860460828372383, 0.002767336802978136254 ),
 .UNSPECIFIED. ) ;
#5339 = AXIS2_PLACEMENT_3D ( 'NONE', #5442, #36394, #75437 ) ;
#5340 = EDGE_CURVE ( 'NONE', #43107, #65034, #33420, .T. ) ;
#5341 = DESIGN_CONTEXT ( 'detailed design', #2559, 'design' ) ;
#5342 = CARTESIAN_POINT ( 'NONE',  ( -51.29687923781917647, -29.50249166729307149, 3.993452963156916002 ) ) ;
#5343 = CARTESIAN_POINT ( 'NONE',  ( -1.438454482798693146, -6.376774720514410077, 19.55848054040323092 ) ) ;
#5344 = CARTESIAN_POINT ( 'NONE',  ( 18.27903665858761073, 9.701928907310005457, 11.49999999999999645 ) ) ;
#5345 = DIRECTION ( 'NONE',  ( -3.773278334453079618E-23, 0.9999999999976377785, 2.173523156925979975E-06 ) ) ;
#5346 = EDGE_CURVE ( 'NONE', #22875, #29959, #9375, .T. ) ;
#5347 = CARTESIAN_POINT ( 'NONE',  ( -127.5228709571500616, -29.50248528299804818, 1.056150453629047137 ) ) ;
#5348 = FACE_OUTER_BOUND ( 'NONE', #19014, .T. ) ;
#5349 = CARTESIAN_POINT ( 'NONE',  ( -0.4833002549469566644, -22.66139224067150337, 11.49999999999999645 ) ) ;
#5350 = VERTEX_POINT ( 'NONE', #96124 ) ;
#5351 = CARTESIAN_POINT ( 'NONE',  ( -67.52287095715004739, -23.94994826722565406, -0.6494450866342734718 ) ) ;
#5352 = CARTESIAN_POINT ( 'NONE',  ( -33.52287095715006160, -24.66019654487198665, 8.947790411086131712 ) ) ;
#5353 = EDGE_CURVE ( 'NONE', #54462, #31713, #19484, .T. ) ;
#5354 = CARTESIAN_POINT ( 'NONE',  ( -100.5228709571500616, -29.50250243563736774, 8.947779886222138046 ) ) ;
#5355 = CARTESIAN_POINT ( 'NONE',  ( 8.160000000000000142, 10.80195425911416507, -0.9450485415980990345 ) ) ;
#5356 = VERTEX_POINT ( 'NONE', #26107 ) ;
#5357 = EDGE_LOOP ( 'NONE', ( #57104, #54102, #29116, #69430 ) ) ;
#5358 = VECTOR ( 'NONE', #90438, 1000.000000000000000 ) ;
#5359 = CARTESIAN_POINT ( 'NONE',  ( -98.52287095715006160, -29.50248528299804818, 1.056150453629042030 ) ) ;
#5360 = CARTESIAN_POINT ( 'NONE',  ( -22.23020047961643186, 5.420056861400933457, 11.49999999999998934 ) ) ;
#5361 = CARTESIAN_POINT ( 'NONE',  ( -2.717543299849222826, 17.80004702990586196, -9.000000000000000000 ) ) ;
#5362 = CARTESIAN_POINT ( 'NONE',  ( 16.61904782137575154, -13.72857183568914685, -1.500000000000002220 ) ) ;
#5363 = DIRECTION ( 'NONE',  ( -3.773278334444166432E-23, 1.000000000000000000, 0.000000000000000000 ) ) ;
#5364 = CARTESIAN_POINT ( 'NONE',  ( -65.52287095715010423, -24.63287334234179937, 0.9662140553045344138 ) ) ;
#5365 = CC_DESIGN_APPROVAL ( #69216, ( #2120 ) ) ;
#5366 = CARTESIAN_POINT ( 'NONE',  ( -8.633696204196466439, -20.85254729778420923, 11.49999999999999645 ) ) ;
#5367 = ORIENTED_EDGE ( 'NONE', *, *, #47058, .F. ) ;
#5368 = DIRECTION ( 'NONE',  ( 1.000000000000000000, 3.773278334444167608E-23, 8.201307833595939069E-29 ) ) ;
#5369 = CARTESIAN_POINT ( 'NONE',  ( -6.321128248299066499, 21.05883132939252533, 11.49999999999998934 ) ) ;
#5370 = DIRECTION ( 'NONE',  ( 0.000000000000000000, 0.000000000000000000, 1.000000000000000000 ) ) ;
#5371 = PLANE ( 'NONE',  #78343 ) ;
#5372 = VECTOR ( 'NONE', #3733, 1000.000000000000000 ) ;
#5373 = ORIENTED_EDGE ( 'NONE', *, *, #91916, .T. ) ;
#5374 = CARTESIAN_POINT ( 'NONE',  ( -48.52204675041186732, -23.48786465467241058, 11.44779295918254824 ) ) ;
#5375 = CARTESIAN_POINT ( 'NONE',  ( -90.55814612579646905, -23.85049219812686871, 10.88485053497527844 ) ) ;
#5376 = VERTEX_POINT ( 'NONE', #74279 ) ;
#5377 = LINE ( 'NONE', #90609, #79315 ) ;
#5378 = VERTEX_POINT ( 'NONE', #96610 ) ;
#5379 = VECTOR ( 'NONE', #38987, 1000.000000000000114 ) ;
#5380 = VERTEX_POINT ( 'NONE', #58077 ) ;
#5381 = CARTESIAN_POINT ( 'NONE',  ( -0.02075734969026423599, -5.965225279485572685, -0.08597719988137648983 ) ) ;
#5382 = CARTESIAN_POINT ( 'NONE',  ( 30.58729439590577570, -4.540774720514427543, 26.14186284044645703 ) ) ;
#5383 = CYLINDRICAL_SURFACE ( 'NONE', #47108, 3.500000000000000000 ) ;
#5384 = CARTESIAN_POINT ( 'NONE',  ( -17.38880980700008294, 10.71821138944157603, -1.500000000000002220 ) ) ;
#5385 = VERTEX_POINT ( 'NONE', #28109 ) ;
#5386 = CARTESIAN_POINT ( 'NONE',  ( -2.492070857093962921, -5.876774720514407413, 19.17707164986947177 ) ) ;
#5387 = CARTESIAN_POINT ( 'NONE',  ( -115.6228709571500417, -24.82576562982393042, 8.398263435472966165 ) ) ;
#5388 = EDGE_CURVE ( 'NONE', #92355, #63898, #32115, .T. ) ;
#5389 = CARTESIAN_POINT ( 'NONE',  ( -105.5477505147810717, -24.83618233451451118, 1.606449574219534826 ) ) ;
#5390 = FACE_OUTER_BOUND ( 'NONE', #19136, .T. ) ;
#5391 = EDGE_LOOP ( 'NONE', ( #19516, #48825, #56348, #37953 ) ) ;
#5392 = FACE_OUTER_BOUND ( 'NONE', #6046, .T. ) ;
#5393 = CARTESIAN_POINT ( 'NONE',  ( -27.70544111104076990, -25.26248076824083100, 8.251825376808540113 ) ) ;
#5394 = CARTESIAN_POINT ( 'NONE',  ( 5.792680761630559338, -19.98616098212858105, -1.500000000000002220 ) ) ;
#5396 = EDGE_CURVE ( 'NONE', #24728, #153, #91412, .T. ) ;
#5395 = ORIENTED_EDGE ( 'NONE', *, *, #3781, .T. ) ;
#5397 = B_SPLINE_CURVE_WITH_KNOTS ( 'NONE', 3,
 ( #27760, #51600, #20138, #82046 ),
 .UNSPECIFIED., .F., .F.,
 ( 4, 4 ),
 ( 1.387778780781445521E-17, 0.0001000000000000028779 ),
 .UNSPECIFIED. ) ;
#5399 = ORIENTED_EDGE ( 'NONE', *, *, #89415, .T. ) ;
#5398 = LINE ( 'NONE', #26741, #23173 ) ;
#5400 = B_SPLINE_SURFACE_WITH_KNOTS ( 'NONE', 3, 1, ( 
 ( #13286, #21390 ),
 ( #12290, #43266 ),
 ( #58992, #5187 ),
 ( #13784, #36143 ),
 ( #44261, #75683 ),
 ( #36635, #34653 ),
 ( #4199, #11799 ),
 ( #58004, #88936 ),
 ( #42773, #19411 ),
 ( #73706, #37135 ),
 ( #16295, #85304 ),
 ( #84804, #68097 ),
 ( #15791, #76183 ),
 ( #70088, #45257 ),
 ( #7178, #571 ),
 ( #38127, #47258 ),
 ( #61488, #37633 ),
 ( #99019, #83806 ),
 ( #30520, #91915 ) ),
 .UNSPECIFIED., .F., .F., .F.,
 ( 4, 1, 1, 1, 1, 1, 1, 1, 1, 1, 1, 1, 1, 1, 1, 1, 4 ),
 ( 2, 2 ),
 ( 0.000000000000000000, 0.06690918560565620177, 0.1334854404229647851, 0.2010351165700799414, 0.2712343400187647857, 0.3428799841615815525, 0.4138361296100178666, 0.4859766219744184323, 0.5602295572555456848, 0.5998841807523912495, 0.6440548396425977984, 0.6918919315842514406, 0.7446875244737690691, 0.8014917751698753534, 0.8628576982200926171, 0.9293283793947423321, 1.000000000000000000 ),
 ( 0.000000000000000000, 1.000000000000000000 ),
 .UNSPECIFIED. ) ;
#5401 = LINE ( 'NONE', #6400, #85960 ) ;
#5402 = CARTESIAN_POINT ( 'NONE',  ( -129.5895789150353323, -24.66019654487200086, 8.947790411086113949 ) ) ;
#5403 = ORIENTED_EDGE ( 'NONE', *, *, #40864, .F. ) ;
#5404 = ORIENTED_EDGE ( 'NONE', *, *, #71191, .F. ) ;
#5405 = CARTESIAN_POINT ( 'NONE',  ( -29.62287095715005592, -24.42603767492987998, 0.6165372256073464730 ) ) ;
#5406 = CARTESIAN_POINT ( 'NONE',  ( 13.91401389203221406, 6.475225279485573360, 158.0376437107427137 ) ) ;
#5407 = LINE ( 'NONE', #67316, #95553 ) ;
#5408 = B_SPLINE_CURVE_WITH_KNOTS ( 'NONE', 3,
 ( #47354, #10289, #2193, #93509 ),
 .UNSPECIFIED., .F., .F.,
 ( 4, 4 ),
 ( 0.000000000000000000, 0.0001000000000000028915 ),
 .UNSPECIFIED. ) ;
#5409 = CARTESIAN_POINT ( 'NONE',  ( -74.62287095715005592, -24.64898659630367561, 1.056161002820824368 ) ) ;
#5411 = VERTEX_POINT ( 'NONE', #42359 ) ;
#5410 = CARTESIAN_POINT ( 'NONE',  ( -7.471142097702432316, -20.87072022463130239, 11.49999999999999645 ) ) ;
#5412 = LINE ( 'NONE', #52091, #54423 ) ;
#5413 = CARTESIAN_POINT ( 'NONE',  ( 22.57354875331468591, -1.174960877787051716, 11.49999999999998934 ) ) ;
#5415 = ORIENTED_EDGE ( 'NONE', *, *, #52219, .F. ) ;
#5414 = CARTESIAN_POINT ( 'NONE',  ( -115.5528638974274003, -24.52399227489127043, 9.353111116836528183 ) ) ;
#5416 = VECTOR ( 'NONE', #36411, 1000.000000000000000 ) ;
#5417 = ORIENTED_EDGE ( 'NONE', *, *, #64498, .F. ) ;
#5418 = CARTESIAN_POINT ( 'NONE',  ( -69.58953762381672448, -23.47593901973091235, -1.443836447539006196 ) ) ;
#5419 = APPROVAL ( #27672, 'UNSPECIFIED' ) ;
#5420 = CARTESIAN_POINT ( 'NONE',  ( -55.52287095715005449, -25.00158670708909270, 2.256160236439166411 ) ) ;
#5421 = ORIENTED_EDGE ( 'NONE', *, *, #22805, .F. ) ;
#5422 = DIRECTION ( 'NONE',  ( 0.000000000000000000, -0.9961946980917452121, 0.08715574274766166307 ) ) ;
#5423 = CARTESIAN_POINT ( 'NONE',  ( 11.91227609878784399, -18.80521639033699799, -1.500000000000002220 ) ) ;
#5424 = CARTESIAN_POINT ( 'NONE',  ( -50.34609605362255280, -25.13941496713000845, 7.561522378954885326 ) ) ;
#5425 = EDGE_LOOP ( 'NONE', ( #77297, #51376 ) ) ;
#5426 = CARTESIAN_POINT ( 'NONE',  ( -73.92287095715008149, -23.47596703998600276, 11.44779298504227860 ) ) ;
#5427 = PLANE ( 'NONE',  #36229 ) ;
#5428 = CARTESIAN_POINT ( 'NONE',  ( -87.52287095715006160, -23.48786465467241058, 11.44779295918254292 ) ) ;
#5429 = CARTESIAN_POINT ( 'NONE',  ( -103.5228709571500758, -23.47596703998600631, 11.44779298504228215 ) ) ;
#5430 = B_SPLINE_CURVE_WITH_KNOTS ( 'NONE', 3,
 ( #21900, #67615, #91930, #6693, #13298, #44275 ),
 .UNSPECIFIED., .F., .F.,
 ( 4, 2, 4 ),
 ( 1.570887131794638196E-05, 0.001396322306279760422, 0.002776935741241574537 ),
 .UNSPECIFIED. ) ;
#5431 = CARTESIAN_POINT ( 'NONE',  ( 13.10664265030973930, -5.965225279485574461, -28.18129937516157568 ) ) ;
#5432 = VECTOR ( 'NONE', #64612, 1000.000000000000000 ) ;
#5433 = CARTESIAN_POINT ( 'NONE',  ( 16.17817332762582794, -10.88531698672339942, 11.49999999999998934 ) ) ;
#5434 = CARTESIAN_POINT ( 'NONE',  ( -21.25412285906045895, 3.082840150875858054, 11.49999999999998934 ) ) ;
#5435 = CARTESIAN_POINT ( 'NONE',  ( -2.780940648273603433, -6.376774720514413630, 20.02088365235843881 ) ) ;
#5436 = CARTESIAN_POINT ( 'NONE',  ( -120.5228709571500190, -24.52232992886364471, 0.6492154411906051470 ) ) ;
#5437 = CARTESIAN_POINT ( 'NONE',  ( -97.62287095715005592, -29.50250786944525672, 11.44777988621623166 ) ) ;
#5438 = CARTESIAN_POINT ( 'NONE',  ( -2.657479817400386413, -22.66247145590962120, -1.500000000000002220 ) ) ;
#5439 = VECTOR ( 'NONE', #66863, 1000.000000000000000 ) ;
#5440 = PERSON_AND_ORGANIZATION_ROLE ( 'design_supplier' ) ;
#5441 = CARTESIAN_POINT ( 'NONE',  ( -96.50664446042894440, -24.66019654487199375, 8.947790411086115725 ) ) ;
#5442 = CARTESIAN_POINT ( 'NONE',  ( 29.80070917940689412, -6.376774720514426953, 27.39560796525321607 ) ) ;
#5443 = CARTESIAN_POINT ( 'NONE',  ( 15.91301918423788919, -12.03417825965012433, 11.49999999999999645 ) ) ;
#5444 = DIRECTION ( 'NONE',  ( 2.910297583984928910E-15, 1.000000000000000000, -3.056206645085457922E-15 ) ) ;
#5445 = AXIS2_PLACEMENT_3D ( 'NONE', #32011, #39118, #560 ) ;
#5446 = CARTESIAN_POINT ( 'NONE',  ( -74.60679680638413913, -23.48786465467241058, 11.44779295918254824 ) ) ;
#5447 = CARTESIAN_POINT ( 'NONE',  ( -43.62287095715004881, -23.47593901973091235, -1.443836447539011525 ) ) ;
#5448 = ADVANCED_FACE ( 'NONE', ( #64705 ), #3784, .T. ) ;
#5449 = EDGE_LOOP ( 'NONE', ( #13137, #38982, #72786, #84044 ) ) ;
#5450 = CARTESIAN_POINT ( 'NONE',  ( -83.52287095715007581, -24.51387760970724372, 9.387446482453407626 ) ) ;
#5451 = FACE_OUTER_BOUND ( 'NONE', #48159, .T. ) ;
#5452 = CARTESIAN_POINT ( 'NONE',  ( -18.02536786162489335, -12.12045427182966861, -1.500000000000002220 ) ) ;
#5453 = FACE_OUTER_BOUND ( 'NONE', #54802, .T. ) ;
#5454 = CARTESIAN_POINT ( 'NONE',  ( 19.09806219120973125, -4.162641619376711510, -1.500000000000002220 ) ) ;
#5455 = CARTESIAN_POINT ( 'NONE',  ( -99.55473692232246208, -25.18616201609388483, 6.774537685832302536 ) ) ;
#5456 = VERTEX_POINT ( 'NONE', #43341 ) ;
#5457 = CALENDAR_DATE ( 2026, 9, 10 ) ;
#5458 = EDGE_CURVE ( 'NONE', #5619, #49448, #34228, .T. ) ;
#5459 = CARTESIAN_POINT ( 'NONE',  ( -42.62287095715004881, -29.50250243563736774, 8.947779886222148704 ) ) ;
#5460 = DIRECTION ( 'NONE',  ( -1.000000000000000000, 0.000000000000000000, 0.000000000000000000 ) ) ;
#5461 = CARTESIAN_POINT ( 'NONE',  ( 7.908618202329199320, -18.92053725880622039, 11.49999999999999645 ) ) ;
#5462 = DIRECTION ( 'NONE',  ( -3.773278334453079618E-23, 0.9999999999976377785, 2.173523156925979975E-06 ) ) ;
#5463 = EDGE_CURVE ( 'NONE', #125, #56501, #75787, .T. ) ;
#5464 = DIRECTION ( 'NONE',  ( 1.743630241030147080E-15, -6.974520964120588319E-15, 1.000000000000000000 ) ) ;
#5465 = B_SPLINE_CURVE_WITH_KNOTS ( 'NONE', 3,
 ( #75075, #59880, #51761, #19297 ),
 .UNSPECIFIED., .F., .F.,
 ( 4, 4 ),
 ( 0.000000000000000000, 9.999999999998897304E-05 ),
 .UNSPECIFIED. ) ;
#5466 = ORIENTED_EDGE ( 'NONE', *, *, #87824, .F. ) ;
#5467 = CARTESIAN_POINT ( 'NONE',  ( -58.62287095715006302, -24.65952944569304250, 1.056160979905695463 ) ) ;
#5468 = CARTESIAN_POINT ( 'NONE',  ( -39.44774024104455634, -25.18431059086297452, 4.157780032001940462 ) ) ;
#5469 = CARTESIAN_POINT ( 'NONE',  ( -19.38764004357183168, 0.3587747205143967943, -21.62823517627351322 ) ) ;
#5470 = ADVANCED_FACE ( 'NONE', ( #88511 ), #34720, .F. ) ;
#5471 = FACE_OUTER_BOUND ( 'NONE', #62373, .T. ) ;
#5472 = VECTOR ( 'NONE', #96581, 1000.000000000000114 ) ;
#5473 = ORIENTED_EDGE ( 'NONE', *, *, #19138, .F. ) ;
#5474 = CARTESIAN_POINT ( 'NONE',  ( 15.29947330337543754, -6.475225279485573360, -27.16854002387008649 ) ) ;
#5475 = CARTESIAN_POINT ( 'NONE',  ( -16.13607370526515794, 16.44073208242836159, 11.49999999999999645 ) ) ;
#5476 = CARTESIAN_POINT ( 'NONE',  ( -21.69093436787670726, -6.948586514802197023, 11.49999999999998934 ) ) ;
#5477 = CARTESIAN_POINT ( 'NONE',  ( 3.448102555317568374, -6.376774720514424288, 21.39871091031772110 ) ) ;
#5478 = CIRCLE ( 'NONE', #2235, 2.399999999999999911 ) ;
#5479 = DIRECTION ( 'NONE',  ( -3.773278334453080206E-23, 0.9999999999976377785, 2.173523156925979552E-06 ) ) ;
#5480 = CARTESIAN_POINT ( 'NONE',  ( -28.98875734969026041, -5.965225279485572685, -0.08597719988137116076 ) ) ;
#5481 = DIRECTION ( 'NONE',  ( 0.000000000000000000, 0.9999999999976377785, 2.173523156925979975E-06 ) ) ;
#5482 = CARTESIAN_POINT ( 'NONE',  ( -110.6248244526476014, -24.83618233451450763, 1.606449574219537935 ) ) ;
#5483 = CARTESIAN_POINT ( 'NONE',  ( 6.492371748702247203, -20.92784845389783399, 11.49999999999998934 ) ) ;
#5484 = DIRECTION ( 'NONE',  ( -3.773278334444167608E-23, 1.000000000000000000, 0.000000000000000000 ) ) ;
#5485 = PLANE ( 'NONE',  #50298 ) ;
#5486 = CARTESIAN_POINT ( 'NONE',  ( -65.05438548721848235, 3.316774720514426456, 27.45402280011862572 ) ) ;
#5487 = CARTESIAN_POINT ( 'NONE',  ( 2.499999999999995115, 19.99999999999999645, 2.100000000000000089 ) ) ;
#5488 = CARTESIAN_POINT ( 'NONE',  ( -58.49331616262661981, -24.51314013834315020, 0.6176544820404091807 ) ) ;
#5489 = VERTEX_POINT ( 'NONE', #81396 ) ;
#5490 = CARTESIAN_POINT ( 'NONE',  ( 19.37909195245082472, -6.530858791768283211, 11.49999999999998934 ) ) ;
#5491 = ORIENTED_EDGE ( 'NONE', *, *, #29005, .T. ) ;
#5492 = ORIENTED_EDGE ( 'NONE', *, *, #12278, .T. ) ;
#5493 = ORIENTED_EDGE ( 'NONE', *, *, #56837, .F. ) ;
#5494 = VERTEX_POINT ( 'NONE', #11876 ) ;
#5495 = EDGE_CURVE ( 'NONE', #44267, #64400, #73777, .T. ) ;
#5496 = CARTESIAN_POINT ( 'NONE',  ( 3.314627170985911420, 22.80399709308638023, 11.49999999999998934 ) ) ;
#5497 = CARTESIAN_POINT ( 'NONE',  ( -61.50935598288339889, -23.96119346886880308, -0.6495511937832122440 ) ) ;
#5498 = CARTESIAN_POINT ( 'NONE',  ( -19.95319933381289701, -3.276446921841525306, -1.500000000000002220 ) ) ;
#5499 = ORIENTED_EDGE ( 'NONE', *, *, #71438, .F. ) ;
#5500 = CARTESIAN_POINT ( 'NONE',  ( -122.5228709571500758, -23.47593901973090524, -1.443836447538996204 ) ) ;
#5501 = CARTESIAN_POINT ( 'NONE',  ( -101.5228709571500758, -23.47593901973090524, -1.443836447538996426 ) ) ;
#5502 = CARTESIAN_POINT ( 'NONE',  ( 10.86264265030973952, -5.965225279485574461, -28.64597719988137570 ) ) ;
#5503 = CARTESIAN_POINT ( 'NONE',  ( -99.58679885002307230, -24.51419770103158413, 9.386484678747175181 ) ) ;
#5505 = ORIENTED_EDGE ( 'NONE', *, *, #65886, .T. ) ;
#5504 = CARTESIAN_POINT ( 'NONE',  ( 17.37860173834871347, 12.56526366372364301, 11.49999999999999645 ) ) ;
#5506 = FACE_OUTER_BOUND ( 'NONE', #84119, .T. ) ;
#5507 = ORIENTED_EDGE ( 'NONE', *, *, #50403, .T. ) ;
#5508 = CARTESIAN_POINT ( 'NONE',  ( 4.478411676025833010, -20.21887007069289766, -1.500000000000002220 ) ) ;
#5509 = ORIENTED_EDGE ( 'NONE', *, *, #60776, .F. ) ;
#5510 = EDGE_CURVE ( 'NONE', #92347, #63576, #38227, .T. ) ;
#5511 = CARTESIAN_POINT ( 'NONE',  ( -29.52287095715006160, -24.57685061924431835, 8.947790457046968626 ) ) ;
#5512 = ORIENTED_EDGE ( 'NONE', *, *, #57691, .T. ) ;
#5513 = DIRECTION ( 'NONE',  ( -0.000000000000000000, 0.000000000000000000, 1.000000000000000000 ) ) ;
#5514 = VERTEX_POINT ( 'NONE', #35226 ) ;
#5515 = CARTESIAN_POINT ( 'NONE',  ( 13.87900837158347755, -15.70065903812341013, -1.500000000000002220 ) ) ;
#5516 = CARTESIAN_POINT ( 'NONE',  ( -6.887433846447126307, -20.85920400149894149, 11.49999999999999645 ) ) ;
#5517 = CARTESIAN_POINT ( 'NONE',  ( -81.52287095715006160, -23.48786465467241058, 11.44779295918254469 ) ) ;
#5518 = CARTESIAN_POINT ( 'NONE',  ( -8.307687032909205627, 20.95097986170506488, -1.500000000000002220 ) ) ;
#5519 = B_SPLINE_CURVE_WITH_KNOTS ( 'NONE', 3,
 ( #30719, #82998, #44462, #75386 ),
 .UNSPECIFIED., .F., .F.,
 ( 4, 4 ),
 ( 0.000000000000000000, 9.999999999999592548E-05 ),
 .UNSPECIFIED. ) ;
#5520 = CARTESIAN_POINT ( 'NONE',  ( -16.25153318171239647, -13.25006309444557751, 11.49999999999998934 ) ) ;
#5521 = CARTESIAN_POINT ( 'NONE',  ( 5.771117285127500551, -5.876774720514417183, 20.39900056875960388 ) ) ;
#5522 = CARTESIAN_POINT ( 'NONE',  ( -119.5202022874163532, -23.96169478059714564, 10.65365249895717170 ) ) ;
#5523 = CARTESIAN_POINT ( 'NONE',  ( 8.097539468418187170, -0.7382521156407183538, -3.736985260579223311 ) ) ;
#5524 = EDGE_LOOP ( 'NONE', ( #73891, #41738 ) ) ;
#5525 = ORIENTED_EDGE ( 'NONE', *, *, #25723, .F. ) ;
#5526 = ORIENTED_EDGE ( 'NONE', *, *, #18535, .T. ) ;
#5527 = CARTESIAN_POINT ( 'NONE',  ( -27.83739072329610664, 0.3587747205143967943, -8.084349702057700426 ) ) ;
#5528 = CIRCLE ( 'NONE', #33129, 0.2499999999997798983 ) ;
#5529 = ADVANCED_FACE ( 'NONE', ( #50953 ), #2725, .F. ) ;
#5530 = CARTESIAN_POINT ( 'NONE',  ( -20.95461191387366284, 4.708766595171775649, -1.500000000000002220 ) ) ;
#5531 = CARTESIAN_POINT ( 'NONE',  ( -105.5228709571500616, -24.62285846331440098, 9.038163153548232742 ) ) ;
#5532 = ORIENTED_EDGE ( 'NONE', *, *, #72612, .T. ) ;
#5533 = CARTESIAN_POINT ( 'NONE',  ( -20.67868931609407213, -4.308284118179648736, -1.500000000000002220 ) ) ;
#5534 = DIRECTION ( 'NONE',  ( -0.000000000000000000, 1.000000000000000000, -0.000000000000000000 ) ) ;
#5535 = CARTESIAN_POINT ( 'NONE',  ( -64.49197637527058191, -24.65952944569304250, 1.056160979905695685 ) ) ;
#5536 = ADVANCED_FACE ( 'NONE', ( #4770 ), #35169, .F. ) ;
#5537 = DIRECTION ( 'NONE',  ( 0.000000000000000000, 0.000000000000000000, 1.000000000000000000 ) ) ;
#5538 = FACE_OUTER_BOUND ( 'NONE', #8765, .T. ) ;
#5539 = CARTESIAN_POINT ( 'NONE',  ( -1.304987980769231948, -5.876774720514413630, 19.76512419871795245 ) ) ;
#5540 = CARTESIAN_POINT ( 'NONE',  ( 21.13397978930849064, -6.478279476769641221, -1.500000000000002220 ) ) ;
#5541 = DIRECTION ( 'NONE',  ( 0.000000000000000000, 0.000000000000000000, 1.000000000000000000 ) ) ;
#5542 = AXIS2_PLACEMENT_3D ( 'NONE', #88739, #98321, #96342 ) ;
#5543 = CARTESIAN_POINT ( 'NONE',  ( -3.085512303079157359, -6.376774720514415407, 19.95084900476495093 ) ) ;
#5544 = CARTESIAN_POINT ( 'NONE',  ( 12.17747153392518733, 4.565036639100802596, -27.62487831441275787 ) ) ;
#5545 = CARTESIAN_POINT ( 'NONE',  ( 19.75748517575715368, 5.965225279485572685, 28.87153971905864580 ) ) ;
#5546 = EDGE_CURVE ( 'NONE', #84539, #80523, #17994, .T. ) ;
#5547 = EDGE_CURVE ( 'NONE', #38515, #76664, #47952, .T. ) ;
#5548 = CARTESIAN_POINT ( 'NONE',  ( -58.62287095715004881, -23.47593901973091235, -1.443836447539007972 ) ) ;
#5549 = B_SPLINE_CURVE_WITH_KNOTS ( 'NONE', 3,
 ( #76015, #14622, #83126, #68421, #67932, #29349 ),
 .UNSPECIFIED., .F., .F.,
 ( 4, 2, 4 ),
 ( 6.391158118967745954E-06, 0.001387004593080788098, 0.002767618028042608501 ),
 .UNSPECIFIED. ) ;
#5550 = CIRCLE ( 'NONE', #53940, 10.11363636363636154 ) ;
#5551 = CARTESIAN_POINT ( 'NONE',  ( -9.780116039169133302, 16.78644576961053048, -1.500000000000002220 ) ) ;
#5552 = EDGE_CURVE ( 'NONE', #52365, #41503, #88012, .T. ) ;
#5553 = CARTESIAN_POINT ( 'NONE',  ( -19.64189229742525455, -8.423329616690555355, -1.500000000000002220 ) ) ;
#5554 = CARTESIAN_POINT ( 'NONE',  ( -26.09636659181000340, -24.96935267319560126, 4.940287552382958580 ) ) ;
#5555 = CARTESIAN_POINT ( 'NONE',  ( -66.62287095715008434, -24.33832256527048088, 0.1851278514138594566 ) ) ;
#5556 = CARTESIAN_POINT ( 'NONE',  ( -0.1426030150137709562, -21.20389190742572083, 11.50200000000000422 ) ) ;
#5557 = DIRECTION ( 'NONE',  ( 3.773278334444167608E-23, -1.000000000000000000, 0.000000000000000000 ) ) ;
#5558 = CARTESIAN_POINT ( 'NONE',  ( 6.494847429386178206, -21.66115869805930672, -1.500000000000002220 ) ) ;
#5559 = B_SPLINE_CURVE_WITH_KNOTS ( 'NONE', 3,
 ( #73898, #11493, #9996, #71914 ),
 .UNSPECIFIED., .F., .F.,
 ( 4, 4 ),
 ( 0.6609719839146940279, 0.6699784151868093396 ),
 .UNSPECIFIED. ) ;
#5560 = VERTEX_POINT ( 'NONE', #90004 ) ;
#5561 = CARTESIAN_POINT ( 'NONE',  ( -110.5228709571500758, -23.47593901973090524, -1.443836447538996204 ) ) ;
#5562 = CARTESIAN_POINT ( 'NONE',  ( 2.589743589743596086, -5.876774720514419847, 20.00140224358974095 ) ) ;
#5563 = CARTESIAN_POINT ( 'NONE',  ( 9.697495225759652726, 17.24774500829319734, 11.49999999999999645 ) ) ;
#5564 = CARTESIAN_POINT ( 'NONE',  ( -74.55620429048340725, -23.48783264082478439, -1.443836473390066821 ) ) ;
#5566 = B_SPLINE_CURVE_WITH_KNOTS ( 'NONE', 3,
 ( #89073, #33274, #42422, #34787 ),
 .UNSPECIFIED., .F., .F.,
 ( 4, 4 ),
 ( 0.3790364612049875181, 0.3800372082457528222 ),
 .UNSPECIFIED. ) ;
#5565 = CARTESIAN_POINT ( 'NONE',  ( -3.302878749216429544, 14.80319218833827044, 8.673617379884035472E-16 ) ) ;
#5567 = EDGE_CURVE ( 'NONE', #70921, #53265, #83877, .T. ) ;
#5568 = VERTEX_POINT ( 'NONE', #13361 ) ;
#5569 = CARTESIAN_POINT ( 'NONE',  ( -66.52287095715006160, -24.64898659630528854, 1.056161002820824368 ) ) ;
#5570 = CARTESIAN_POINT ( 'NONE',  ( -29.71166344112055668, -25.26026716537907291, 3.608440118052277157 ) ) ;
#5571 = FACE_OUTER_BOUND ( 'NONE', #77902, .T. ) ;
#5572 = CARTESIAN_POINT ( 'NONE',  ( 17.58597629297885589, -12.55149374826878272, -1.500000000000002220 ) ) ;
#5573 = CARTESIAN_POINT ( 'NONE',  ( -49.88732701573676565, -25.27517896348679827, 2.919594870841833334 ) ) ;
#5574 = CARTESIAN_POINT ( 'NONE',  ( -17.02366064725396555, -9.230830265533395362, -1.500000000000002220 ) ) ;
#5575 = CARTESIAN_POINT ( 'NONE',  ( -3.749999999999999556, 26.59999999999999432, 2.100000000000000089 ) ) ;
#5576 = DIRECTION ( 'NONE',  ( 0.000000000000000000, 0.000000000000000000, -1.000000000000000000 ) ) ;
#5577 = CARTESIAN_POINT ( 'NONE',  ( -15.51018552496569392, -12.33189742059753868, -1.500000000000002220 ) ) ;
#5578 = ORIENTED_EDGE ( 'NONE', *, *, #83070, .T. ) ;
#5579 = AXIS2_PLACEMENT_3D ( 'NONE', #4956, #64892, #80579 ) ;
#5580 = CARTESIAN_POINT ( 'NONE',  ( -3.904290608643684379, -19.93223805144805283, 11.49999999999999645 ) ) ;
#5581 = CARTESIAN_POINT ( 'NONE',  ( 8.868390920966309210, 6.053523946337313610, -26.43277665853620206 ) ) ;
#5582 = EDGE_CURVE ( 'NONE', #41241, #34495, #99850, .T. ) ;
#5583 = CARTESIAN_POINT ( 'NONE',  ( 33.64447732616053344, -3.738877066258443627, -11.77943383154337376 ) ) ;
#5584 = ADVANCED_FACE ( 'NONE', ( #14358 ), #60066, .T. ) ;
#5585 = ORIENTED_EDGE ( 'NONE', *, *, #88413, .T. ) ;
#5586 = B_SPLINE_SURFACE_WITH_KNOTS ( 'NONE', 3, 1, ( 
 ( #11847, #42818 ),
 ( #82356, #73749 ),
 ( #4248, #5235 ),
 ( #36192, #58536 ),
 ( #35197, #66169 ),
 ( #97087, #27586 ),
 ( #89477, #48698 ),
 ( #86734, #55306 ),
 ( #25336, #63426 ),
 ( #17222, #30056 ),
 ( #32959, #86237 ),
 ( #68139, #8617 ),
 ( #79621, #6723 ),
 ( #56314, #10113 ),
 ( #16719, #37677 ) ),
 .UNSPECIFIED., .F., .F., .F.,
 ( 4, 1, 1, 1, 1, 1, 1, 1, 1, 1, 1, 1, 4 ),
 ( 2, 2 ),
 ( 0.000000000000000000, 0.1183849129606691086, 0.2344384882140508886, 0.3525851839391771492, 0.4731673593536172007, 0.5350581108286732723, 0.5975237332646006205, 0.6605170696247792961, 0.7251603465314735431, 0.7908841475025376599, 0.8587744642336311296, 0.9282339358416605846, 1.000000000000000000 ),
 ( 0.000000000000000000, 1.000000000000000000 ),
 .UNSPECIFIED. ) ;
#5587 = CARTESIAN_POINT ( 'NONE',  ( -30.61333094834725088, -24.36247485673954571, 0.01136689895587403298 ) ) ;
#5588 = CARTESIAN_POINT ( 'NONE',  ( -85.62287095715004170, -29.50249982740957577, 7.747779886224967605 ) ) ;
#5589 = CARTESIAN_POINT ( 'NONE',  ( -71.52287095715003318, -23.73934037231756022, 11.05740245334328797 ) ) ;
#5590 = DIRECTION ( 'NONE',  ( 0.000000000000000000, 2.664535259100375697E-15, 1.000000000000000000 ) ) ;
#5591 = CARTESIAN_POINT ( 'NONE',  ( -31.52287095715006870, -23.95044443724991368, 10.65354141964649415 ) ) ;
#5592 = CARTESIAN_POINT ( 'NONE',  ( -2.827821146493835425, 19.88259668395040691, -1.500000000000002220 ) ) ;
#5593 = EDGE_CURVE ( 'NONE', #2529, #79651, #90498, .T. ) ;
#5594 = DIRECTION ( 'NONE',  ( 0.000000000000000000, -1.224646799147353207E-16, 1.000000000000000000 ) ) ;
#5595 = EDGE_LOOP ( 'NONE', ( #27226, #52542, #28497, #70797, #70436, #4677 ) ) ;
#5596 = EDGE_CURVE ( 'NONE', #63330, #79616, #21964, .T. ) ;
#5597 = EDGE_CURVE ( 'NONE', #30238, #34031, #58722, .T. ) ;
#5598 = CARTESIAN_POINT ( 'NONE',  ( -19.65108876255925807, -11.61119296138784662, 11.49999999999999645 ) ) ;
#5599 = CARTESIAN_POINT ( 'NONE',  ( -106.5228709571500900, -23.47593901973090524, -1.443836447538996204 ) ) ;
#5600 = LINE ( 'NONE', #20811, #28346 ) ;
#5601 = CARTESIAN_POINT ( 'NONE',  ( 29.68479148105952703, -1.682774720514426114, -9.431263391055123790 ) ) ;
#5602 = CARTESIAN_POINT ( 'NONE',  ( 6.110660513271839456, -5.876774720514422512, 21.43053473047838509 ) ) ;
#5603 = AXIS2_PLACEMENT_3D ( 'NONE', #76460, #6967, #37918 ) ;
#5604 = CARTESIAN_POINT ( 'NONE',  ( 5.271800844963591359, -6.376774720514426953, -28.56638892015329745 ) ) ;
#5605 = CARTESIAN_POINT ( 'NONE',  ( -3.561414601982806349, 22.15502443119318343, 11.49999999999999645 ) ) ;
#5606 = CARTESIAN_POINT ( 'NONE',  ( -50.78074163454362377, -25.29440776045720085, 5.833784451200526355 ) ) ;
#5607 = ORIENTED_EDGE ( 'NONE', *, *, #88374, .T. ) ;
#5608 = CARTESIAN_POINT ( 'NONE',  ( -16.75749313124890350, -11.57646860041911019, 11.49999999999998934 ) ) ;
#5609 = ORIENTED_EDGE ( 'NONE', *, *, #77398, .T. ) ;
#5610 = CARTESIAN_POINT ( 'NONE',  ( 17.95915693031428262, 14.28781372813260120, 11.49999999999998934 ) ) ;
#5611 = CARTESIAN_POINT ( 'NONE',  ( -10.54059822343757880, -5.876774720514426953, 23.12308057603841149 ) ) ;
#5612 = VECTOR ( 'NONE', #69900, 1000.000000000000114 ) ;
#5613 = VERTEX_POINT ( 'NONE', #29590 ) ;
#5614 = CARTESIAN_POINT ( 'NONE',  ( -20.27875734969026311, -4.543225279485573864, 25.15402280011862146 ) ) ;
#5615 = CARTESIAN_POINT ( 'NONE',  ( -77.56400409816168917, -23.48786465467240703, 11.44779295918254647 ) ) ;
#5616 = B_SPLINE_CURVE_WITH_KNOTS ( 'NONE', 3,
 ( #86045, #93647, #46488, #94658, #61729, #92648 ),
 .UNSPECIFIED., .F., .F.,
 ( 4, 2, 4 ),
 ( 0.000000000000000000, 0.001380901958385390062, 0.002761803916770780125 ),
 .UNSPECIFIED. ) ;
#5617 = CARTESIAN_POINT ( 'NONE',  ( -72.62287095715005592, -23.47593901973091235, -1.443836447539006196 ) ) ;
#5619 = VERTEX_POINT ( 'NONE', #52946 ) ;
#5618 = CARTESIAN_POINT ( 'NONE',  ( 19.37530031839547107, -8.734557088507903799, 11.49999999999999645 ) ) ;
#5620 = ORIENTED_EDGE ( 'NONE', *, *, #39501, .F. ) ;
#5621 = CARTESIAN_POINT ( 'NONE',  ( -7.477829544921322125, 20.88912457518834742, -1.500000000000002220 ) ) ;
#5622 = CARTESIAN_POINT ( 'NONE',  ( -9.109090448966927767, 18.51201596650851400, 11.49999999999998934 ) ) ;
#5623 = VERTEX_POINT ( 'NONE', #99583 ) ;
#5624 = VERTEX_POINT ( 'NONE', #45334 ) ;
#5625 = CARTESIAN_POINT ( 'NONE',  ( 30.93860345374796594, 6.475225279485573360, 20.86760796525322093 ) ) ;
#5626 = CARTESIAN_POINT ( 'NONE',  ( -39.81584396008233284, -25.14432053789888855, 2.967919351947699180 ) ) ;
#5627 = ORIENTED_EDGE ( 'NONE', *, *, #34312, .T. ) ;
#5628 = ORIENTED_EDGE ( 'NONE', *, *, #6224, .T. ) ;
#5629 = DIRECTION ( 'NONE',  ( 0.000000000000000000, -1.000000000000000000, 0.000000000000000000 ) ) ;
#5630 = CARTESIAN_POINT ( 'NONE',  ( -46.52287095715007581, -24.33832256527048088, 0.1851278514138610942 ) ) ;
#5631 = DIRECTION ( 'NONE',  ( -0.000000000000000000, -1.000000000000000000, -0.000000000000000000 ) ) ;
#5632 = CARTESIAN_POINT ( 'NONE',  ( 1.212613378922696050, -20.72488358683818888, -1.500000000000002220 ) ) ;
#5633 = CARTESIAN_POINT ( 'NONE',  ( 7.827691340095081607, 20.28360254610759839, 11.49999999999999645 ) ) ;
#5634 = ORIENTED_EDGE ( 'NONE', *, *, #98274, .F. ) ;
#5635 = CARTESIAN_POINT ( 'NONE',  ( -40.72474911149932097, -25.27806132187204469, 5.047107969529861293 ) ) ;
#5636 = CARTESIAN_POINT ( 'NONE',  ( -113.6228709571500985, -24.51387760970724727, 9.387446482453412955 ) ) ;
#5637 = CARTESIAN_POINT ( 'NONE',  ( -115.5183070177505869, -24.15503026093914940, -0.2815557561904543094 ) ) ;
#5638 = CARTESIAN_POINT ( 'NONE',  ( 14.18375884139645215, 17.39688726336347102, 11.49999999999998934 ) ) ;
#5639 = CARTESIAN_POINT ( 'NONE',  ( -50.80769758106637823, -25.31296745734188036, 4.647238349682671910 ) ) ;
#5640 = EDGE_LOOP ( 'NONE', ( #43228, #20314, #41991, #42658 ) ) ;
#5641 = LINE ( 'NONE', #13742, #85766 ) ;
#5642 = CARTESIAN_POINT ( 'NONE',  ( -69.52287095715007581, -24.50321055353803601, 9.387540953477520489 ) ) ;
#5643 = CIRCLE ( 'NONE', #67234, 1.399999999999998579 ) ;
#5644 = VERTEX_POINT ( 'NONE', #74765 ) ;
#5645 = ORIENTED_EDGE ( 'NONE', *, *, #77506, .T. ) ;
#5646 = CARTESIAN_POINT ( 'NONE',  ( -100.6814946224345846, -25.31401921878175898, 5.197788989978544549 ) ) ;
#5647 = ORIENTED_EDGE ( 'NONE', *, *, #2261, .F. ) ;
#5648 = EDGE_CURVE ( 'NONE', #99058, #75155, #98300, .T. ) ;
#5649 = CARTESIAN_POINT ( 'NONE',  ( 3.065528897535349628, -21.08962430476942274, -1.500000000000002220 ) ) ;
#5650 = VERTEX_POINT ( 'NONE', #44338 ) ;
#5651 = CARTESIAN_POINT ( 'NONE',  ( -26.33488822642538452, -24.88201932036028552, 6.524121876823151034 ) ) ;
#5652 = CARTESIAN_POINT ( 'NONE',  ( -20.11743356864677423, -6.099313207006018089, 11.49999999999998934 ) ) ;
#5653 = FACE_OUTER_BOUND ( 'NONE', #73296, .T. ) ;
#5654 = CARTESIAN_POINT ( 'NONE',  ( -6.316168294299441932, 21.79233575779346310, 11.49999999999998934 ) ) ;
#5655 = CARTESIAN_POINT ( 'NONE',  ( 15.00349586803797486, -3.316774720514427344, -27.42854230132123305 ) ) ;
#5656 = CARTESIAN_POINT ( 'NONE',  ( -29.22287096141859664, -23.36591977638094875, 11.44779298504228038 ) ) ;
#5657 = CARTESIAN_POINT ( 'NONE',  ( -14.06357901826416068, -16.81340526219955933, -1.500000000000002220 ) ) ;
#5658 = FACE_OUTER_BOUND ( 'NONE', #73987, .T. ) ;
#5659 = ORIENTED_EDGE ( 'NONE', *, *, #52191, .F. ) ;
#5660 = CARTESIAN_POINT ( 'NONE',  ( -122.5885208564929627, -24.66019654487200086, 8.947790411086113949 ) ) ;
#5661 = ADVANCED_FACE ( 'NONE', ( #28602 ), #36716, .T. ) ;
#5662 = ADVANCED_FACE ( 'NONE', ( #5760 ), #38464, .T. ) ;
#5663 = ORIENTED_EDGE ( 'NONE', *, *, #10316, .T. ) ;
#5664 = EDGE_CURVE ( 'NONE', #51748, #24998, #77745, .T. ) ;
#5665 = CARTESIAN_POINT ( 'NONE',  ( -120.5228709571500616, -24.99132157543167310, 2.256160258750667502 ) ) ;
#5666 = CARTESIAN_POINT ( 'NONE',  ( -41.62287095715008434, -24.34917612406837861, 0.1852690917426561001 ) ) ;
#5667 = ADVANCED_FACE ( 'NONE', ( #16361 ), #46829, .F. ) ;
#5668 = CARTESIAN_POINT ( 'NONE',  ( -10.29678027404481000, -22.20953590936370858, -0.9709657327914291702 ) ) ;
#5669 = CARTESIAN_POINT ( 'NONE',  ( 20.85495618715548716, -4.085033163991189653, 11.49999999999998934 ) ) ;
#5670 = CARTESIAN_POINT ( 'NONE',  ( -112.5526696820402464, -24.34968618360934656, 0.1864209137779000991 ) ) ;
#5671 = CARTESIAN_POINT ( 'NONE',  ( -26.71643515402310953, -24.75186064014422982, 2.706679525859190694 ) ) ;
#5672 = AXIS2_PLACEMENT_3D ( 'NONE', #87597, #47539, #1861 ) ;
#5673 = CARTESIAN_POINT ( 'NONE',  ( -85.59574030132286282, -24.15503026093914229, -0.2815557561904377115 ) ) ;
#5674 = CARTESIAN_POINT ( 'NONE',  ( -33.48943877366978938, -24.34968618360933235, 0.1864209137778845560 ) ) ;
#5675 = CARTESIAN_POINT ( 'NONE',  ( -79.62287095715005592, -24.33927499327854704, 9.819080762295817166 ) ) ;
#5676 = ORIENTED_EDGE ( 'NONE', *, *, #57042, .F. ) ;
#5677 = CARTESIAN_POINT ( 'NONE',  ( -3.832734262880480358, 19.25313627021017382, 11.49999999999999645 ) ) ;
#5678 = DIRECTION ( 'NONE',  ( -3.773278334453079618E-23, 0.9999999999976377785, 2.173523156925979975E-06 ) ) ;
#5679 = CARTESIAN_POINT ( 'NONE',  ( -119.5895376238167103, -23.47593901973091235, -1.443836447538997536 ) ) ;
#5680 = EDGE_CURVE ( 'NONE', #90732, #11989, #72034, .T. ) ;
#5681 = ORIENTED_EDGE ( 'NONE', *, *, #52529, .T. ) ;
#5682 = AXIS2_PLACEMENT_3D ( 'NONE', #75015, #27361, #58322 ) ;
#5683 = FACE_OUTER_BOUND ( 'NONE', #72027, .T. ) ;
#5684 = DIRECTION ( 'NONE',  ( 0.000000000000000000, -1.000000000000000000, 0.000000000000000000 ) ) ;
#5685 = VECTOR ( 'NONE', #6239, 1000.000000000000000 ) ;
#5686 = CARTESIAN_POINT ( 'NONE',  ( -27.33665423334501554, -24.63129246155760299, 8.218578399534145262 ) ) ;
#5687 = CARTESIAN_POINT ( 'NONE',  ( -45.62287095715004881, -24.99132157543083821, 2.256160258750667502 ) ) ;
#5689 = ADVANCED_FACE ( 'NONE', ( #93987 ), #24477, .F. ) ;
#5688 = CARTESIAN_POINT ( 'NONE',  ( -18.76583335001664565, 6.068782795689376286, 11.49999999999998934 ) ) ;
#5690 = VERTEX_POINT ( 'NONE', #2166 ) ;
#5691 = DIRECTION ( 'NONE',  ( 0.000000000000000000, -1.000000000000000000, 0.000000000000000000 ) ) ;
#5692 = PLANE ( 'NONE',  #41551 ) ;
#5693 = EDGE_CURVE ( 'NONE', #54115, #35328, #92981, .T. ) ;
#5694 = PERSON_AND_ORGANIZATION ( #70597, #27821 ) ;
#5695 = VERTEX_POINT ( 'NONE', #15356 ) ;
#5696 = LINE ( 'NONE', #21404, #87286 ) ;
#5697 = DIRECTION ( 'NONE',  ( -0.7863974287229266169, -5.639749025771352497E-15, 0.6177208787939496570 ) ) ;
#5698 = CARTESIAN_POINT ( 'NONE',  ( -47.53068546992037824, -24.65952944569304606, 1.056160979905696129 ) ) ;
#5699 = LINE ( 'NONE', #98535, #12049 ) ;
#5700 = DIRECTION ( 'NONE',  ( -0.6451914333552730696, 0.000000000000000000, -0.7640209514960754067 ) ) ;
#5701 = CARTESIAN_POINT ( 'NONE',  ( -70.15650799851037789, -25.31201593609383593, 5.327550971973213478 ) ) ;
#5702 = CARTESIAN_POINT ( 'NONE',  ( -112.5228709571500758, -24.50216790748205042, 0.6166512839542561686 ) ) ;
#5703 = CARTESIAN_POINT ( 'NONE',  ( 8.874027960929927517, 17.90919871486395465, -1.500000000000002220 ) ) ;
#5704 = EDGE_CURVE ( 'NONE', #89148, #44949, #74315, .T. ) ;
#5705 = CARTESIAN_POINT ( 'NONE',  ( -100.4381051993576506, -25.10935037667020708, 2.832404819440808907 ) ) ;
#5706 = CARTESIAN_POINT ( 'NONE',  ( -130.5728709571500588, -23.47596703998600631, 11.44779298504227860 ) ) ;
#5707 = ORIENTED_EDGE ( 'NONE', *, *, #11016, .T. ) ;
#5708 = CARTESIAN_POINT ( 'NONE',  ( -16.89397143409390623, -5.876774720514426953, 16.89397143409405899 ) ) ;
#5709 = DIRECTION ( 'NONE',  ( 1.000000000000000000, 3.491481338843133355E-15, 2.352173255807796056E-16 ) ) ;
#5710 = B_SPLINE_CURVE_WITH_KNOTS ( 'NONE', 3,
 ( #77853, #10233, #18842, #85477, #15464, #56930, #23570, #46928 ),
 .UNSPECIFIED., .F., .F.,
 ( 4, 2, 2, 4 ),
 ( 0.000000000000000000, 0.002001079623178225395, 0.003001619434767336357, 0.004002159246356447320 ),
 .UNSPECIFIED. ) ;
#5711 = EDGE_CURVE ( 'NONE', #79973, #96474, #54439, .T. ) ;
#5712 = CARTESIAN_POINT ( 'NONE',  ( -119.5178303131261686, -24.51314013834316086, 0.6176544820404233915 ) ) ;
#5713 = AXIS2_PLACEMENT_3D ( 'NONE', #69854, #48022, #40899 ) ;
#5714 = CARTESIAN_POINT ( 'NONE',  ( -80.63077793647542535, -24.63419186844610920, 9.035850630976915099 ) ) ;
#5715 = FACE_OUTER_BOUND ( 'NONE', #99330, .T. ) ;
#5716 = CARTESIAN_POINT ( 'NONE',  ( -81.50938704143565872, -24.15543982623907482, -0.2315651400026469686 ) ) ;
#5717 = EDGE_CURVE ( 'NONE', #13954, #52058, #39199, .T. ) ;
#5718 = LINE ( 'NONE', #60524, #7560 ) ;
#5719 = CARTESIAN_POINT ( 'NONE',  ( -51.61156992512332664, -25.26279989178249963, 4.398685687049794346 ) ) ;
#5720 = ORIENTED_EDGE ( 'NONE', *, *, #23048, .F. ) ;
#5721 = CARTESIAN_POINT ( 'NONE',  ( -34.62287095715004881, -23.48783264082478084, -1.443836473390074149 ) ) ;
#5722 = DIRECTION ( 'NONE',  ( 1.000000000000000000, 3.773278334444166432E-23, 8.201307841325785021E-29 ) ) ;
#5723 = ORIENTED_EDGE ( 'NONE', *, *, #78971, .T. ) ;
#5724 = CARTESIAN_POINT ( 'NONE',  ( -17.45352675615719917, 10.31968153043333380, 11.49999999999998934 ) ) ;
#5725 = CARTESIAN_POINT ( 'NONE',  ( -69.09926072775436978, -25.30615323796089911, 5.508687107256749371 ) ) ;
#5726 = DIRECTION ( 'NONE',  ( -3.773278334444167608E-23, 1.000000000000000000, 0.000000000000000000 ) ) ;
#5727 = CARTESIAN_POINT ( 'NONE',  ( -82.52287095715007581, -24.66019654487199730, 8.947790411086122830 ) ) ;
#5728 = ORIENTED_EDGE ( 'NONE', *, *, #79331, .F. ) ;
#5729 = DIRECTION ( 'NONE',  ( 1.000000000000000000, 3.773278334444167608E-23, 8.201307833595939069E-29 ) ) ;
#5730 = CARTESIAN_POINT ( 'NONE',  ( -52.52287095715007581, -23.73934037231757088, 11.05740245334329153 ) ) ;
#5731 = CARTESIAN_POINT ( 'NONE',  ( 11.77038589110637901, 16.27938679534767275, -1.500000000000002220 ) ) ;
#5732 = CARTESIAN_POINT ( 'NONE',  ( -2.639205680565387624, -20.84613592336672028, 11.49999999999999645 ) ) ;
#5733 = CARTESIAN_POINT ( 'NONE',  ( -28.74730064801421747, -24.99530720856141741, 7.079464916830322530 ) ) ;
#5734 = LINE ( 'NONE', #37186, #70872 ) ;
#5735 = CARTESIAN_POINT ( 'NONE',  ( 10.35204687333978057, 19.51823071965408829, -1.500000000000002220 ) ) ;
#5736 = VECTOR ( 'NONE', #87338, 1000.000000000000114 ) ;
#5737 = CARTESIAN_POINT ( 'NONE',  ( 18.57849760351508195, 8.651319581928444080, -1.500000000000002220 ) ) ;
#5738 = CARTESIAN_POINT ( 'NONE',  ( -39.44787993411948435, -25.27805918946292252, 4.218554851849822818 ) ) ;
#5739 = CIRCLE ( 'NONE', #41471, 252.4458649670781085 ) ;
#5740 = DIRECTION ( 'NONE',  ( 1.000000000000000000, 0.000000000000000000, 0.000000000000000000 ) ) ;
#5741 = PLANE ( 'NONE',  #71995 ) ;
#5742 = ORIENTED_EDGE ( 'NONE', *, *, #13121, .F. ) ;
#5743 = FACE_OUTER_BOUND ( 'NONE', #2363, .T. ) ;
#5744 = CARTESIAN_POINT ( 'NONE',  ( -72.55620429048340725, -24.64965694238574656, 8.947790433994198267 ) ) ;
#5745 = ORIENTED_EDGE ( 'NONE', *, *, #35402, .T. ) ;
#5746 = AXIS2_PLACEMENT_3D ( 'NONE', #34639, #42274, #51861 ) ;
#5747 = ORIENTED_EDGE ( 'NONE', *, *, #15829, .T. ) ;
#5748 = CARTESIAN_POINT ( 'NONE',  ( -55.52287095715009002, -24.15431212366389246, -0.2830839119429263695 ) ) ;
#5749 = DIRECTION ( 'NONE',  ( -1.000000000000000000, -0.000000000000000000, -0.000000000000000000 ) ) ;
#5750 = CARTESIAN_POINT ( 'NONE',  ( -76.50054984638063615, -24.51314013834316441, 0.6176544820404193947 ) ) ;
#5751 = CARTESIAN_POINT ( 'NONE',  ( -16.41017380093149214, -12.48182641202616416, -1.500000000000002220 ) ) ;
#5752 = VECTOR ( 'NONE', #21114, 1000.000000000000114 ) ;
#5753 = CARTESIAN_POINT ( 'NONE',  ( -11.74548148041400708, 18.04809798412036059, 11.49999999999999645 ) ) ;
#5754 = ORIENTED_EDGE ( 'NONE', *, *, #91820, .F. ) ;
#5755 = DIRECTION ( 'NONE',  ( 0.000000000000000000, -0.000000000000000000, -1.000000000000000000 ) ) ;
#5756 = CARTESIAN_POINT ( 'NONE',  ( -129.6228709571500133, -23.48783264082478794, -1.443836473390056607 ) ) ;
#5757 = CARTESIAN_POINT ( 'NONE',  ( 8.681249458320607459, -20.60847208623538762, 11.49999999999998934 ) ) ;
#5758 = AXIS2_PLACEMENT_3D ( 'NONE', #87249, #49713, #32975 ) ;
#5759 = CARTESIAN_POINT ( 'NONE',  ( -80.45048864170028935, -25.12205811578958148, 7.100580275183103751 ) ) ;
#5760 = FACE_OUTER_BOUND ( 'NONE', #38086, .T. ) ;
#5761 = ORIENTED_EDGE ( 'NONE', *, *, #2594, .F. ) ;
#5762 = CARTESIAN_POINT ( 'NONE',  ( 15.92621150404962016, -6.475225279485573360, -27.29681269571041824 ) ) ;
#5763 = CARTESIAN_POINT ( 'NONE',  ( -49.59948343357038425, -23.96169478059712432, 10.65365249895718414 ) ) ;
#5764 = CARTESIAN_POINT ( 'NONE',  ( 16.07097863352054290, 13.35096362007907622, -1.500000000000002220 ) ) ;
#5765 = EDGE_LOOP ( 'NONE', ( #68931, #14063, #81932, #83262 ) ) ;
#5767 = ORIENTED_EDGE ( 'NONE', *, *, #41579, .F. ) ;
#5766 = CARTESIAN_POINT ( 'NONE',  ( -67.59254650884999194, -24.15620529776628800, 10.23563542870660115 ) ) ;
#5768 = ORIENTED_EDGE ( 'NONE', *, *, #49672, .F. ) ;
#5769 = CARTESIAN_POINT ( 'NONE',  ( 8.160000000000000142, 0.000000000000000000, 2.399999999999999911 ) ) ;
#5770 = CARTESIAN_POINT ( 'NONE',  ( 1.363997202867437863, 21.09336101032836908, -1.500000000000002220 ) ) ;
#5771 = EDGE_LOOP ( 'NONE', ( #63225, #25539, #46611, #71942 ) ) ;
#5772 = DIRECTION ( 'NONE',  ( -1.654368437580061084E-16, 1.000000000000000000, 2.664535259100375697E-15 ) ) ;
#5774 = ADVANCED_FACE ( 'NONE', ( #94492 ), #47828, .T. ) ;
#5773 = DIRECTION ( 'NONE',  ( 1.000000000000000000, 0.000000000000000000, 0.000000000000000000 ) ) ;
#5775 = DIRECTION ( 'NONE',  ( 1.000000000000000000, 0.000000000000000000, 0.000000000000000000 ) ) ;
#5776 = EDGE_CURVE ( 'NONE', #59325, #97546, #31590, .T. ) ;
#5777 = CARTESIAN_POINT ( 'NONE',  ( -76.62667340351318046, -24.51419770103157347, 9.386484678747176957 ) ) ;
#5778 = CARTESIAN_POINT ( 'NONE',  ( 7.344278919687202922, -5.876774720514417183, 20.19896341048075783 ) ) ;
#5779 = CARTESIAN_POINT ( 'NONE',  ( -17.45706314325883213, 13.02611496694466275, -1.500000000000002220 ) ) ;
#5780 = CARTESIAN_POINT ( 'NONE',  ( -79.45432304757802910, -25.11735646291920077, 7.191156800755474698 ) ) ;
#5782 = VERTEX_POINT ( 'NONE', #55949 ) ;
#5781 = CARTESIAN_POINT ( 'NONE',  ( 16.98343680692684643, -14.46476453587665389, 11.49999999999999645 ) ) ;
#5783 = CARTESIAN_POINT ( 'NONE',  ( 31.99559323149412648, 3.570691370340881576, -11.82294999027247862 ) ) ;
#5784 = CARTESIAN_POINT ( 'NONE',  ( 23.50000000000000000, -0.9000000000000000222, 1.103411337323757735 ) ) ;
#5785 = DIRECTION ( 'NONE',  ( 0.000000000000000000, -2.173523156925980399E-06, 0.9999999999976378895 ) ) ;
#5786 = ORIENTED_EDGE ( 'NONE', *, *, #23619, .F. ) ;
#5787 = EDGE_CURVE ( 'NONE', #28152, #27902, #96055, .T. ) ;
#5788 = EDGE_CURVE ( 'NONE', #29452, #21016, #57437, .T. ) ;
#5789 = VERTEX_POINT ( 'NONE', #43224 ) ;
#5790 = VERTEX_POINT ( 'NONE', #80780 ) ;
#5791 = VECTOR ( 'NONE', #7835, 1000.000000000000114 ) ;
#5792 = CARTESIAN_POINT ( 'NONE',  ( -100.4426124108961176, -25.13313949306887451, 7.101635536975466678 ) ) ;
#5793 = B_SPLINE_CURVE_WITH_KNOTS ( 'NONE', 3,
 ( #22681, #62790, #38924, #84096 ),
 .UNSPECIFIED., .F., .F.,
 ( 4, 4 ),
 ( 1.387778780781445676E-17, 9.999999999997510880E-05 ),
 .UNSPECIFIED. ) ;
#5794 = DIRECTION ( 'NONE',  ( 3.491481338843133355E-15, -1.000000000000000000, 2.352173255807804438E-16 ) ) ;
#5795 = CARTESIAN_POINT ( 'NONE',  ( 30.60993360729056079, -4.065030569019225659, 27.12046991540520580 ) ) ;
#5796 = CARTESIAN_POINT ( 'NONE',  ( -67.58953762381672448, -23.48786465467241058, 11.44779295918254647 ) ) ;
#5797 = CARTESIAN_POINT ( 'NONE',  ( 2.021814659504407579E-13, -19.30000000000000426, 11.49999999999998934 ) ) ;
#5798 = EDGE_CURVE ( 'NONE', #59154, #36357, #93710, .T. ) ;
#5799 = DIRECTION ( 'NONE',  ( -3.773278334453079618E-23, 0.9999999999976377785, 2.173523156925979975E-06 ) ) ;
#5800 = ORIENTED_EDGE ( 'NONE', *, *, #57280, .F. ) ;
#5801 = CARTESIAN_POINT ( 'NONE',  ( -16.24122463664219396, 10.56255597858309869, 11.49999999999999645 ) ) ;
#5802 = DIRECTION ( 'NONE',  ( 0.000000000000000000, 0.9999999999976377785, 2.173523156925979128E-06 ) ) ;
#5803 = ORIENTED_EDGE ( 'NONE', *, *, #4430, .T. ) ;
#5804 = CARTESIAN_POINT ( 'NONE',  ( 3.787259615384621636, -5.876774720514404748, 18.51923076923076650 ) ) ;
#5805 = CARTESIAN_POINT ( 'NONE',  ( 3.797776442307698286, -6.376774720514401196, 18.16025641025640525 ) ) ;
#5806 = FACE_OUTER_BOUND ( 'NONE', #80995, .T. ) ;
#5807 = CARTESIAN_POINT ( 'NONE',  ( 26.73860345374794178, -5.161986642477099707, -6.453784975055922857 ) ) ;
#5808 = B_SPLINE_CURVE_WITH_KNOTS ( 'NONE', 3,
 ( #64141, #19431, #89449, #80334 ),
 .UNSPECIFIED., .F., .F.,
 ( 4, 4 ),
 ( 0.5408862336198214660, 0.5498926648919369997 ),
 .UNSPECIFIED. ) ;
#5809 = CARTESIAN_POINT ( 'NONE',  ( 13.00645856128228495, 14.71372164842801844, -1.500000000000002220 ) ) ;
#5810 = CARTESIAN_POINT ( 'NONE',  ( -46.62846617042131925, -24.51314013834315020, 0.6176544820404077374 ) ) ;
#5811 = ORIENTED_EDGE ( 'NONE', *, *, #18163, .F. ) ;
#5812 = CARTESIAN_POINT ( 'NONE',  ( 21.29926025483437257, -3.289820829717503337, -1.500000000000002220 ) ) ;
#5813 = CARTESIAN_POINT ( 'NONE',  ( -33.51255700051650877, -23.73791477778911130, 11.05961554403171299 ) ) ;
#5814 = LINE ( 'NONE', #44393, #95042 ) ;
#5815 = PLANE ( 'NONE',  #42768 ) ;
#5816 = CARTESIAN_POINT ( 'NONE',  ( -3.388261204761456646, -14.20760230196127516, 0.000000000000000000 ) ) ;
#5817 = CARTESIAN_POINT ( 'NONE',  ( 22.99805582222048272, -0.5679727363130141482, -1.500000000000002220 ) ) ;
#5818 = CIRCLE ( 'NONE', #46378, 4.300000000000000711 ) ;
#5819 = PERSON_AND_ORGANIZATION_ROLE ( 'creator' ) ;
#5820 = LINE ( 'NONE', #44900, #87215 ) ;
#5821 = LINE ( 'NONE', #6322, #96025 ) ;
#5822 = CARTESIAN_POINT ( 'NONE',  ( 17.50376878386636292, -9.983289808088789741, 11.49999999999999645 ) ) ;
#5823 = CARTESIAN_POINT ( 'NONE',  ( -108.9756736452620771, -25.28814302825212934, 3.908685561323612667 ) ) ;
#5824 = FACE_OUTER_BOUND ( 'NONE', #1681, .T. ) ;
#5825 = AXIS2_PLACEMENT_3D ( 'NONE', #63338, #94256, #78015 ) ;
#5827 = CARTESIAN_POINT ( 'NONE',  ( -6.741682653110981249, -5.965225279485572685, 30.62569541381301619 ) ) ;
#5826 = VECTOR ( 'NONE', #16529, 999.9999999999998863 ) ;
#5828 = LINE ( 'NONE', #37777, #39160 ) ;
#5829 = CARTESIAN_POINT ( 'NONE',  ( 29.73860345376319003, -4.772782019468681192, -4.021180035027960287 ) ) ;
#5830 = CARTESIAN_POINT ( 'NONE',  ( -16.51628311069853083, -11.03946451426814690, -1.500000000000002220 ) ) ;
#5831 = VECTOR ( 'NONE', #85170, 1000.000000000000000 ) ;
#5832 = FACE_OUTER_BOUND ( 'NONE', #7513, .T. ) ;
#5833 = CARTESIAN_POINT ( 'NONE',  ( -7.851535696030730982, 18.15458241006858131, -1.500000000000002220 ) ) ;
#5834 = CIRCLE ( 'NONE', #72339, 2.040000000000000036 ) ;
#5835 = CARTESIAN_POINT ( 'NONE',  ( -126.6252828959654693, -23.48786465467241769, 11.44779295918253759 ) ) ;
#5836 = B_SPLINE_CURVE_WITH_KNOTS ( 'NONE', 3,
 ( #53391, #5702, #68115, #59503, #84319, #14304 ),
 .UNSPECIFIED., .F., .F.,
 ( 4, 2, 4 ),
 ( 0.000000000000000000, 0.001380764517854767351, 0.002761529035709534702 ),
 .UNSPECIFIED. ) ;
#5837 = EDGE_CURVE ( 'NONE', #88037, #65689, #57458, .T. ) ;
#5838 = DIRECTION ( 'NONE',  ( 0.000000000000000000, 0.000000000000000000, 1.000000000000000000 ) ) ;
#5839 = DIRECTION ( 'NONE',  ( 0.000000000000000000, 0.000000000000000000, -1.000000000000000000 ) ) ;
#5840 = CARTESIAN_POINT ( 'NONE',  ( -19.40337959798338119, 7.141409694766009508, 11.49999999999999645 ) ) ;
#5841 = CARTESIAN_POINT ( 'NONE',  ( -39.53777310077231277, -25.27985545899512587, 5.501674941588943213 ) ) ;
#5842 = EDGE_CURVE ( 'NONE', #13993, #38068, #92441, .T. ) ;
#5843 = CARTESIAN_POINT ( 'NONE',  ( 31.21829842716237735, 4.540774721315884221, 2.131740660352481775 ) ) ;
#5844 = DIRECTION ( 'NONE',  ( -1.000000000000000000, -3.773278334444166432E-23, -8.201307841325785021E-29 ) ) ;
#5845 = CARTESIAN_POINT ( 'NONE',  ( 7.379361219544559702, 21.46082085352547963, 11.49999999999999645 ) ) ;
#5846 = VERTEX_POINT ( 'NONE', #50831 ) ;
#5847 = CARTESIAN_POINT ( 'NONE',  ( -67.52287095715006160, -23.72747288104470087, -1.053458166803226792 ) ) ;
#5848 = FACE_OUTER_BOUND ( 'NONE', #55846, .T. ) ;
#5849 = CARTESIAN_POINT ( 'NONE',  ( -13.64458216870221818, 14.86554040878868044, -1.500000000000002220 ) ) ;
#5850 = CARTESIAN_POINT ( 'NONE',  ( 8.456965425111588885, -0.2003331576018184679, -3.712238059855192951 ) ) ;
#5851 = FACE_OUTER_BOUND ( 'NONE', #83884, .T. ) ;
#5852 = VECTOR ( 'NONE', #63386, 1000.000000000000000 ) ;
#5853 = VERTEX_POINT ( 'NONE', #65578 ) ;
#5854 = ORIENTED_EDGE ( 'NONE', *, *, #54318, .F. ) ;
#5855 = CARTESIAN_POINT ( 'NONE',  ( -0.3982818654701407723, -5.876774720514410077, 19.46306892155547530 ) ) ;
#5856 = CARTESIAN_POINT ( 'NONE',  ( 10.78062712001149492, -20.16176685268226976, -1.500000000000002220 ) ) ;
#5857 = CARTESIAN_POINT ( 'NONE',  ( -29.53073231778219210, -24.42996351905146568, 0.6176547996449994749 ) ) ;
#5858 = CARTESIAN_POINT ( 'NONE',  ( 18.49883484089910723, -11.16122333755292750, -1.500000000000002220 ) ) ;
#5859 = CARTESIAN_POINT ( 'NONE',  ( -123.6259815149813619, -23.73766607897670866, -1.055555164236449350 ) ) ;
#5860 = CARTESIAN_POINT ( 'NONE',  ( -65.52287095715006160, -24.15431212366389602, -0.2830839119429243156 ) ) ;
#5861 = CARTESIAN_POINT ( 'NONE',  ( 14.20245820080859289, -17.52920931871068433, 11.49999999999999645 ) ) ;
#5862 = ORIENTED_EDGE ( 'NONE', *, *, #30640, .F. ) ;
#5863 = CARTESIAN_POINT ( 'NONE',  ( -28.37181345154649392, -24.87786573453352901, 2.467876546412420602 ) ) ;
#5864 = CARTESIAN_POINT ( 'NONE',  ( 21.52718982488130450, -4.553922534329950089, -1.500000000000002220 ) ) ;
#5865 = CARTESIAN_POINT ( 'NONE',  ( -105.5221828483186357, -23.48786465467241769, 11.44779295918254114 ) ) ;
#5866 = CARTESIAN_POINT ( 'NONE',  ( -41.16467076663393243, -25.10925807807259247, 3.014416003260400156 ) ) ;
#5867 = ORIENTED_EDGE ( 'NONE', *, *, #20848, .F. ) ;
#5868 = LINE ( 'NONE', #36825, #86532 ) ;
#5869 = DIRECTION ( 'NONE',  ( 0.000000000000000000, -1.000000000000000000, 0.000000000000000000 ) ) ;
#5870 = ORIENTED_EDGE ( 'NONE', *, *, #58819, .F. ) ;
#5871 = CARTESIAN_POINT ( 'NONE',  ( -84.62287095715007013, -24.50216790748101303, 0.6166512839513667021 ) ) ;
#5872 = VERTEX_POINT ( 'NONE', #96493 ) ;
#5873 = B_SPLINE_CURVE_WITH_KNOTS ( 'NONE', 3,
 ( #42568, #57789, #10599, #56800, #72018, #89728, #64423, #57304, #2499, #58288, #95338, #95837, #73504, #18699, #49682, #66415 ),
 .UNSPECIFIED., .F., .F.,
 ( 4, 2, 2, 2, 2, 2, 2, 4 ),
 ( 0.000000000000000000, 0.0001840283733332804216, 0.0003680567466665608431, 0.0007361134933331239631, 0.0009201418666664060381, 0.001104170239999688113, 0.001288198613332970296, 0.001472226986666252263 ),
 .UNSPECIFIED. ) ;
#5874 = ORIENTED_EDGE ( 'NONE', *, *, #17942, .T. ) ;
#5875 = DIRECTION ( 'NONE',  ( -2.313651251573816365E-16, -1.000000000000000000, -8.068660792749104624E-16 ) ) ;
#5876 = CARTESIAN_POINT ( 'NONE',  ( -104.5228709571501184, -23.48783264082477373, -1.443836473390087027 ) ) ;
#5877 = CARTESIAN_POINT ( 'NONE',  ( -104.6353747070892553, -23.48786465467241413, 11.44779295918254469 ) ) ;
#5878 = CARTESIAN_POINT ( 'NONE',  ( 14.97853827808193294, 13.91023239937271860, -1.500000000000002220 ) ) ;
#5879 = ORIENTED_EDGE ( 'NONE', *, *, #48517, .F. ) ;
#5880 = CARTESIAN_POINT ( 'NONE',  ( -3.085512303079157359, -5.876774720514414518, 19.95084900476495093 ) ) ;
#5881 = DIRECTION ( 'NONE',  ( -0.8246584009594636333, 0.5656310827093757876, 0.000000000000000000 ) ) ;
#5882 = AXIS2_PLACEMENT_3D ( 'NONE', #64268, #87578, #57150 ) ;
#5883 = LINE ( 'NONE', #21592, #59461 ) ;
#5884 = CARTESIAN_POINT ( 'NONE',  ( -25.53098197642538736, -24.91566218739149363, 4.942811707542018596 ) ) ;
#5885 = ORIENTED_EDGE ( 'NONE', *, *, #9249, .T. ) ;
#5886 = CARTESIAN_POINT ( 'NONE',  ( -10.40290173325841216, -5.356774720514425603, 27.45402280011861862 ) ) ;
#5887 = CARTESIAN_POINT ( 'NONE',  ( -88.52287095715006160, -23.47593901973090524, -1.443836447538996426 ) ) ;
#5888 = CARTESIAN_POINT ( 'NONE',  ( 19.40640353424967302, -7.489167304209242815, 11.49999999999998934 ) ) ;
#5889 = VERTEX_POINT ( 'NONE', #42730 ) ;
#5891 = ORIENTED_EDGE ( 'NONE', *, *, #42071, .T. ) ;
#5890 = CARTESIAN_POINT ( 'NONE',  ( 4.328803674008796065, -6.376774720514406525, 18.75671216747623049 ) ) ;
#5892 = AXIS2_PLACEMENT_3D ( 'NONE', #32686, #86971, #17463 ) ;
#5893 = CARTESIAN_POINT ( 'NONE',  ( -28.98875734969026041, 0.3587747205144265483, 25.61802280011862720 ) ) ;
#5894 = ORIENTED_EDGE ( 'NONE', *, *, #16773, .T. ) ;
#5895 = ORIENTED_EDGE ( 'NONE', *, *, #15857, .T. ) ;
#5896 = VECTOR ( 'NONE', #66051, 1000.000000000000000 ) ;
#5897 = CARTESIAN_POINT ( 'NONE',  ( -105.5228709571500758, -23.47596703998600631, 11.44779298504228038 ) ) ;
#5898 = EDGE_CURVE ( 'NONE', #6243, #69692, #75554, .T. ) ;
#5899 = CARTESIAN_POINT ( 'NONE',  ( -117.7765849230966637, -25.21250125880507653, 3.500947807641612730 ) ) ;
#5900 = AXIS2_PLACEMENT_3D ( 'NONE', #66193, #81888, #12365 ) ;
#5901 = CARTESIAN_POINT ( 'NONE',  ( -4.886549725601808447, -5.876774720514410077, 19.15251819062245175 ) ) ;
#5902 = FACE_OUTER_BOUND ( 'NONE', #61449, .T. ) ;
#5904 = ORIENTED_EDGE ( 'NONE', *, *, #67020, .T. ) ;
#5903 = CARTESIAN_POINT ( 'NONE',  ( 18.07010470096111021, 12.80550835427630574, 11.49999999999999645 ) ) ;
#5905 = CARTESIAN_POINT ( 'NONE',  ( -108.5593186212889520, -23.48783264082478084, -1.443836473390062602 ) ) ;
#5906 = ADVANCED_FACE ( 'NONE', ( #41220 ), #25482, .F. ) ;
#5907 = CARTESIAN_POINT ( 'NONE',  ( -4.753580043990282888, 22.13494492317406070, 11.49999999999998934 ) ) ;
#5908 = AXIS2_PLACEMENT_3D ( 'NONE', #64785, #18567, #57652 ) ;
#5909 = EDGE_CURVE ( 'NONE', #50658, #7479, #18869, .T. ) ;
#5911 = EDGE_LOOP ( 'NONE', ( #3431, #44322, #68522, #30830 ) ) ;
#5910 = FACE_OUTER_BOUND ( 'NONE', #1091, .T. ) ;
#5912 = EDGE_CURVE ( 'NONE', #84523, #59400, #79764, .T. ) ;
#5913 = VERTEX_POINT ( 'NONE', #87381 ) ;
#5914 = ADVANCED_FACE ( 'NONE', ( #73170 ), #49846, .F. ) ;
#5915 = CYLINDRICAL_SURFACE ( 'NONE', #53161, 84.48086791635432746 ) ;
#5916 = CARTESIAN_POINT ( 'NONE',  ( -9.210493908506615313, -17.87979239004878451, 11.49999999999998934 ) ) ;
#5917 = DIRECTION ( 'NONE',  ( -3.773278334453079618E-23, 0.9999999999976377785, 2.173523156925978705E-06 ) ) ;
#5918 = ORIENTED_EDGE ( 'NONE', *, *, #75191, .F. ) ;
#5919 = CARTESIAN_POINT ( 'NONE',  ( -89.52287095715009002, -24.66019654487200441, 8.947790411086119278 ) ) ;
#5920 = CARTESIAN_POINT ( 'NONE',  ( 9.404896790668452411, 20.21284700076377305, -1.500000000000002220 ) ) ;
#5921 = EDGE_CURVE ( 'NONE', #4897, #50678, #28301, .T. ) ;
#5922 = VERTEX_POINT ( 'NONE', #19367 ) ;
#5923 = CARTESIAN_POINT ( 'NONE',  ( -78.62287095715005592, -23.47593901973091235, -1.443836447539004642 ) ) ;
#5924 = CARTESIAN_POINT ( 'NONE',  ( -81.88534077628074215, -25.23679622552714363, 6.293943003980942308 ) ) ;
#5925 = DIRECTION ( 'NONE',  ( 0.000000000000000000, 0.000000000000000000, -1.000000000000000000 ) ) ;
#5926 = AXIS2_PLACEMENT_3D ( 'NONE', #89502, #57575, #80893 ) ;
#5927 = DIRECTION ( 'NONE',  ( -1.000000000000000000, 0.000000000000000000, 0.000000000000000000 ) ) ;
#5928 = CARTESIAN_POINT ( 'NONE',  ( 7.694069055508638399, 17.95645395709951941, 11.49999999999998934 ) ) ;
#5929 = B_SPLINE_CURVE_WITH_KNOTS ( 'NONE', 3,
 ( #35809, #80983, #82472, #81981 ),
 .UNSPECIFIED., .F., .F.,
 ( 4, 4 ),
 ( 0.000000000000000000, 9.999999999998897304E-05 ),
 .UNSPECIFIED. ) ;
#5930 = CARTESIAN_POINT ( 'NONE',  ( -20.86232423683148340, -5.086641213604358391, -1.500000000000002220 ) ) ;
#5931 = CARTESIAN_POINT ( 'NONE',  ( -2.791950601096355733, -6.376774720514417183, 20.17732409774492552 ) ) ;
#5932 = CARTESIAN_POINT ( 'NONE',  ( -120.5228709571500048, -24.92579138211018730, 1.929029949965664015 ) ) ;
#5933 = CARTESIAN_POINT ( 'NONE',  ( 21.57151214508649772, 3.625915217019311583E-15, -1.699999999999999956 ) ) ;
#5934 = CARTESIAN_POINT ( 'NONE',  ( -6.081610112697643622, 21.96313418072945822, -1.500000000000002220 ) ) ;
#5935 = APPROVAL_STATUS ( 'not_yet_approved' ) ;
#5936 = CARTESIAN_POINT ( 'NONE',  ( -96.58651527631003830, -24.51419770103159834, 9.386484678747169852 ) ) ;
#5937 = CARTESIAN_POINT ( 'NONE',  ( 11.62916340711181284, -0.3587747205144265483, 28.75961759920349792 ) ) ;
#5938 = CARTESIAN_POINT ( 'NONE',  ( 4.555139465550277933, 19.45931829295258453, 11.49999999999999645 ) ) ;
#5939 = FACE_OUTER_BOUND ( 'NONE', #31744, .T. ) ;
#5940 = CARTESIAN_POINT ( 'NONE',  ( -57.52287095715005449, -23.48786465467241058, 11.44779295918254824 ) ) ;
#5941 = LINE ( 'NONE', #14550, #63461 ) ;
#5942 = VERTEX_POINT ( 'NONE', #72173 ) ;
#5943 = CARTESIAN_POINT ( 'NONE',  ( 1.949999999999999956, 0.1924999999999999489, 0.1925000000000000322 ) ) ;
#5944 = EDGE_CURVE ( 'NONE', #96134, #1389, #3661, .T. ) ;
#5945 = CARTESIAN_POINT ( 'NONE',  ( -70.62287095715004170, -23.48786465467241058, 11.44779295918254469 ) ) ;
#5946 = CARTESIAN_POINT ( 'NONE',  ( -6.878457297428972161, 20.61903435171069532, -1.500000000000002220 ) ) ;
#5947 = CARTESIAN_POINT ( 'NONE',  ( -4.537657931416015700, -6.376774720514410077, 19.25713806424188235 ) ) ;
#5948 = CARTESIAN_POINT ( 'NONE',  ( 6.425176733589397671, 18.50107501292125178, -1.500000000000002220 ) ) ;
#5949 = CARTESIAN_POINT ( 'NONE',  ( -99.29763196087627364, -25.25808875684148092, 6.184470363489280587 ) ) ;
#5950 = EDGE_CURVE ( 'NONE', #64064, #61556, #3169, .T. ) ;
#5951 = EDGE_LOOP ( 'NONE', ( #79420, #80661, #90756, #6867 ) ) ;
#5952 = DATE_AND_TIME ( #6955, #71720 ) ;
#5953 = CARTESIAN_POINT ( 'NONE',  ( -59.62287095715004881, -23.48783264082478794, -1.443836473390069042 ) ) ;
#5954 = CARTESIAN_POINT ( 'NONE',  ( 3.714529970114099022, -6.376774720514426065, 21.83853177191107520 ) ) ;
#5955 = CARTESIAN_POINT ( 'NONE',  ( 19.38413035786728145, -6.671778716439519030, 11.49999999999999645 ) ) ;
#5956 = CARTESIAN_POINT ( 'NONE',  ( 8.071512145086506607, -2.028487854913506805, -6.500000000000000000 ) ) ;
#5957 = VECTOR ( 'NONE', #68505, 1000.000000000000000 ) ;
#5958 = DIRECTION ( 'NONE',  ( 0.000000000000000000, 0.000000000000000000, -1.000000000000000000 ) ) ;
#5959 = ORIENTED_EDGE ( 'NONE', *, *, #60356, .F. ) ;
#5960 = EDGE_CURVE ( 'NONE', #32849, #47463, #65081, .T. ) ;
#5961 = CARTESIAN_POINT ( 'NONE',  ( 33.74607884027702909, 0.3587747205144265483, -4.999864028243830916 ) ) ;
#5962 = DIRECTION ( 'NONE',  ( 0.06975647374412546897, 0.9975640502598241977, 4.700301109882544451E-17 ) ) ;
#5963 = VECTOR ( 'NONE', #68807, 1000.000000000000000 ) ;
#5964 = PLANE ( 'NONE',  #88970 ) ;
#5965 = AXIS2_PLACEMENT_3D ( 'NONE', #67697, #29606, #97623 ) ;
#5966 = B_SPLINE_CURVE_WITH_KNOTS ( 'NONE', 3,
 ( #69064, #14764, #52351, #90905 ),
 .UNSPECIFIED., .F., .F.,
 ( 4, 4 ),
 ( 0.03052179486661367805, 0.03952822613872867402 ),
 .UNSPECIFIED. ) ;
#5967 = ADVANCED_FACE ( 'NONE', ( #41730 ), #15781, .T. ) ;
#5968 = CARTESIAN_POINT ( 'NONE',  ( -85.52287095715004739, -24.83602698348159876, 1.605859176311262182 ) ) ;
#5969 = ORIENTED_EDGE ( 'NONE', *, *, #25952, .F. ) ;
#5970 = CARTESIAN_POINT ( 'NONE',  ( -119.6228709571500843, -24.34917612406838217, 0.1852690917426684236 ) ) ;
#5971 = VECTOR ( 'NONE', #14646, 1000.000000000000114 ) ;
#5972 = CARTESIAN_POINT ( 'NONE',  ( -15.77545706029219730, -16.76941864122914083, 11.49999999999999645 ) ) ;
#5973 = CARTESIAN_POINT ( 'NONE',  ( -10.92962168092244823, 19.99562239114850826, 11.49999999999998934 ) ) ;
#5974 = CARTESIAN_POINT ( 'NONE',  ( 3.787259615384621192, -6.376774720514426065, 21.48076923076922640 ) ) ;
#5975 = DIRECTION ( 'NONE',  ( -0.000000000000000000, -0.000000000000000000, -1.000000000000000000 ) ) ;
#5976 = CARTESIAN_POINT ( 'NONE',  ( -49.56812738534774354, -25.24883509930233672, 3.728933213414787229 ) ) ;
#5977 = DIRECTION ( 'NONE',  ( 0.000000000000000000, 2.173523156925980399E-06, -0.9999999999976378895 ) ) ;
#5978 = CARTESIAN_POINT ( 'NONE',  ( -110.5878966670114494, -24.73486907724917572, 1.287355809206965240 ) ) ;
#5979 = B_SPLINE_CURVE_WITH_KNOTS ( 'NONE', 3,
 ( #31666, #48410, #78332, #717 ),
 .UNSPECIFIED., .F., .F.,
 ( 4, 4 ),
 ( 0.2807004413142643595, 0.2897068725863799488 ),
 .UNSPECIFIED. ) ;
#5980 = CARTESIAN_POINT ( 'NONE',  ( 19.28182042344761626, 10.37885539243483812, -1.500000000000002220 ) ) ;
#5981 = CC_DESIGN_PERSON_AND_ORGANIZATION_ASSIGNMENT ( #18428, #47888, ( #55421 ) ) ;
#5982 = CARTESIAN_POINT ( 'NONE',  ( 7.478911390063968767, -5.876774720514421624, 20.82112274756839199 ) ) ;
#5983 = CARTESIAN_POINT ( 'NONE',  ( -87.60283309997878121, -23.48786465467240703, 11.44779295918254647 ) ) ;
#5984 = CARTESIAN_POINT ( 'NONE',  ( -41.45956028061454646, -25.29644670601110690, 4.317464567834644384 ) ) ;
#5985 = CARTESIAN_POINT ( 'NONE',  ( -28.62287095715004881, -23.31954350884483773, -1.443835782653508426 ) ) ;
#5986 = PLANE ( 'NONE',  #61456 ) ;
#5987 = CARTESIAN_POINT ( 'NONE',  ( -43.62287095715004881, -29.50248528299804818, 1.056150453629031594 ) ) ;
#5988 = ORIENTED_EDGE ( 'NONE', *, *, #73110, .T. ) ;
#5989 = CARTESIAN_POINT ( 'NONE',  ( 14.97853827808193294, 13.91023239937271860, -1.500000000000002220 ) ) ;
#5990 = ORIENTED_EDGE ( 'NONE', *, *, #28011, .F. ) ;
#5991 = ORIENTED_EDGE ( 'NONE', *, *, #58155, .F. ) ;
#5992 = EDGE_LOOP ( 'NONE', ( #41990, #47814, #20136, #18360 ) ) ;
#5993 = ORIENTED_EDGE ( 'NONE', *, *, #85675, .F. ) ;
#5994 = CARTESIAN_POINT ( 'NONE',  ( 21.63105218614105851, 7.968772182826888262, -1.500000000000002220 ) ) ;
#5995 = CARTESIAN_POINT ( 'NONE',  ( -61.52208242660627491, -23.48783264082477018, -1.443836473390096575 ) ) ;
#5996 = CARTESIAN_POINT ( 'NONE',  ( -8.208445925564873846, -18.52556626786687488, -1.500000000000002220 ) ) ;
#5997 = ORIENTED_EDGE ( 'NONE', *, *, #50163, .T. ) ;
#5998 = VECTOR ( 'NONE', #60942, 1000.000000000000000 ) ;
#5999 = CARTESIAN_POINT ( 'NONE',  ( -26.09140115595797837, -24.64100662373225603, 2.243760839632586546 ) ) ;
#6000 = CARTESIAN_POINT ( 'NONE',  ( -40.93384499162358736, -25.30615997036905185, 5.482420585942463731 ) ) ;
#6001 = DIRECTION ( 'NONE',  ( -3.773278334453079030E-23, 0.9999999999976377785, 2.173523156925979128E-06 ) ) ;
#6002 = CARTESIAN_POINT ( 'NONE',  ( -99.52218628114583510, -23.48786465467241413, 11.44779295918254469 ) ) ;
#6004 = ORIENTED_EDGE ( 'NONE', *, *, #99966, .F. ) ;
#6003 = CARTESIAN_POINT ( 'NONE',  ( 2.169945595249806125, 21.32849103866527329, 11.49999999999999645 ) ) ;
#6005 = FACE_OUTER_BOUND ( 'NONE', #25921, .T. ) ;
#6006 = CARTESIAN_POINT ( 'NONE',  ( -113.5228709571500616, -23.47596703998600631, 11.44779298504228038 ) ) ;
#6007 = EDGE_LOOP ( 'NONE', ( #31569, #45963, #76413, #66822 ) ) ;
#6008 = CIRCLE ( 'NONE', #22140, 1.150000000000003464 ) ;
#6009 = CARTESIAN_POINT ( 'NONE',  ( 19.89799572200132971, -5.707369160466581270, -1.500000000000002220 ) ) ;
#6010 = ORIENTED_EDGE ( 'NONE', *, *, #48557, .F. ) ;
#6011 = CARTESIAN_POINT ( 'NONE',  ( -100.6228709571500559, -23.48786465467241769, 11.44779295918254114 ) ) ;
#6012 = VERTEX_POINT ( 'NONE', #62323 ) ;
#6013 = CARTESIAN_POINT ( 'NONE',  ( 4.959895098850171102, -6.376774720514411854, 19.67755022954121813 ) ) ;
#6014 = ORIENTED_EDGE ( 'NONE', *, *, #9336, .T. ) ;
#6015 = CARTESIAN_POINT ( 'NONE',  ( 20.40321384664088811, -4.974606123342796060, -1.500000000000002220 ) ) ;
#6016 = EDGE_CURVE ( 'NONE', #84981, #28945, #5296, .T. ) ;
#6017 = CARTESIAN_POINT ( 'NONE',  ( 10.07166557822571207, 19.55152498600455857, 11.49999999999999645 ) ) ;
#6018 = CARTESIAN_POINT ( 'NONE',  ( -73.55409107130910229, -23.96169478059713143, 10.65365249895718236 ) ) ;
#6019 = CARTESIAN_POINT ( 'NONE',  ( 5.070899574700155732, -21.93562493352797915, -1.500000000000002220 ) ) ;
#6020 = VECTOR ( 'NONE', #28381, 1000.000000000000114 ) ;
#6021 = CARTESIAN_POINT ( 'NONE',  ( -16.25153318171239647, -13.25006309444557751, -1.500000000000002220 ) ) ;
#6022 = FACE_OUTER_BOUND ( 'NONE', #13996, .T. ) ;
#6023 = B_SPLINE_CURVE_WITH_KNOTS ( 'NONE', 3,
 ( #33772, #35280, #95671, #80946, #26154, #94663, #65743, #65252, #17541, #57128, #58124, #18540, #50496, #95170 ),
 .UNSPECIFIED., .F., .F.,
 ( 4, 2, 2, 2, 2, 2, 4 ),
 ( 0.000000000000000000, 0.0001582106571450110329, 0.0003164213142900220658, 0.0006328426285800532389, 0.0009492639428700843035, 0.001107474600015089699, 0.001265685257160095202 ),
 .UNSPECIFIED. ) ;
#6024 = CARTESIAN_POINT ( 'NONE',  ( -119.5185284771687435, -24.35071581493544457, 9.817618358456018157 ) ) ;
#6025 = PLANE ( 'NONE',  #68632 ) ;
#6026 = VERTEX_POINT ( 'NONE', #51325 ) ;
#6027 = ADVANCED_FACE ( 'NONE', ( #47097 ), #82267, .F. ) ;
#6028 = ORIENTED_EDGE ( 'NONE', *, *, #63541, .T. ) ;
#6029 = ORIENTED_EDGE ( 'NONE', *, *, #45545, .F. ) ;
#6030 = EDGE_CURVE ( 'NONE', #100104, #24545, #30821, .T. ) ;
#6031 = CARTESIAN_POINT ( 'NONE',  ( -66.59259820813811359, -24.15543982623906771, -0.2315651400026688400 ) ) ;
#6032 = VECTOR ( 'NONE', #69403, 1000.000000000000000 ) ;
#6033 = CARTESIAN_POINT ( 'NONE',  ( -5.607854029519995898, -20.77141283803394955, -1.500000000000002220 ) ) ;
#6034 = PLANE ( 'NONE',  #50527 ) ;
#6035 = ORIENTED_EDGE ( 'NONE', *, *, #57930, .T. ) ;
#6036 = CARTESIAN_POINT ( 'NONE',  ( -20.79277273739468512, 3.736189789763188607, -1.500000000000002220 ) ) ;
#6037 = CARTESIAN_POINT ( 'NONE',  ( -13.89275734969026388, -5.965225279485572685, 30.51402280011862089 ) ) ;
#6038 = CARTESIAN_POINT ( 'NONE',  ( 22.02124265030973760, 5.356774720514425603, 16.20402280011862217 ) ) ;
#6039 = CARTESIAN_POINT ( 'NONE',  ( -100.5228709571500332, -23.85196035786899316, -0.8779234886475159039 ) ) ;
#6040 = CIRCLE ( 'NONE', #25528, 6.600000000000001421 ) ;
#6041 = CARTESIAN_POINT ( 'NONE',  ( 5.097264368844749427, 3.316774720514425567, -27.56135813788841560 ) ) ;
#6042 = DIRECTION ( 'NONE',  ( 0.8219392559241306406, 0.08114015731558892053, -0.5637660281018073150 ) ) ;
#6043 = CARTESIAN_POINT ( 'NONE',  ( -13.28819421967561532, -17.68372732473523001, -1.500000000000002220 ) ) ;
#6044 = CARTESIAN_POINT ( 'NONE',  ( -81.58509740774454144, -24.51419770103159834, 9.386484678747182286 ) ) ;
#6045 = EDGE_CURVE ( 'NONE', #40031, #23809, #64638, .T. ) ;
#6046 = EDGE_LOOP ( 'NONE', ( #73428, #92760, #90766, #92309 ) ) ;
#6047 = FACE_BOUND ( 'NONE', #63065, .T. ) ;
#6048 = CARTESIAN_POINT ( 'NONE',  ( -58.92287095715006018, -23.47596703998600276, 11.44779298504227860 ) ) ;
#6049 = FACE_OUTER_BOUND ( 'NONE', #384, .T. ) ;
#6050 = CARTESIAN_POINT ( 'NONE',  ( 14.76093561896379214, 5.965225279485572685, -27.88148769130088667 ) ) ;
#6051 = CARTESIAN_POINT ( 'NONE',  ( -19.39930850525863804, 0.8904154686948315689, -1.500000000000002220 ) ) ;
#6052 = CARTESIAN_POINT ( 'NONE',  ( 3.659817510876246960, 21.07357064420920878, 11.49999999999998934 ) ) ;
#6053 = CARTESIAN_POINT ( 'NONE',  ( -69.63554751688641886, -25.07830883915396925, 7.394653300768065485 ) ) ;
#6054 = DIRECTION ( 'NONE',  ( 1.000000000000000000, 0.000000000000000000, 0.000000000000000000 ) ) ;
#6055 = CARTESIAN_POINT ( 'NONE',  ( -79.62287095715005592, -23.48783264082478794, -1.443836473390065489 ) ) ;
#6056 = CARTESIAN_POINT ( 'NONE',  ( -27.96875734969026084, -6.143225279485574397, 24.50402280011861933 ) ) ;
#6057 = CARTESIAN_POINT ( 'NONE',  ( 8.854694546379761277, 20.84150027139232364, -1.500000000000002220 ) ) ;
#6058 = ORIENTED_EDGE ( 'NONE', *, *, #21085, .F. ) ;
#6059 = CARTESIAN_POINT ( 'NONE',  ( 3.787259615384621192, -5.876774720514425177, 21.48076923076922640 ) ) ;
#6060 = PLANE ( 'NONE',  #21643 ) ;
#6061 = CARTESIAN_POINT ( 'NONE',  ( 5.507670110241905448, 19.00313184189250038, 11.49999999999999645 ) ) ;
#6062 = CARTESIAN_POINT ( 'NONE',  ( -70.58953762381673869, -25.00182538069145011, 7.747789668545102870 ) ) ;
#6063 = B_SPLINE_CURVE_WITH_KNOTS ( 'NONE', 3,
 ( #24688, #17084, #40436, #39429 ),
 .UNSPECIFIED., .F., .F.,
 ( 4, 4 ),
 ( 0.000000000000000000, 9.999999999997510880E-05 ),
 .UNSPECIFIED. ) ;
#6064 = PLANE ( 'NONE',  #26915 ) ;
#6065 = EDGE_LOOP ( 'NONE', ( #64564, #92466, #78642, #80127 ) ) ;
#6066 = CARTESIAN_POINT ( 'NONE',  ( 14.73434868161571920, -2.682774720514425670, -27.37990131745768707 ) ) ;
#6067 = CARTESIAN_POINT ( 'NONE',  ( -32.50560602629348494, -29.50248678627064081, 1.747779886239157809 ) ) ;
#6068 = CARTESIAN_POINT ( 'NONE',  ( 8.597998336517790108, -19.88058937513707392, 11.49999999999998934 ) ) ;
#6069 = VECTOR ( 'NONE', #98615, 1000.000000000000000 ) ;
#6070 = CARTESIAN_POINT ( 'NONE',  ( -26.45501174925725962, -24.85202181775033736, 6.809000457855336030 ) ) ;
#6071 = CARTESIAN_POINT ( 'NONE',  ( 17.66168439605153395, -8.020940556088177686, -1.500000000000002220 ) ) ;
#6072 = DIRECTION ( 'NONE',  ( 0.000000000000000000, 1.000000000000000000, 0.000000000000000000 ) ) ;
#6073 = CARTESIAN_POINT ( 'NONE',  ( 7.526024287269984292, 4.772774720514425972, 9.032262774691707463 ) ) ;
#6074 = CARTESIAN_POINT ( 'NONE',  ( -19.81728208556213389, 0.3677575464312098363, -1.500000000000002220 ) ) ;
#6075 = EDGE_CURVE ( 'NONE', #98743, #90405, #87614, .T. ) ;
#6076 = B_SPLINE_CURVE_WITH_KNOTS ( 'NONE', 3,
 ( #35522, #5056, #21761, #42644, #21265, #6053, #52735, #11664, #37006, #73579, #4068, #27404, #12162, #43130, #54747, #7555 ),
 .UNSPECIFIED., .F., .F.,
 ( 4, 2, 2, 2, 2, 2, 2, 4 ),
 ( 0.000000000000000000, 0.0002739161793723606311, 0.0005478323587447212623, 0.001095664717489443609, 0.001369580896861805541, 0.001643497076234167690, 0.001917413255606529839, 0.002191329434978891988 ),
 .UNSPECIFIED. ) ;
#6077 = EDGE_LOOP ( 'NONE', ( #73628, #15986, #6004, #10856, #32353 ) ) ;
#6078 = AXIS2_PLACEMENT_3D ( 'NONE', #58605, #13410, #73824 ) ;
#6079 = CARTESIAN_POINT ( 'NONE',  ( -17.48930418531667996, -10.34094407820366612, 11.49999999999999645 ) ) ;
#6080 = CARTESIAN_POINT ( 'NONE',  ( -8.160000000000000142, -9.728493947732140157, 1.239948043688426926 ) ) ;
#6081 = EDGE_CURVE ( 'NONE', #91131, #55445, #23416, .T. ) ;
#6082 = EDGE_CURVE ( 'NONE', #69136, #42281, #53208, .T. ) ;
#6083 = ORIENTED_EDGE ( 'NONE', *, *, #52560, .F. ) ;
#6084 = CARTESIAN_POINT ( 'NONE',  ( -0.05019100999760693627, -22.40023793344692393, 1.063373454495736725 ) ) ;
#6085 = DIRECTION ( 'NONE',  ( -1.000000000000000000, -0.000000000000000000, -0.000000000000000000 ) ) ;
#6086 = LINE ( 'NONE', #4607, #38635 ) ;
#6087 = CARTESIAN_POINT ( 'NONE',  ( 3.509873074917118085, -0.3587747205144265483, 29.15869884040363758 ) ) ;
#6088 = DIRECTION ( 'NONE',  ( -0.000000000000000000, 1.000000000000000000, -0.000000000000000000 ) ) ;
#6089 = CARTESIAN_POINT ( 'NONE',  ( -14.05898297266747221, -14.31596314050798568, 11.49999999999998934 ) ) ;
#6090 = CARTESIAN_POINT ( 'NONE',  ( -120.5895376238167103, -25.00182538069146432, 7.747789668545101094 ) ) ;
#6091 = ORIENTED_EDGE ( 'NONE', *, *, #79142, .F. ) ;
#6092 = CARTESIAN_POINT ( 'NONE',  ( -117.6228709571500559, -24.64965695001469115, 8.947790433994175174 ) ) ;
#6093 = VECTOR ( 'NONE', #6673, 1000.000000000000114 ) ;
#6094 = CARTESIAN_POINT ( 'NONE',  ( 9.312063170398973355, -20.82641193498425025, 11.49999999999999645 ) ) ;
#6095 = CARTESIAN_POINT ( 'NONE',  ( -49.62307173802614102, -25.26258801428243572, 4.349864120288108538 ) ) ;
#6096 = LINE ( 'NONE', #51783, #98006 ) ;
#6097 = CARTESIAN_POINT ( 'NONE',  ( -102.6228709571500559, -29.50250243563736774, 8.947779886222138046 ) ) ;
#6098 = DIRECTION ( 'NONE',  ( 0.000000000000000000, -1.000000000000000000, 0.000000000000000000 ) ) ;
#6099 = EDGE_CURVE ( 'NONE', #71512, #65451, #62285, .T. ) ;
#6100 = VECTOR ( 'NONE', #35954, 1000.000000000000114 ) ;
#6101 = EDGE_CURVE ( 'NONE', #39894, #77573, #64849, .T. ) ;
#6102 = LINE ( 'NONE', #21811, #12188 ) ;
#6103 = DIRECTION ( 'NONE',  ( 0.000000000000000000, 0.9999999999976377785, 2.173523156925979128E-06 ) ) ;
#6104 = ORIENTED_EDGE ( 'NONE', *, *, #73379, .F. ) ;
#6105 = CARTESIAN_POINT ( 'NONE',  ( -18.95781532540867076, -7.450117396690965066, 11.49999999999998934 ) ) ;
#6106 = EDGE_LOOP ( 'NONE', ( #73299, #63937, #16387, #34774 ) ) ;
#6107 = CARTESIAN_POINT ( 'NONE',  ( 11.31314246093949727, 19.96360691973900359, -1.500000000000002220 ) ) ;
#6108 = PLANE ( 'NONE',  #77642 ) ;
#6110 = EDGE_LOOP ( 'NONE', ( #6146, #50049, #56706, #9627 ) ) ;
#6109 = EDGE_CURVE ( 'NONE', #75450, #9293, #95059, .T. ) ;
#6111 = LINE ( 'NONE', #76112, #46117 ) ;
#6112 = EDGE_CURVE ( 'NONE', #82884, #83477, #53836, .T. ) ;
#6113 = CARTESIAN_POINT ( 'NONE',  ( -77.55884324271059427, -23.73791477778911840, 11.05961554403170588 ) ) ;
#6114 = CARTESIAN_POINT ( 'NONE',  ( -51.58728277246709837, -24.35071581493543036, 9.817618358456028815 ) ) ;
#6116 = VERTEX_POINT ( 'NONE', #24738 ) ;
#6115 = CARTESIAN_POINT ( 'NONE',  ( -16.96849063341007380, -12.82450338531451450, 11.49999999999999645 ) ) ;
#6117 = ADVANCED_FACE ( 'NONE', ( #32867 ), #55217, .T. ) ;
#6118 = VERTEX_POINT ( 'NONE', #63841 ) ;
#6119 = CARTESIAN_POINT ( 'NONE',  ( 17.16062296631688255, 14.07911611715085876, 11.49999999999998934 ) ) ;
#6120 = CARTESIAN_POINT ( 'NONE',  ( -20.60850594246137035, -0.7621957659720622891, 11.49999999999998934 ) ) ;
#6121 = ORIENTED_EDGE ( 'NONE', *, *, #12306, .F. ) ;
#6122 = ORIENTED_EDGE ( 'NONE', *, *, #27889, .F. ) ;
#6123 = FACE_BOUND ( 'NONE', #77144, .T. ) ;
#6124 = CARTESIAN_POINT ( 'NONE',  ( -56.62287095715008434, -24.34917612406837506, 0.1852690917426586537 ) ) ;
#6125 = ORIENTED_EDGE ( 'NONE', *, *, #24330, .T. ) ;
#6126 = ORIENTED_EDGE ( 'NONE', *, *, #44181, .F. ) ;
#6127 = CARTESIAN_POINT ( 'NONE',  ( -125.0508404609613535, -25.24693487555286708, 3.801655821953191960 ) ) ;
#6128 = CARTESIAN_POINT ( 'NONE',  ( -41.52884051539315635, -24.66019654487199375, 8.947790411086124607 ) ) ;
#6129 = CARTESIAN_POINT ( 'NONE',  ( -130.5728709571500588, -23.50397814795999096, 11.46586199002818418 ) ) ;
#6130 = CARTESIAN_POINT ( 'NONE',  ( -20.74012505511919713, -1.853331690952414013, -1.500000000000002220 ) ) ;
#6131 = ADVANCED_FACE ( 'NONE', ( #57225 ), #88157, .F. ) ;
#6132 = CARTESIAN_POINT ( 'NONE',  ( -21.74948284930419717, -1.071797830193938372, 11.49999999999999645 ) ) ;
#6133 = CARTESIAN_POINT ( 'NONE',  ( -51.40810796848847986, -25.09333842084080146, 7.265259977906233679 ) ) ;
#6134 = CARTESIAN_POINT ( 'NONE',  ( 9.071512145086499501, 0.000000000000000000, 3.687490859131163923 ) ) ;
#6135 = AXIS2_PLACEMENT_3D ( 'NONE', #65853, #88169, #14014 ) ;
#6136 = CARTESIAN_POINT ( 'NONE',  ( 14.18375884139645215, 17.39688726336347102, -1.500000000000002220 ) ) ;
#6137 = LINE ( 'NONE', #61443, #5998 ) ;
#6138 = ORIENTED_EDGE ( 'NONE', *, *, #88764, .T. ) ;
#6139 = CARTESIAN_POINT ( 'NONE',  ( -71.45307692756523466, -25.31256585376154433, 5.292613253404210738 ) ) ;
#6140 = CARTESIAN_POINT ( 'NONE',  ( 32.70426658926474062, 3.547616055647111022, -3.273583889775387057 ) ) ;
#6141 = B_SPLINE_SURFACE_WITH_KNOTS ( 'NONE', 3, 1, ( 
 ( #36621, #58976 ),
 ( #20886, #4688 ),
 ( #50865, #27022 ),
 ( #12777, #13273 ),
 ( #28509, #65608 ),
 ( #89915, #19891 ),
 ( #20384, #35636 ),
 ( #82298, #51358 ),
 ( #3693, #96527 ),
 ( #57988, #88926 ),
 ( #19396, #11789 ),
 ( #43746, #97521 ),
 ( #81304, #42759 ),
 ( #74681, #5175 ),
 ( #73692, #81802 ),
 ( #75177, #5671 ),
 ( #67590, #12277 ),
 ( #43255, #98507 ),
 ( #4188, #35141 ),
 ( #66111, #97027 ),
 ( #39116, #62466 ),
 ( #69068, #99004 ),
 ( #83789, #30501 ) ),
 .UNSPECIFIED., .F., .F., .F.,
 ( 4, 1, 1, 1, 1, 1, 1, 1, 1, 1, 1, 1, 1, 1, 1, 1, 1, 1, 1, 1, 4 ),
 ( 2, 2 ),
 ( 0.000000000000000000, 0.06568119799063881770, 0.1284864641740647850, 0.1881751303280078946, 0.2451061306699865161, 0.2994484245294755653, 0.3508229360093824689, 0.3999416805337780434, 0.4466717436323727197, 0.4912545333734983366, 0.5333763442704372304, 0.5738527549682245210, 0.6125263117194527096, 0.6495971364453301256, 0.6855320415538502798, 0.7201057860682015255, 0.7538376629736506240, 0.8189254160467146493, 0.8804934616501651767, 0.9403113338460583615, 1.000000000000000000 ),
 ( 0.000000000000000000, 1.000000000000000000 ),
 .UNSPECIFIED. ) ;
#6142 = VERTEX_POINT ( 'NONE', #10521 ) ;
#6143 = VERTEX_POINT ( 'NONE', #41481 ) ;
#6145 = ADVANCED_FACE ( 'NONE', ( #72437 ), #70075, .T. ) ;
#6144 = DIRECTION ( 'NONE',  ( 0.000000000000000000, -0.000000000000000000, -1.000000000000000000 ) ) ;
#6146 = ORIENTED_EDGE ( 'NONE', *, *, #27326, .F. ) ;
#6147 = CARTESIAN_POINT ( 'NONE',  ( 0.1273799443098547757, 21.28700333820561497, -1.500000000000002220 ) ) ;
#6148 = EDGE_CURVE ( 'NONE', #64607, #96582, #44131, .T. ) ;
#6149 = ORIENTED_EDGE ( 'NONE', *, *, #65294, .F. ) ;
#6150 = DIRECTION ( 'NONE',  ( 0.06486421869277853025, 0.000000000000000000, -0.9978940991575084851 ) ) ;
#6151 = CARTESIAN_POINT ( 'NONE',  ( -15.31302551872622075, -14.39686070098267479, 11.49999999999998934 ) ) ;
#6152 = CARTESIAN_POINT ( 'NONE',  ( 24.50000000000000000, -0.9000000000000000222, -2.000000000000000000 ) ) ;
#6153 = CARTESIAN_POINT ( 'NONE',  ( 15.00349588318476712, -3.443263483566525007, -27.42854228801664007 ) ) ;
#6154 = CARTESIAN_POINT ( 'NONE',  ( -28.49194798280534968, -0.3587747205144265483, 28.38521343323375490 ) ) ;
#6155 = CARTESIAN_POINT ( 'NONE',  ( 21.59112034314636119, 3.954845139028329015, -1.500000000000002220 ) ) ;
#6156 = CARTESIAN_POINT ( 'NONE',  ( -27.13414387080440093, 0.3587747205144061202, -10.21530720150730609 ) ) ;
#6157 = ORIENTED_EDGE ( 'NONE', *, *, #23504, .T. ) ;
#6158 = CARTESIAN_POINT ( 'NONE',  ( -80.53885740889012368, -25.30580248539637012, 4.514386826132675168 ) ) ;
#6159 = ADVANCED_FACE ( 'NONE', ( #35861 ), #59474, .T. ) ;
#6160 = VECTOR ( 'NONE', #27173, 1000.000000000000000 ) ;
#6161 = EDGE_CURVE ( 'NONE', #55098, #35049, #38348, .T. ) ;
#6162 = CARTESIAN_POINT ( 'NONE',  ( 0.4325450954222598288, 0.000000000000000000, 2.350000000000000089 ) ) ;
#6163 = CARTESIAN_POINT ( 'NONE',  ( -130.5728709571500303, -24.04615231314292600, -0.4716817114508828346 ) ) ;
#6164 = CARTESIAN_POINT ( 'NONE',  ( -30.61626505086094951, -24.37935006484465106, 9.703205396196684873 ) ) ;
#6165 = CARTESIAN_POINT ( 'NONE',  ( 17.95810460983813783, 11.44545274529666479, -1.500000000000002220 ) ) ;
#6166 = CARTESIAN_POINT ( 'NONE',  ( -40.52287095715005449, -25.00158670708908915, 2.256160236439166411 ) ) ;
#6167 = CARTESIAN_POINT ( 'NONE',  ( -15.87499999999997868, 1.530808498934188119E-16, -1.249999999999997113 ) ) ;
#6168 = B_SPLINE_CURVE_WITH_KNOTS ( 'NONE', 3,
 ( #59384, #75583, #52271, #90326 ),
 .UNSPECIFIED., .F., .F.,
 ( 4, 4 ),
 ( 0.000000000000000000, 9.999999999997510880E-05 ),
 .UNSPECIFIED. ) ;
#6169 = CARTESIAN_POINT ( 'NONE',  ( 15.99992875909482137, -3.579156900695799060, -27.91088829768895963 ) ) ;
#6170 = VECTOR ( 'NONE', #62550, 1000.000000000000114 ) ;
#6171 = CARTESIAN_POINT ( 'NONE',  ( -33.55276516485183436, -23.96119346886880308, -0.6495511937832006977 ) ) ;
#6172 = CARTESIAN_POINT ( 'NONE',  ( -20.53624283083718893, 9.024085183690161216, -1.500000000000002220 ) ) ;
#6173 = CARTESIAN_POINT ( 'NONE',  ( 6.660000000000001030, 1.527978830621527617, 4.717155776778118259 ) ) ;
#6174 = ORIENTED_EDGE ( 'NONE', *, *, #51482, .T. ) ;
#6175 = DIRECTION ( 'NONE',  ( 0.000000000000000000, -0.000000000000000000, -1.000000000000000000 ) ) ;
#6176 = CARTESIAN_POINT ( 'NONE',  ( 19.40334540789412188, 3.064012487144803565, 11.49999999999999645 ) ) ;
#6177 = CARTESIAN_POINT ( 'NONE',  ( -99.17877183848689526, -25.29933319754236720, 4.367345793447098501 ) ) ;
#6178 = VECTOR ( 'NONE', #18816, 1000.000000000000000 ) ;
#6179 = CARTESIAN_POINT ( 'NONE',  ( -89.62287095715004170, -29.50250243563736774, 8.947779886222139822 ) ) ;
#6180 = VERTEX_POINT ( 'NONE', #31234 ) ;
#6181 = CARTESIAN_POINT ( 'NONE',  ( -88.59160659386742509, -24.15620529776628800, 10.23563542870660115 ) ) ;
#6182 = CARTESIAN_POINT ( 'NONE',  ( -42.58953762381672448, -24.64965694238406613, 8.947790433994663672 ) ) ;
#6183 = CARTESIAN_POINT ( 'NONE',  ( -41.32836283488544638, 2.803225279485573207, 39.26872235229541985 ) ) ;
#6184 = CARTESIAN_POINT ( 'NONE',  ( -10.34999999999999254, 0.000000000000000000, -2.500000000000001332 ) ) ;
#6185 = EDGE_CURVE ( 'NONE', #98585, #92378, #17332, .T. ) ;
#6186 = CARTESIAN_POINT ( 'NONE',  ( 2.169241753049089727, -19.58708112974024829, -1.500000000000002220 ) ) ;
#6187 = B_SPLINE_CURVE_WITH_KNOTS ( 'NONE', 3,
 ( #54473, #94526, #64110, #2200 ),
 .UNSPECIFIED., .F., .F.,
 ( 4, 4 ),
 ( 0.1788870530518809898, 0.1798878000926463494 ),
 .UNSPECIFIED. ) ;
#6188 = AXIS2_PLACEMENT_3D ( 'NONE', #84952, #16435, #71243 ) ;
#6189 = ORIENTED_EDGE ( 'NONE', *, *, #62501, .T. ) ;
#6190 = CARTESIAN_POINT ( 'NONE',  ( 33.61713288457014670, -3.416362262365323144, -11.96006463429725564 ) ) ;
#6191 = DIRECTION ( 'NONE',  ( -0.000000000000000000, -1.000000000000000000, -0.000000000000000000 ) ) ;
#6192 = EDGE_CURVE ( 'NONE', #66070, #2943, #25446, .T. ) ;
#6193 = PERSON_AND_ORGANIZATION_ROLE ( 'design_supplier' ) ;
#6194 = EDGE_LOOP ( 'NONE', ( #77645, #12340, #96844, #39597, #18121 ) ) ;
#6195 = CARTESIAN_POINT ( 'NONE',  ( -16.22218391600152643, -6.475225279485573360, -54.85883559227303863 ) ) ;
#6196 = CARTESIAN_POINT ( 'NONE',  ( -84.55620429048337883, -23.48783264082478794, -1.443836473390064601 ) ) ;
#6197 = LINE ( 'NONE', #61499, #32897 ) ;
#6198 = CARTESIAN_POINT ( 'NONE',  ( -118.5210660692146547, -23.73766607897671221, -1.055555164236448462 ) ) ;
#6199 = CARTESIAN_POINT ( 'NONE',  ( 22.81105451610979173, 1.477225279485574028, -18.46691820600746681 ) ) ;
#6200 = CARTESIAN_POINT ( 'NONE',  ( -69.71577706848860601, -25.31201633809909879, 5.512506568089135861 ) ) ;
#6201 = CARTESIAN_POINT ( 'NONE',  ( 4.784292611718075072, 6.376774720514426953, -25.54547254883186014 ) ) ;
#6202 = CARTESIAN_POINT ( 'NONE',  ( 19.86090765050778728, -2.328952942160339212, -1.500000000000002220 ) ) ;
#6203 = LINE ( 'NONE', #60516, #43499 ) ;
#6204 = CARTESIAN_POINT ( 'NONE',  ( -45.59295858554241221, -24.40133493613049964, 9.663955038902802386 ) ) ;
#6205 = ORIENTED_EDGE ( 'NONE', *, *, #57726, .T. ) ;
#6206 = FACE_OUTER_BOUND ( 'NONE', #7010, .T. ) ;
#6207 = DIRECTION ( 'NONE',  ( -4.472869286569340140E-16, 1.000000000000000000, 7.102795889480464408E-16 ) ) ;
#6208 = CARTESIAN_POINT ( 'NONE',  ( -12.64432969575899968, -0.3587747205143967943, -26.13179214487285407 ) ) ;
#6209 = DIRECTION ( 'NONE',  ( 0.000000000000000000, 2.173523156925980399E-06, -0.9999999999976378895 ) ) ;
#6210 = DIRECTION ( 'NONE',  ( -1.000000000000000000, -3.773278334444167608E-23, -8.201307833595939069E-29 ) ) ;
#6211 = CARTESIAN_POINT ( 'NONE',  ( -28.27781825664440873, -24.60093909322488415, 1.715750617954505453 ) ) ;
#6212 = CARTESIAN_POINT ( 'NONE',  ( -1.371775545366004545, -5.876774720514413630, 20.39230070883894186 ) ) ;
#6213 = EDGE_CURVE ( 'NONE', #18460, #45193, #83519, .T. ) ;
#6214 = B_SPLINE_SURFACE_WITH_KNOTS ( 'NONE', 3, 3, ( 
 ( #98398, #11185, #27905, #51245 ),
 ( #42157, #81195, #89805, #58861 ),
 ( #36012, #97900, #4076, #74089 ),
 ( #3585, #82683, #18787, #49766 ),
 ( #57880, #80696, #44135, #27413 ),
 ( #96920, #66987, #57386, #20275 ),
 ( #58372, #35028, #12672, #65500 ) ),
 .UNSPECIFIED., .F., .F., .F.,
 ( 4, 3, 4 ),
 ( 4, 4 ),
 ( 0.0004766839783814931075, 0.1029713700210893451, 0.2054660560637971978 ),
 ( 0.5096236367946838097, 0.5108715007603359393 ),
 .UNSPECIFIED. ) ;
#6215 = LINE ( 'NONE', #68129, #73808 ) ;
#6216 = LINE ( 'NONE', #20434, #100299 ) ;
#6217 = EDGE_LOOP ( 'NONE', ( #9518, #93130, #1179, #52330 ) ) ;
#6218 = CARTESIAN_POINT ( 'NONE',  ( -13.42616926349082895, -15.17935092467416069, 11.49999999999998934 ) ) ;
#6219 = CARTESIAN_POINT ( 'NONE',  ( -122.5900856979687603, -24.15543982623907482, -0.2315651400026565443 ) ) ;
#6220 = CARTESIAN_POINT ( 'NONE',  ( 20.57455539870835537, 4.132774720514415634, -18.22080502500613974 ) ) ;
#6221 = EDGE_CURVE ( 'NONE', #28633, #41093, #56176, .T. ) ;
#6222 = EDGE_CURVE ( 'NONE', #94651, #21242, #29741, .T. ) ;
#6223 = CARTESIAN_POINT ( 'NONE',  ( -83.52287095715007581, -23.48783264082477018, -1.443836473390090802 ) ) ;
#6224 = EDGE_CURVE ( 'NONE', #69183, #26963, #59767, .T. ) ;
#6225 = VERTEX_POINT ( 'NONE', #22603 ) ;
#6226 = CYLINDRICAL_SURFACE ( 'NONE', #38811, 2.499999999999963141 ) ;
#6227 = CARTESIAN_POINT ( 'NONE',  ( 10.86264265031000775, 1.324225279485583551, -28.05717073599341660 ) ) ;
#6228 = CARTESIAN_POINT ( 'NONE',  ( -8.609638109768802394, 18.19638482192696216, -1.500000000000002220 ) ) ;
#6229 = CARTESIAN_POINT ( 'NONE',  ( 0.3207198112191017025, -21.10926996749724083, 11.49999999999999645 ) ) ;
#6230 = EDGE_CURVE ( 'NONE', #28349, #30238, #15008, .T. ) ;
#6231 = CARTESIAN_POINT ( 'NONE',  ( -89.81226385320383088, -25.26364009184147008, 3.993462176398974162 ) ) ;
#6232 = CARTESIAN_POINT ( 'NONE',  ( 2.303347834742990763, 21.97011321758780866, -1.500000000000002220 ) ) ;
#6233 = CARTESIAN_POINT ( 'NONE',  ( -17.34406541665444124, 10.97931167347951842, 11.49999999999998934 ) ) ;
#6234 = CARTESIAN_POINT ( 'NONE',  ( 22.81105451610979173, -1.682774720514426114, -18.46691820600746681 ) ) ;
#6235 = CARTESIAN_POINT ( 'NONE',  ( 31.02038118199824268, 5.152774720514427642, -4.893189986691015569 ) ) ;
#6236 = ORIENTED_EDGE ( 'NONE', *, *, #460, .F. ) ;
#6237 = CARTESIAN_POINT ( 'NONE',  ( -111.5228709571500616, -24.65952944569305316, 1.056160979905704123 ) ) ;
#6238 = ORIENTED_EDGE ( 'NONE', *, *, #41569, .T. ) ;
#6239 = DIRECTION ( 'NONE',  ( 0.000000000000000000, 0.000000000000000000, 1.000000000000000000 ) ) ;
#6240 = CARTESIAN_POINT ( 'NONE',  ( -48.87380231474225667, -25.26256937810135028, 6.137091986423513390 ) ) ;
#6241 = ORIENTED_EDGE ( 'NONE', *, *, #24909, .T. ) ;
#6242 = CONICAL_SURFACE ( 'NONE', #84040, 1.249999999999996003, 0.7853981633974514986 ) ;
#6243 = VERTEX_POINT ( 'NONE', #98747 ) ;
#6244 = CARTESIAN_POINT ( 'NONE',  ( 22.65031661608482594, -1.684774720501991618, -20.71116937900383448 ) ) ;
#6245 = CARTESIAN_POINT ( 'NONE',  ( -0.3244794670026783234, -9.612687562450236811, 9.000000000000000000 ) ) ;
#6246 = CARTESIAN_POINT ( 'NONE',  ( -0.1037292527911751056, -6.376774720514413630, 19.53657742262743824 ) ) ;
#6247 = CARTESIAN_POINT ( 'NONE',  ( 19.39738937107077632, -6.937168198526852514, -1.500000000000002220 ) ) ;
#6248 = EDGE_CURVE ( 'NONE', #32532, #58649, #67145, .T. ) ;
#6249 = ADVANCED_FACE ( 'NONE', ( #52087 ), #44477, .F. ) ;
#6250 = CARTESIAN_POINT ( 'NONE',  ( 14.45009471711328786, 16.04676183837579373, 11.49999999999999645 ) ) ;
#6251 = ORIENTED_EDGE ( 'NONE', *, *, #649, .T. ) ;
#6252 = DIRECTION ( 'NONE',  ( -1.000000000000000000, -3.773278334444167608E-23, -8.201307833595939069E-29 ) ) ;
#6253 = CARTESIAN_POINT ( 'NONE',  ( -35.58953762381671737, -23.48783264082477729, -1.443836473390072372 ) ) ;
#6254 = CARTESIAN_POINT ( 'NONE',  ( 19.81157572017019319, -10.35993776028809421, 11.49999999999998934 ) ) ;
#6255 = CARTESIAN_POINT ( 'NONE',  ( -34.52287095715004739, -24.66019654487199730, 8.947790411086121054 ) ) ;
#6256 = CARTESIAN_POINT ( 'NONE',  ( -84.55846692228539041, -23.73766607897669445, -1.055555164236457344 ) ) ;
#6257 = ORIENTED_EDGE ( 'NONE', *, *, #70402, .T. ) ;
#6258 = CARTESIAN_POINT ( 'NONE',  ( 32.16024265030974050, 5.965225279485572685, 16.27760796525321751 ) ) ;
#6259 = CARTESIAN_POINT ( 'NONE',  ( -35.57729810147962723, -24.83644354573578994, 8.397322867130093016 ) ) ;
#6260 = VECTOR ( 'NONE', #22906, 1000.000000000000000 ) ;
#6261 = CARTESIAN_POINT ( 'NONE',  ( 18.75483278694074940, -9.228467059531109129, -1.500000000000002220 ) ) ;
#6262 = ORIENTED_EDGE ( 'NONE', *, *, #13583, .F. ) ;
#6263 = B_SPLINE_CURVE_WITH_KNOTS ( 'NONE', 3,
 ( #72338, #33258, #34275, #65740 ),
 .UNSPECIFIED., .F., .F.,
 ( 4, 4 ),
 ( 0.1799143969445999580, 0.1889208282167155195 ),
 .UNSPECIFIED. ) ;
#6266 = ORIENTED_EDGE ( 'NONE', *, *, #86906, .F. ) ;
#6265 = ADVANCED_FACE ( 'NONE', ( #5902 ), #84021, .F. ) ;
#6264 = CARTESIAN_POINT ( 'NONE',  ( -86.63220112534330042, -24.15543982623907482, -0.2315651400026493556 ) ) ;
#6267 = ORIENTED_EDGE ( 'NONE', *, *, #33647, .T. ) ;
#6268 = CARTESIAN_POINT ( 'NONE',  ( -100.5511717382577928, -24.40133493613050319, 9.663955038902802386 ) ) ;
#6269 = CARTESIAN_POINT ( 'NONE',  ( -7.596101150008887082, -19.70107428960382734, -1.500000000000002220 ) ) ;
#6270 = ORIENTED_EDGE ( 'NONE', *, *, #23171, .T. ) ;
#6271 = CARTESIAN_POINT ( 'NONE',  ( -60.58953762381671737, -24.99156044556202261, 7.747789690856174083 ) ) ;
#6272 = DIRECTION ( 'NONE',  ( -3.773278334453079618E-23, 0.9999999999976377785, 2.173523156925979975E-06 ) ) ;
#6273 = CARTESIAN_POINT ( 'NONE',  ( -17.45706314325883213, 13.02611496694466275, -1.500000000000002220 ) ) ;
#6274 = PLANE ( 'NONE',  #57858 ) ;
#6275 = FACE_OUTER_BOUND ( 'NONE', #52825, .T. ) ;
#6276 = CARTESIAN_POINT ( 'NONE',  ( -123.5228709571500616, -29.50248528299804818, 1.056150453629045360 ) ) ;
#6277 = CARTESIAN_POINT ( 'NONE',  ( 15.29254711327534899, -15.47666941828629739, -1.500000000000002220 ) ) ;
#6278 = CARTESIAN_POINT ( 'NONE',  ( -71.33541886227440898, -25.31639513781093598, 5.089068469391626159 ) ) ;
#6280 = VERTEX_POINT ( 'NONE', #99727 ) ;
#6279 = CARTESIAN_POINT ( 'NONE',  ( 7.974090105135403839, 20.87195307945309963, 11.49999999999999645 ) ) ;
#6281 = CARTESIAN_POINT ( 'NONE',  ( -5.366453405989236813, 2.681976490132703452E-15, -21.89999999999999858 ) ) ;
#6282 = CARTESIAN_POINT ( 'NONE',  ( -110.3346797185884327, -25.19502912051678933, 3.293943094755625633 ) ) ;
#6283 = CARTESIAN_POINT ( 'NONE',  ( 32.34323322234308051, -6.036341485554500785, 0.7979233379450167973 ) ) ;
#6285 = ORIENTED_EDGE ( 'NONE', *, *, #40097, .F. ) ;
#6284 = EDGE_CURVE ( 'NONE', #67077, #37098, #14005, .T. ) ;
#6286 = EDGE_CURVE ( 'NONE', #13745, #27602, #68309, .T. ) ;
#6287 = ORIENTED_EDGE ( 'NONE', *, *, #98913, .T. ) ;
#6288 = EDGE_CURVE ( 'NONE', #45475, #30329, #2988, .T. ) ;
#6289 = ORIENTED_EDGE ( 'NONE', *, *, #93198, .T. ) ;
#6290 = CARTESIAN_POINT ( 'NONE',  ( -63.52287095715003318, -23.48783264082477018, -1.443836473390091690 ) ) ;
#6291 = CARTESIAN_POINT ( 'NONE',  ( 3.302162439418223627, -20.95225242093645690, 11.49999999999998934 ) ) ;
#6292 = CARTESIAN_POINT ( 'NONE',  ( -36.62287095715005592, -29.50250786944525672, 11.44777988621624232 ) ) ;
#6293 = CARTESIAN_POINT ( 'NONE',  ( -79.20032202190461135, -25.27791825670924553, 6.885559576519126423 ) ) ;
#6294 = LINE ( 'NONE', #74799, #11319 ) ;
#6295 = DIRECTION ( 'NONE',  ( -0.09824042138329590335, 0.9951627101165078093, 3.519298150595267489E-15 ) ) ;
#6296 = CARTESIAN_POINT ( 'NONE',  ( -13.43510958081001050, -13.94331287200543024, -1.500000000000002220 ) ) ;
#6297 = ADVANCED_FACE ( 'NONE', ( #76398 ), #85015, .F. ) ;
#6298 = DIRECTION ( 'NONE',  ( 0.000000000000000000, 1.000000000000000000, 0.000000000000000000 ) ) ;
#6299 = ORIENTED_EDGE ( 'NONE', *, *, #7135, .F. ) ;
#6300 = CIRCLE ( 'NONE', #63030, 1.000000000000000222 ) ;
#6301 = CARTESIAN_POINT ( 'NONE',  ( -12.57844902324429448, -14.85176824229388437, 11.49999999999999645 ) ) ;
#6302 = DIRECTION ( 'NONE',  ( 0.2164396139380966033, -0.9762960071199348056, 4.401934094135205585E-16 ) ) ;
#6303 = AXIS2_PLACEMENT_3D ( 'NONE', #20260, #5048, #19759 ) ;
#6304 = B_SPLINE_CURVE_WITH_KNOTS ( 'NONE', 3,
 ( #4784, #35740, #28122, #90019 ),
 .UNSPECIFIED., .F., .F.,
 ( 4, 4 ),
 ( 4.163336342344337027E-17, 9.999999999998898659E-05 ),
 .UNSPECIFIED. ) ;
#6305 = ORIENTED_EDGE ( 'NONE', *, *, #62012, .T. ) ;
#6306 = CARTESIAN_POINT ( 'NONE',  ( 2.920210193027767076, -6.376774720514413630, 19.64065332113010243 ) ) ;
#6307 = CARTESIAN_POINT ( 'NONE',  ( -116.5228709571500616, -23.48786465467241769, 11.44779295918253759 ) ) ;
#6308 = DIRECTION ( 'NONE',  ( -1.000000000000000000, -0.000000000000000000, -7.994117400814786717E-16 ) ) ;
#6309 = B_SPLINE_CURVE_WITH_KNOTS ( 'NONE', 3,
 ( #76945, #837, #53644, #61258 ),
 .UNSPECIFIED., .F., .F.,
 ( 4, 4 ),
 ( 0.000000000000000000, 9.999999999998897304E-05 ),
 .UNSPECIFIED. ) ;
#6310 = CARTESIAN_POINT ( 'NONE',  ( -30.62205116524630810, -24.04668586515358442, 10.47594215909545312 ) ) ;
#6311 = CARTESIAN_POINT ( 'NONE',  ( 6.560884470684795744, 18.50665934316380756, 11.49999999999998934 ) ) ;
#6312 = CARTESIAN_POINT ( 'NONE',  ( 8.971512145086499856, -0.9999999999999991118, 3.746884140868835367 ) ) ;
#6313 = ORIENTED_EDGE ( 'NONE', *, *, #85647, .T. ) ;
#6314 = CARTESIAN_POINT ( 'NONE',  ( -16.67190562677319932, -13.68652177170558204, 11.49999999999998934 ) ) ;
#6315 = FACE_OUTER_BOUND ( 'NONE', #16949, .T. ) ;
#6316 = CARTESIAN_POINT ( 'NONE',  ( -96.58953762381671027, -23.48783264082478794, -1.443836473390061936 ) ) ;
#6317 = CARTESIAN_POINT ( 'NONE',  ( 3.797776442307698286, -5.876774720514402084, 18.16025641025640525 ) ) ;
#6318 = CARTESIAN_POINT ( 'NONE',  ( -74.52287095715007581, -23.48786465467241058, 11.44779295918254647 ) ) ;
#6319 = CARTESIAN_POINT ( 'NONE',  ( 21.75825945658488436, -7.631246777643061030, -1.500000000000002220 ) ) ;
#6320 = CALENDAR_DATE ( 2026, 9, 10 ) ;
#6321 = LINE ( 'NONE', #37277, #85543 ) ;
#6322 = CARTESIAN_POINT ( 'NONE',  ( -105.6228709571500559, -29.50250786944525672, 11.44777988621622988 ) ) ;
#6323 = CARTESIAN_POINT ( 'NONE',  ( -19.30929855918770954, 5.666966705251045511, 11.49999999999999645 ) ) ;
#6324 = CARTESIAN_POINT ( 'NONE',  ( -84.62287095715008434, -24.33927499327855415, 9.819080762295815390 ) ) ;
#6325 = CARTESIAN_POINT ( 'NONE',  ( -29.49875734969025842, -0.3587747205144265483, 17.86602280011862476 ) ) ;
#6326 = CIRCLE ( 'NONE', #54928, 132.8284398600581824 ) ;
#6327 = CARTESIAN_POINT ( 'NONE',  ( -4.635780534842457001, -5.876774720514410077, 19.53657742262743113 ) ) ;
#6328 = DIRECTION ( 'NONE',  ( -1.000000000000000000, -0.000000000000000000, -0.000000000000000000 ) ) ;
#6329 = DIRECTION ( 'NONE',  ( 0.000000000000000000, 0.000000000000000000, -1.000000000000000000 ) ) ;
#6330 = CARTESIAN_POINT ( 'NONE',  ( 18.24224480919323810, -7.949361806615760528, -1.500000000000002220 ) ) ;
#6331 = CYLINDRICAL_SURFACE ( 'NONE', #45218, 1.836000000000000743 ) ;
#6332 = CARTESIAN_POINT ( 'NONE',  ( -18.42202159362721048, -7.168033771007030097, -1.500000000000002220 ) ) ;
#6333 = CARTESIAN_POINT ( 'NONE',  ( -42.58702278591343315, -24.34968618360933590, 0.1864209137778841396 ) ) ;
#6334 = DESIGN_CONTEXT ( 'detailed design', #97813, 'design' ) ;
#6335 = DIRECTION ( 'NONE',  ( -3.773278334453079030E-23, 0.9999999999976377785, 2.173523156925979128E-06 ) ) ;
#6336 = DIRECTION ( 'NONE',  ( 1.333806637208504346E-15, 0.000000000000000000, 1.000000000000000000 ) ) ;
#6337 = CARTESIAN_POINT ( 'NONE',  ( -19.50335911044312098, -6.847048061534898977, 11.49999999999999645 ) ) ;
#6338 = DIRECTION ( 'NONE',  ( 3.491481338843133355E-15, -1.000000000000000000, 2.352173255807804438E-16 ) ) ;
#6339 = FACE_OUTER_BOUND ( 'NONE', #4380, .T. ) ;
#6340 = CARTESIAN_POINT ( 'NONE',  ( -109.6228709571500559, -29.50248528299804818, 1.056150453629043584 ) ) ;
#6341 = CIRCLE ( 'NONE', #100255, 2.039999999999998703 ) ;
#6342 = CARTESIAN_POINT ( 'NONE',  ( -22.72798930328562150, -0.2126449523330483371, 11.49999999999999645 ) ) ;
#6344 = EDGE_CURVE ( 'NONE', #25080, #79914, #61212, .T. ) ;
#6343 = ORIENTED_EDGE ( 'NONE', *, *, #56463, .F. ) ;
#6345 = CARTESIAN_POINT ( 'NONE',  ( 0.03625801282051022839, -5.876774720514410077, 19.27714342948718240 ) ) ;
#6347 = ADVANCED_FACE ( 'NONE', ( #7895 ), #77395, .T. ) ;
#6346 = CARTESIAN_POINT ( 'NONE',  ( 29.77147767949870882, 5.356774720514427379, 26.15915692125050995 ) ) ;
#6348 = EDGE_CURVE ( 'NONE', #89809, #96286, #98554, .T. ) ;
#6349 = CARTESIAN_POINT ( 'NONE',  ( -5.623992922573770592, 19.38241096367466199, -1.500000000000002220 ) ) ;
#6350 = CARTESIAN_POINT ( 'NONE',  ( -63.53556326798187825, -24.65952944569304250, 1.056160979905695463 ) ) ;
#6351 = B_SPLINE_CURVE_WITH_KNOTS ( 'NONE', 3,
 ( #36152, #44766, #76189, #12794 ),
 .UNSPECIFIED., .F., .F.,
 ( 4, 4 ),
 ( 0.7793352775112003528, 0.7803360245519654903 ),
 .UNSPECIFIED. ) ;
#6352 = EDGE_CURVE ( 'NONE', #68666, #5121, #54581, .T. ) ;
#6353 = CARTESIAN_POINT ( 'NONE',  ( -52.52287095715005449, -23.47593901973090524, -1.443836447538997092 ) ) ;
#6354 = EDGE_CURVE ( 'NONE', #14971, #65243, #65897, .T. ) ;
#6355 = ORIENTED_EDGE ( 'NONE', *, *, #54479, .T. ) ;
#6356 = ADVANCED_FACE ( 'NONE', ( #77892 ), #94128, .T. ) ;
#6357 = ORIENTED_EDGE ( 'NONE', *, *, #80933, .F. ) ;
#6358 = CARTESIAN_POINT ( 'NONE',  ( 0.3376760108279234784, -6.376774720514417183, 20.09898898868105732 ) ) ;
#6359 = CARTESIAN_POINT ( 'NONE',  ( -9.150087108448493822, 20.98025145036519845, 11.49999999999998934 ) ) ;
#6360 = DIRECTION ( 'NONE',  ( -3.773278334453079618E-23, 0.9999999999976377785, 2.173523156925979975E-06 ) ) ;
#6361 = CARTESIAN_POINT ( 'NONE',  ( 5.689979955356517571, -20.79666814084963278, -1.500000000000002220 ) ) ;
#6362 = CARTESIAN_POINT ( 'NONE',  ( -123.5895128515731329, -24.34968618360933945, 0.1864209137778903291 ) ) ;
#6363 = CARTESIAN_POINT ( 'NONE',  ( -34.48977707614956500, -24.34968618360933590, 0.1864209137778841396 ) ) ;
#6364 = CARTESIAN_POINT ( 'NONE',  ( -3.950822543831816080, -20.53616823614468956, 11.49999999999999645 ) ) ;
#6365 = ORIENTED_EDGE ( 'NONE', *, *, #64617, .F. ) ;
#6366 = CARTESIAN_POINT ( 'NONE',  ( -29.11546134910147998, -25.11176486633936022, 3.495844674899231119 ) ) ;
#6367 = CARTESIAN_POINT ( 'NONE',  ( 12.33731239738771102, -18.22686410513083288, -1.500000000000002220 ) ) ;
#6368 = CARTESIAN_POINT ( 'NONE',  ( -105.6317550840261248, -24.15602025860896163, 10.28564288303535967 ) ) ;
#6369 = CARTESIAN_POINT ( 'NONE',  ( -27.68651082257923335, -24.79700317482176786, 7.605672542379497081 ) ) ;
#6370 = ORIENTED_EDGE ( 'NONE', *, *, #42025, .T. ) ;
#6371 = PLANE ( 'NONE',  #33076 ) ;
#6372 = CARTESIAN_POINT ( 'NONE',  ( -90.49972517448894394, -24.92592662359561118, 8.075495903017998245 ) ) ;
#6373 = ORIENTED_EDGE ( 'NONE', *, *, #14607, .T. ) ;
#6374 = FACE_OUTER_BOUND ( 'NONE', #18385, .T. ) ;
#6375 = EDGE_LOOP ( 'NONE', ( #11781, #2174, #49087, #68527 ) ) ;
#6376 = VECTOR ( 'NONE', #29885, 999.9999999999998863 ) ;
#6377 = ORIENTED_EDGE ( 'NONE', *, *, #29753, .F. ) ;
#6378 = CARTESIAN_POINT ( 'NONE',  ( -32.58953762381672448, -24.64898659630367206, 1.056161002820376726 ) ) ;
#6379 = DIRECTION ( 'NONE',  ( -3.773278334453079030E-23, 0.9999999999976377785, 2.173523156925979128E-06 ) ) ;
#6380 = CARTESIAN_POINT ( 'NONE',  ( -36.65740791118662401, -23.73766607897670156, -1.055555164236459120 ) ) ;
#6381 = CARTESIAN_POINT ( 'NONE',  ( 8.549789220347504326, 18.50885834720105905, -1.500000000000002220 ) ) ;
#6382 = EDGE_CURVE ( 'NONE', #1528, #51970, #8397, .T. ) ;
#6383 = ORIENTED_EDGE ( 'NONE', *, *, #89842, .F. ) ;
#6384 = CARTESIAN_POINT ( 'NONE',  ( -2.369893591381136755, -6.376774720514410077, 19.15221817653405623 ) ) ;
#6385 = CIRCLE ( 'NONE', #79310, 3.349999999999998757 ) ;
#6386 = CARTESIAN_POINT ( 'NONE',  ( -115.6228709571500275, -24.51254535404255464, 9.355368623467647637 ) ) ;
#6387 = DIRECTION ( 'NONE',  ( -7.960204194457801640E-17, -1.000000000000000000, 0.000000000000000000 ) ) ;
#6388 = CARTESIAN_POINT ( 'NONE',  ( -28.52287095715005805, -24.48903441264110015, 8.947790432046794251 ) ) ;
#6389 = EDGE_CURVE ( 'NONE', #27315, #80744, #46458, .T. ) ;
#6390 = EDGE_LOOP ( 'NONE', ( #83802, #73561, #23408, #72048 ) ) ;
#6391 = DIRECTION ( 'NONE',  ( -3.773278334444166432E-23, 1.000000000000000000, 0.000000000000000000 ) ) ;
#6392 = AXIS2_PLACEMENT_3D ( 'NONE', #52293, #68514, #59917 ) ;
#6393 = CARTESIAN_POINT ( 'NONE',  ( -29.54485641382474626, -25.26247775934018946, 6.867482800137663546 ) ) ;
#6394 = AXIS2_PLACEMENT_3D ( 'NONE', #81117, #11598, #73510 ) ;
#6395 = B_SPLINE_CURVE_WITH_KNOTS ( 'NONE', 3,
 ( #44823, #84364, #6741, #83866 ),
 .UNSPECIFIED., .F., .F.,
 ( 4, 4 ),
 ( 0.000000000000000000, 0.0001000000000000028644 ),
 .UNSPECIFIED. ) ;
#6396 = CARTESIAN_POINT ( 'NONE',  ( 18.03836333725549324, -10.36167025447706713, -1.500000000000002220 ) ) ;
#6397 = ORIENTED_EDGE ( 'NONE', *, *, #60836, .T. ) ;
#6399 = ORIENTED_EDGE ( 'NONE', *, *, #59316, .T. ) ;
#6398 = DIRECTION ( 'NONE',  ( 3.773278334444166432E-23, -1.000000000000000000, 0.000000000000000000 ) ) ;
#6400 = CARTESIAN_POINT ( 'NONE',  ( -107.6228709571500701, -29.50247984919015209, -1.443849546365048253 ) ) ;
#6401 = ORIENTED_EDGE ( 'NONE', *, *, #85445, .T. ) ;
#6402 = EDGE_LOOP ( 'NONE', ( #39396, #89291, #7255, #51192 ) ) ;
#6403 = CARTESIAN_POINT ( 'NONE',  ( -65.62287095715005592, -23.48786465467241058, 11.44779295918254647 ) ) ;
#6404 = FACE_OUTER_BOUND ( 'NONE', #56949, .T. ) ;
#6405 =( REPRESENTATION_RELATIONSHIP ('NONE','NONE', #96270, #32845 ) REPRESENTATION_RELATIONSHIP_WITH_TRANSFORMATION ( #72867 )SHAPE_REPRESENTATION_RELATIONSHIP( ) );
#6406 =( BOUNDED_CURVE ( )  B_SPLINE_CURVE ( 3, ( #75774, #60085, #44851, #37231 ),
 .UNSPECIFIED., .F., .T. ) 
 B_SPLINE_CURVE_WITH_KNOTS ( ( 4, 4 ),
 ( 1.466983014708610034, 1.570796326794896558 ),
 .UNSPECIFIED. ) 
 CURVE ( )  GEOMETRIC_REPRESENTATION_ITEM ( )  RATIONAL_B_SPLINE_CURVE ( ( 1.000000000000000000, 0.9991021013140741758, 0.9991021013140741758, 1.000000000000000000 ) ) 
 REPRESENTATION_ITEM ( '' )  );
#6407 = DIRECTION ( 'NONE',  ( 0.000000000000000000, 0.000000000000000000, 1.000000000000000000 ) ) ;
#6408 = CARTESIAN_POINT ( 'NONE',  ( -51.62287095715005592, -24.65952944569304250, 1.056160979905695019 ) ) ;
#6409 = PLANE ( 'NONE',  #12521 ) ;
#6410 = CARTESIAN_POINT ( 'NONE',  ( 1.999999999999998224, 0.000000000000000000, 0.000000000000000000 ) ) ;
#6412 = ORIENTED_EDGE ( 'NONE', *, *, #66071, .T. ) ;
#6411 = CARTESIAN_POINT ( 'NONE',  ( 8.970247382295582383, 20.24485829007567617, 11.49999999999999645 ) ) ;
#6413 = CARTESIAN_POINT ( 'NONE',  ( -108.5907138255110880, -24.15543982623907837, -0.2315651400026445539 ) ) ;
#6414 = CARTESIAN_POINT ( 'NONE',  ( 22.31954755298990278, 3.869410565987296380, 11.49999999999998934 ) ) ;
#6415 = EDGE_CURVE ( 'NONE', #44866, #86377, #93125, .T. ) ;
#6417 = ORIENTED_EDGE ( 'NONE', *, *, #47305, .F. ) ;
#6416 = CARTESIAN_POINT ( 'NONE',  ( -27.68651082257923335, -24.79949475646172630, 7.605672536963987262 ) ) ;
#6418 = ORIENTED_EDGE ( 'NONE', *, *, #77124, .T. ) ;
#6419 = CARTESIAN_POINT ( 'NONE',  ( -10.14776687836540070, -4.675267808546679227, 30.20327419389746382 ) ) ;
#6420 = EDGE_CURVE ( 'NONE', #29980, #80353, #80231, .T. ) ;
#6421 = CARTESIAN_POINT ( 'NONE',  ( -2.706554608146168217, 19.95013100808389339, -1.500000000000002220 ) ) ;
#6422 = B_SPLINE_SURFACE_WITH_KNOTS ( 'NONE', 3, 3, ( 
 ( #11064, #18666, #10063, #72976 ),
 ( #32907, #3466, #87691, #57752 ),
 ( #27291, #94793, #73465, #33900 ),
 ( #3959, #34403, #34903, #25282 ),
 ( #96300, #9558, #95795, #26289 ),
 ( #57265, #50625, #88195, #33392 ),
 ( #58246, #18175, #72474, #17673 ) ),
 .UNSPECIFIED., .F., .F., .F.,
 ( 4, 3, 4 ),
 ( 4, 4 ),
 ( 0.0004766839783842919754, 0.1029713700210908994, 0.2054660560637975031 ),
 ( 0.2795651138368219768, 0.2807068292226991280 ),
 .UNSPECIFIED. ) ;
#6423 = DIRECTION ( 'NONE',  ( 0.000000000000000000, 0.000000000000000000, -1.000000000000000000 ) ) ;
#6424 = ORIENTED_EDGE ( 'NONE', *, *, #24819, .F. ) ;
#6425 = LINE ( 'NONE', #99259, #51879 ) ;
#6426 = CARTESIAN_POINT ( 'NONE',  ( 13.91197278145025074, 17.48688927191260234, -1.500000000000002220 ) ) ;
#6427 = ORIENTED_EDGE ( 'NONE', *, *, #59308, .T. ) ;
#6428 = ORIENTED_EDGE ( 'NONE', *, *, #1889, .F. ) ;
#6429 = CARTESIAN_POINT ( 'NONE',  ( -101.5468792378191978, -25.25341103933382314, 6.236250660175814531 ) ) ;
#6430 = CARTESIAN_POINT ( 'NONE',  ( 27.53860345374771867, -1.682774720514426114, -9.482392034746242260 ) ) ;
#6431 = PLANE ( 'NONE',  #31210 ) ;
#6432 = CARTESIAN_POINT ( 'NONE',  ( 1.259127588940877285, 10.83856991095998801, 0.000000000000000000 ) ) ;
#6433 = CARTESIAN_POINT ( 'NONE',  ( -37.62287095715005592, -24.64965695001467694, 8.947790433994187609 ) ) ;
#6434 = CARTESIAN_POINT ( 'NONE',  ( 8.254404603115069960, -17.72612730319335839, 11.49999999999998934 ) ) ;
#6435 = DIRECTION ( 'NONE',  ( 3.773278334444166432E-23, -1.000000000000000000, 0.000000000000000000 ) ) ;
#6436 = CARTESIAN_POINT ( 'NONE',  ( -12.84383942963603964, -17.20202612561282862, -1.500000000000002220 ) ) ;
#6437 = CARTESIAN_POINT ( 'NONE',  ( -2.702089344534958304, -6.376774720514413630, 19.72789237585158162 ) ) ;
#6438 = DIRECTION ( 'NONE',  ( -1.000000000000000000, 0.000000000000000000, -0.000000000000000000 ) ) ;
#6439 = CARTESIAN_POINT ( 'NONE',  ( 7.160000000000000142, -0.1502355682624769706, 6.837492552117866218 ) ) ;
#6440 = VECTOR ( 'NONE', #3740, 1000.000000000000000 ) ;
#6441 = CARTESIAN_POINT ( 'NONE',  ( -22.32109313027335062, -5.015931025267754251, -1.500000000000002220 ) ) ;
#6442 = PERSON_AND_ORGANIZATION_ROLE ( 'design_owner' ) ;
#6443 = CARTESIAN_POINT ( 'NONE',  ( -106.5515553243550642, -24.35071581493544457, 9.817618358456019934 ) ) ;
#6444 = CARTESIAN_POINT ( 'NONE',  ( 31.31283134548411340, 1.682774720514426114, -10.20862453625735533 ) ) ;
#6445 = CARTESIAN_POINT ( 'NONE',  ( 19.86090765050778728, -2.328952942160339212, 11.49999999999999645 ) ) ;
#6446 = DIRECTION ( 'NONE',  ( 0.1827036106964188000, 3.614007241618350743E-15, -0.9831680378442393398 ) ) ;
#6447 = AXIS2_PLACEMENT_3D ( 'NONE', #93452, #47299, #78225 ) ;
#6448 = CARTESIAN_POINT ( 'NONE',  ( -74.59223320385581246, -24.15620529776628800, 10.23563542870659937 ) ) ;
#6449 = CARTESIAN_POINT ( 'NONE',  ( 22.02124265030973760, 7.743225279485574042, 16.20402280011862217 ) ) ;
#6450 = ORIENTED_EDGE ( 'NONE', *, *, #22098, .F. ) ;
#6451 = LINE ( 'NONE', #29284, #99557 ) ;
#6452 = CARTESIAN_POINT ( 'NONE',  ( -2.872281323269014752, -16.94322527948557422, 1.999999999999999556 ) ) ;
#6453 = CARTESIAN_POINT ( 'NONE',  ( -21.72135255055207281, 0.4632500610043824851, -1.500000000000002220 ) ) ;
#6454 = CARTESIAN_POINT ( 'NONE',  ( -60.52287095715006160, -25.00158670708908915, 2.256160236439166411 ) ) ;
#6455 = VECTOR ( 'NONE', #82406, 1000.000000000000114 ) ;
#6456 = CARTESIAN_POINT ( 'NONE',  ( 9.507684299284662188, -17.14340340408069707, -1.500000000000002220 ) ) ;
#6457 = CARTESIAN_POINT ( 'NONE',  ( -93.62287095715005592, -29.50250786944525672, 11.44777988621623344 ) ) ;
#6459 = ORIENTED_EDGE ( 'NONE', *, *, #70975, .T. ) ;
#6458 = CIRCLE ( 'NONE', #27544, 0.8160000000000007248 ) ;
#6460 = VECTOR ( 'NONE', #34061, 1000.000000000000000 ) ;
#6461 = CARTESIAN_POINT ( 'NONE',  ( 5.184553252003285984, -6.475225279485573360, -28.06387035751381731 ) ) ;
#6462 = CARTESIAN_POINT ( 'NONE',  ( 3.474198977381013798, -6.376774720514426065, 21.79108561604954986 ) ) ;
#6463 = CARTESIAN_POINT ( 'NONE',  ( -17.09319154528168383, -11.34935287704045948, 11.49999999999999645 ) ) ;
#6464 = CARTESIAN_POINT ( 'NONE',  ( 3.794707603699265519E-15, -5.876774720514426953, 17.50000000000000000 ) ) ;
#6465 = CARTESIAN_POINT ( 'NONE',  ( -64.62287095715005592, -29.50248528299804818, 1.056150453629034924 ) ) ;
#6466 = B_SPLINE_CURVE_WITH_KNOTS ( 'NONE', 1,
 ( #35219, #56571 ),
 .UNSPECIFIED., .F., .F.,
 ( 2, 2 ),
 ( 0.000000000000000000, 1.000000000000000000 ),
 .UNSPECIFIED. ) ;
#6467 = CIRCLE ( 'NONE', #35659, 25.90800000000000125 ) ;
#6468 = EDGE_CURVE ( 'NONE', #29344, #12604, #77291, .T. ) ;
#6469 = VERTEX_POINT ( 'NONE', #70307 ) ;
#6470 = CARTESIAN_POINT ( 'NONE',  ( -30.49303573129054357, -23.47596703998576118, 11.44779287168131710 ) ) ;
#6471 = CARTESIAN_POINT ( 'NONE',  ( -39.98073487448829155, -25.18430893388618230, 3.395433981284617708 ) ) ;
#6473 = EDGE_CURVE ( 'NONE', #60061, #67442, #88690, .T. ) ;
#6472 = CARTESIAN_POINT ( 'NONE',  ( -101.5895376238167103, -23.48783264082479505, -1.443836473390062380 ) ) ;
#6474 = CARTESIAN_POINT ( 'NONE',  ( -85.52287095715004739, -24.15431212366391023, -0.2830839119429376938 ) ) ;
#6475 = EDGE_CURVE ( 'NONE', #76346, #81696, #39846, .T. ) ;
#6476 = CARTESIAN_POINT ( 'NONE',  ( -119.6228709571500701, -23.96127896941632685, -0.6493128931037793761 ) ) ;
#6477 = EDGE_CURVE ( 'NONE', #23609, #52671, #66955, .T. ) ;
#6478 = CARTESIAN_POINT ( 'NONE',  ( 0.1381291366035634904, -23.06709338131901532, 11.49999999999999645 ) ) ;
#6479 = CARTESIAN_POINT ( 'NONE',  ( 2.581029390964978187, -22.66945732913600509, -1.500000000000002220 ) ) ;
#6480 = CARTESIAN_POINT ( 'NONE',  ( -70.74026866089612042, -25.31517382824369378, 4.894904372083641597 ) ) ;
#6481 = ADVANCED_FACE ( 'NONE', ( #87533 ), #56090, .F. ) ;
#6482 = CARTESIAN_POINT ( 'NONE',  ( -5.115065434581078208, -6.376774720514408301, 19.15054976246387497 ) ) ;
#6483 = DIRECTION ( 'NONE',  ( 0.000000000000000000, 0.000000000000000000, -1.000000000000000000 ) ) ;
#6484 = DIRECTION ( 'NONE',  ( -3.773278334453079030E-23, 0.9999999999976377785, 2.173523156925979128E-06 ) ) ;
#6485 = EDGE_CURVE ( 'NONE', #31685, #57944, #41356, .T. ) ;
#6486 = CARTESIAN_POINT ( 'NONE',  ( -99.19454649804008284, -25.31582273046552700, 5.270710005526405340 ) ) ;
#6487 = CARTESIAN_POINT ( 'NONE',  ( -12.72821696145241255, -17.84489267850806726, -1.500000000000002220 ) ) ;
#6488 = CARTESIAN_POINT ( 'NONE',  ( -87.62287095715004170, -24.65952944569304606, 1.056160979905700348 ) ) ;
#6489 = CARTESIAN_POINT ( 'NONE',  ( -87.54804369446171108, -24.35071581493543391, 9.817618358456025263 ) ) ;
#6490 = CARTESIAN_POINT ( 'NONE',  ( -33.52287095715004028, -24.35013146730201683, 9.818937971375110152 ) ) ;
#6491 = CARTESIAN_POINT ( 'NONE',  ( -78.62986303001336807, -24.34968618360933945, 0.1864209137778830849 ) ) ;
#6492 = CARTESIAN_POINT ( 'NONE',  ( -112.6228709571501128, -24.33832256526968507, 0.1851278514119968077 ) ) ;
#6493 = DIRECTION ( 'NONE',  ( 0.000000000000000000, 0.000000000000000000, -1.000000000000000000 ) ) ;
#6494 = ORIENTED_EDGE ( 'NONE', *, *, #65848, .T. ) ;
#6495 = CARTESIAN_POINT ( 'NONE',  ( 14.46511082492616573, -14.46070965572739730, 11.49999999999998934 ) ) ;
#6496 = ORIENTED_EDGE ( 'NONE', *, *, #82765, .F. ) ;
#6497 = ORIENTED_EDGE ( 'NONE', *, *, #48774, .F. ) ;
#6498 = VERTEX_POINT ( 'NONE', #46970 ) ;
#6499 = VERTEX_POINT ( 'NONE', #3805 ) ;
#6500 = B_SPLINE_CURVE_WITH_KNOTS ( 'NONE', 3,
 ( #83210, #87964, #13696, #44667, #75589, #6092 ),
 .UNSPECIFIED., .F., .F.,
 ( 4, 2, 4 ),
 ( 0.000000000000000000, 0.001380901958385389195, 0.002761803916770778390 ),
 .UNSPECIFIED. ) ;
#6501 = CARTESIAN_POINT ( 'NONE',  ( 6.753845092018655016, 22.03294598498517232, -1.500000000000002220 ) ) ;
#6502 = CARTESIAN_POINT ( 'NONE',  ( -61.54847807619834299, -24.15543982623907127, -0.2315651400026656481 ) ) ;
#6503 = CARTESIAN_POINT ( 'NONE',  ( 19.74221769882431587, -4.499994434135383692, -1.500000000000002220 ) ) ;
#6504 = ORIENTED_EDGE ( 'NONE', *, *, #5510, .F. ) ;
#6505 = CARTESIAN_POINT ( 'NONE',  ( -54.58953762381672448, -24.64965694238406613, 8.947790433994660120 ) ) ;
#6506 = CARTESIAN_POINT ( 'NONE',  ( -7.999999999999996447, -6.376774720514426953, 0.000000000000000000 ) ) ;
#6507 = B_SPLINE_CURVE_WITH_KNOTS ( 'NONE', 3,
 ( #53086, #89640, #66826, #12999 ),
 .UNSPECIFIED., .F., .F.,
 ( 4, 4 ),
 ( 0.1388571714212596120, 0.1398579184620250271 ),
 .UNSPECIFIED. ) ;
#6508 = CARTESIAN_POINT ( 'NONE',  ( -89.81226385320383088, -25.27880950044345454, 5.947789066509452383 ) ) ;
#6509 = CARTESIAN_POINT ( 'NONE',  ( -99.55495890202929843, -23.96169478059713853, 10.65365249895717703 ) ) ;
#6511 = VERTEX_POINT ( 'NONE', #34743 ) ;
#6510 = CARTESIAN_POINT ( 'NONE',  ( -16.73372362409233105, 13.38858591273363174, 11.49999999999999645 ) ) ;
#6512 = CARTESIAN_POINT ( 'NONE',  ( -53.01255352321339842, 1.682774720514426114, 35.59556822165056644 ) ) ;
#6513 = CARTESIAN_POINT ( 'NONE',  ( -34.62287095715005592, -23.47593901973091235, -1.443836447539013301 ) ) ;
#6514 = ORIENTED_EDGE ( 'NONE', *, *, #41198, .F. ) ;
#6515 = CARTESIAN_POINT ( 'NONE',  ( 4.478411676025833010, -20.21887007069289766, 11.49999999999998934 ) ) ;
#6516 = VECTOR ( 'NONE', #31073, 1000.000000000000000 ) ;
#6518 = ORIENTED_EDGE ( 'NONE', *, *, #18937, .F. ) ;
#6517 = LINE ( 'NONE', #7509, #18341 ) ;
#6519 = CARTESIAN_POINT ( 'NONE',  ( -28.63640793023710174, -24.19694052941946438, 0.1864216068622559508 ) ) ;
#6520 = VERTEX_POINT ( 'NONE', #58096 ) ;
#6521 = CARTESIAN_POINT ( 'NONE',  ( 4.263585034174699473, -5.876774720514401196, 18.26968045024142739 ) ) ;
#6522 = VECTOR ( 'NONE', #45204, 1000.000000000000000 ) ;
#6523 = ORIENTED_EDGE ( 'NONE', *, *, #33510, .T. ) ;
#6524 = CARTESIAN_POINT ( 'NONE',  ( 20.11839708684271244, 8.774209887332036217, 11.49999999999999645 ) ) ;
#6525 = CARTESIAN_POINT ( 'NONE',  ( -73.60155561396484813, -23.73791477778911840, 11.05961554403170766 ) ) ;
#6526 = CARTESIAN_POINT ( 'NONE',  ( 15.50834587592193259, -16.38432980155966590, 11.49999999999998934 ) ) ;
#6527 = CARTESIAN_POINT ( 'NONE',  ( 0.9685562702117149758, 20.96446713366763248, -1.500000000000002220 ) ) ;
#6528 = DIRECTION ( 'NONE',  ( -3.773278334453079030E-23, 0.9999999999976377785, 2.173523156925979128E-06 ) ) ;
#6529 = CARTESIAN_POINT ( 'NONE',  ( 5.981014360695730225, -6.376774720514426065, 21.36744920115099333 ) ) ;
#6530 = ORIENTED_EDGE ( 'NONE', *, *, #61002, .T. ) ;
#6531 = VECTOR ( 'NONE', #62060, 1000.000000000000114 ) ;
#6532 = ORIENTED_EDGE ( 'NONE', *, *, #13693, .F. ) ;
#6533 = AXIS2_PLACEMENT_3D ( 'NONE', #94344, #94845, #79120 ) ;
#6534 = ORIENTED_EDGE ( 'NONE', *, *, #64252, .F. ) ;
#6535 = CARTESIAN_POINT ( 'NONE',  ( -66.58776058314595048, -24.34968618360933235, 0.1864209137778773395 ) ) ;
#6536 = EDGE_CURVE ( 'NONE', #19444, #61919, #7631, .T. ) ;
#6537 = AXIS2_PLACEMENT_3D ( 'NONE', #92290, #60371, #100380 ) ;
#6538 = CARTESIAN_POINT ( 'NONE',  ( -11.74548148041400708, 18.04809798412036059, -1.500000000000002220 ) ) ;
#6539 = ADVANCED_FACE ( 'NONE', ( #42378 ), #47409, .T. ) ;
#6540 = FACE_OUTER_BOUND ( 'NONE', #44472, .T. ) ;
#6541 = ORIENTED_EDGE ( 'NONE', *, *, #26398, .T. ) ;
#6542 = CARTESIAN_POINT ( 'NONE',  ( -9.089321149825819290, -19.05894737874082168, 11.49999999999998934 ) ) ;
#6543 = CARTESIAN_POINT ( 'NONE',  ( -126.6228709571500843, -24.65952944569305316, 1.056160979905707675 ) ) ;
#6544 = CARTESIAN_POINT ( 'NONE',  ( -64.51566560751066959, -23.73766607897670156, -1.055555164236459564 ) ) ;
#6545 = PLANE ( 'NONE',  #40525 ) ;
#6546 = LINE ( 'NONE', #90783, #28053 ) ;
#6547 = CARTESIAN_POINT ( 'NONE',  ( -0.6735982426299428338, -5.876774720514410077, 19.16400979764068069 ) ) ;
#6548 = CARTESIAN_POINT ( 'NONE',  ( -19.05511597014879044, -11.33806725510066826, -1.500000000000002220 ) ) ;
#6549 = CARTESIAN_POINT ( 'NONE',  ( -81.56339976896980204, -23.48786465467241058, 11.44779295918254824 ) ) ;
#6550 = VERTEX_POINT ( 'NONE', #50468 ) ;
#6551 = CARTESIAN_POINT ( 'NONE',  ( -6.660000000000001030, 0.000000000000000000, 0.000000000000000000 ) ) ;
#6552 = LINE ( 'NONE', #38000, #15185 ) ;
#6553 = PLANE ( 'NONE',  #64721 ) ;
#6554 = CARTESIAN_POINT ( 'NONE',  ( -100.5100558546852341, -24.52300882791530512, 0.6510814631126384810 ) ) ;
#6555 = CARTESIAN_POINT ( 'NONE',  ( -12.57844902324429448, -14.85176824229388437, 11.49999999999998934 ) ) ;
#6556 = CARTESIAN_POINT ( 'NONE',  ( -21.04715019690976874, -3.721878931196799467, -1.500000000000002220 ) ) ;
#6557 = FACE_OUTER_BOUND ( 'NONE', #44600, .T. ) ;
#6558 = DIRECTION ( 'NONE',  ( -1.000000000000000000, 0.000000000000000000, -3.469446951953617147E-16 ) ) ;
#6559 = CARTESIAN_POINT ( 'NONE',  ( -40.55620429048338593, -25.00158670708908915, 2.256160236439166855 ) ) ;
#6560 = PLANE ( 'NONE',  #33049 ) ;
#6562 = EDGE_CURVE ( 'NONE', #64622, #57117, #73310, .T. ) ;
#6561 = APPROVAL ( #7950, 'UNKNOWN' ) ;
#6563 = CARTESIAN_POINT ( 'NONE',  ( -7.157701736792966507, -21.45640540170154509, -1.500000000000002220 ) ) ;
#6564 = ORIENTED_EDGE ( 'NONE', *, *, #70852, .T. ) ;
#6565 = CARTESIAN_POINT ( 'NONE',  ( 4.127208352283176396, -5.876774720514423400, 21.39624840817692686 ) ) ;
#6566 = CARTESIAN_POINT ( 'NONE',  ( -122.5895376238167245, -23.48783264082479505, -1.443836473390058828 ) ) ;
#6567 = CARTESIAN_POINT ( 'NONE',  ( 18.24360591643979035, -7.691401616277519615, 11.49999999999999645 ) ) ;
#6568 = CARTESIAN_POINT ( 'NONE',  ( -47.52287095715006160, -29.50247984919015209, -1.443849546365058689 ) ) ;
#6569 = ORIENTED_EDGE ( 'NONE', *, *, #66322, .F. ) ;
#6570 = DIRECTION ( 'NONE',  ( -0.000000000000000000, -1.000000000000000000, -0.000000000000000000 ) ) ;
#6571 = DIRECTION ( 'NONE',  ( -0.000000000000000000, -1.000000000000000000, -0.000000000000000000 ) ) ;
#6572 = CARTESIAN_POINT ( 'NONE',  ( 21.56569437331729233, -1.927008741106717604, -1.500000000000002220 ) ) ;
#6573 = CARTESIAN_POINT ( 'NONE',  ( -26.38942647803707686, -24.86721634236063849, 6.669030906457092733 ) ) ;
#6574 = CARTESIAN_POINT ( 'NONE',  ( 4.312616920666290987, -18.91975033782923887, -1.500000000000002220 ) ) ;
#6575 = PLANE ( 'NONE',  #50723 ) ;
#6576 = CARTESIAN_POINT ( 'NONE',  ( -8.418173371947181849, -17.93405594323863284, -1.500000000000002220 ) ) ;
#6577 = VERTEX_POINT ( 'NONE', #20008 ) ;
#6578 = B_SPLINE_CURVE_WITH_KNOTS ( 'NONE', 3,
 ( #43457, #51566, #4888, #12980, #35833, #43945, #67292, #98212 ),
 .UNSPECIFIED., .F., .F.,
 ( 4, 2, 2, 4 ),
 ( -0.001240666984355836069, -0.0002401179793394933766, 0.0007604310256768488825, 0.002761529035709529498 ),
 .UNSPECIFIED. ) ;
#6579 = CARTESIAN_POINT ( 'NONE',  ( -15.63206872509828571, 12.99414084278249071, 11.49999999999999645 ) ) ;
#6580 = CARTESIAN_POINT ( 'NONE',  ( -80.49262340036909791, -25.00158670708910691, 2.256160236439221034 ) ) ;
#6581 = VECTOR ( 'NONE', #37225, 1000.000000000000114 ) ;
#6582 = CARTESIAN_POINT ( 'NONE',  ( -7.160000000000000142, -0.1502355682624769706, 6.837492552117866218 ) ) ;
#6583 = ORIENTED_EDGE ( 'NONE', *, *, #55227, .F. ) ;
#6584 = CARTESIAN_POINT ( 'NONE',  ( -102.5955360307746531, -23.73791477778911840, 11.05961554403170410 ) ) ;
#6585 = CARTESIAN_POINT ( 'NONE',  ( -95.52287095715006160, -24.82576562948887400, 8.398263436605493126 ) ) ;
#6586 = DIRECTION ( 'NONE',  ( 0.000000000000000000, -1.000000000000000000, -0.000000000000000000 ) ) ;
#6587 = CARTESIAN_POINT ( 'NONE',  ( -95.62287095715008434, -24.63287334234179582, 0.9662140553045412972 ) ) ;
#6588 = CARTESIAN_POINT ( 'NONE',  ( -36.52287095715006870, -29.50248528299804818, 1.056150453629031594 ) ) ;
#6589 = CARTESIAN_POINT ( 'NONE',  ( -10.05502934987021391, 17.38067806581081598, 11.49999999999998934 ) ) ;
#6590 = CARTESIAN_POINT ( 'NONE',  ( -85.52287095715007581, -24.51163499207180507, 0.6490370598555504911 ) ) ;
#6592 = ORIENTED_EDGE ( 'NONE', *, *, #6645, .T. ) ;
#6591 = EDGE_CURVE ( 'NONE', #25405, #18886, #11898, .T. ) ;
#6593 = CARTESIAN_POINT ( 'NONE',  ( -130.5728709571500588, -23.56000036390796737, 11.50200000000000244 ) ) ;
#6594 = B_SPLINE_CURVE_WITH_KNOTS ( 'NONE', 3,
 ( #17775, #95393, #96391, #42130, #81166, #56855, #26385, #80667, #73560, #57355 ),
 .UNSPECIFIED., .F., .F.,
 ( 4, 2, 2, 2, 4 ),
 ( 0.000000000000000000, 0.0004025782241721760006, 0.0008051564483443520012, 0.001207734672516527948, 0.001610312896688704002 ),
 .UNSPECIFIED. ) ;
#6595 = AXIS2_PLACEMENT_3D ( 'NONE', #86539, #77909, #61723 ) ;
#6596 = CARTESIAN_POINT ( 'NONE',  ( -20.58715743568940226, -9.973749938417524774, 11.49999999999999645 ) ) ;
#6597 = CARTESIAN_POINT ( 'NONE',  ( -102.5228709571500900, -23.47593901973090524, -1.443836447538996648 ) ) ;
#6598 = EDGE_CURVE ( 'NONE', #85004, #51581, #68200, .T. ) ;
#6599 = CARTESIAN_POINT ( 'NONE',  ( 4.621320343559619737, 12.50000000000004974, 2.100000000000000089 ) ) ;
#6600 = FACE_OUTER_BOUND ( 'NONE', #32604, .T. ) ;
#6601 = VECTOR ( 'NONE', #34344, 1000.000000000000114 ) ;
#6602 = EDGE_CURVE ( 'NONE', #40297, #86774, #17327, .T. ) ;
#6603 = CARTESIAN_POINT ( 'NONE',  ( 5.641025641025643189, -5.876774720514419847, 20.78665865384615330 ) ) ;
#6604 = CARTESIAN_POINT ( 'NONE',  ( 29.64064043116815128, -5.965225279485572685, 28.71191112024341408 ) ) ;
#6605 = LINE ( 'NONE', #37556, #92284 ) ;
#6606 = ORIENTED_EDGE ( 'NONE', *, *, #57607, .F. ) ;
#6607 = CARTESIAN_POINT ( 'NONE',  ( 20.12614038868121824, 2.982395457389826809, -1.500000000000002220 ) ) ;
#6608 = ORIENTED_EDGE ( 'NONE', *, *, #46717, .F. ) ;
#6609 = EDGE_CURVE ( 'NONE', #72159, #62379, #46532, .T. ) ;
#6610 = CARTESIAN_POINT ( 'NONE',  ( 3.929728083993185184, -22.62717521373229701, 11.49999999999998934 ) ) ;
#6611 = PLANE ( 'NONE',  #6392 ) ;
#6612 = ORIENTED_EDGE ( 'NONE', *, *, #11576, .T. ) ;
#6613 = CARTESIAN_POINT ( 'NONE',  ( -101.5292794699970642, -25.23690811000786383, 6.294209816776285216 ) ) ;
#6614 = CARTESIAN_POINT ( 'NONE',  ( -77.58953762381673869, -24.64965694238406968, 8.947790433994654791 ) ) ;
#6615 = B_SPLINE_CURVE_WITH_KNOTS ( 'NONE', 3,
 ( #30879, #40502, #23756, #86663, #61845, #71456 ),
 .UNSPECIFIED., .F., .F.,
 ( 4, 2, 4 ),
 ( 0.000000000000000000, 0.001380901958385379220, 0.002761803916770758441 ),
 .UNSPECIFIED. ) ;
#6616 = CARTESIAN_POINT ( 'NONE',  ( -111.5228709571500616, -24.64965694238407323, 8.947790433994192938 ) ) ;
#6618 = ORIENTED_EDGE ( 'NONE', *, *, #65677, .F. ) ;
#6617 = CARTESIAN_POINT ( 'NONE',  ( 21.23515499356076930, 0.7789969333488580006, 11.49999999999999645 ) ) ;
#6619 = ORIENTED_EDGE ( 'NONE', *, *, #73743, .T. ) ;
#6620 = CARTESIAN_POINT ( 'NONE',  ( 21.60277357391871433, -5.133695162202882578, -1.500000000000002220 ) ) ;
#6621 = CARTESIAN_POINT ( 'NONE',  ( -16.38011734009650411, 12.53836025512309149, 11.49999999999998934 ) ) ;
#6622 = B_SPLINE_CURVE_WITH_KNOTS ( 'NONE', 3,
 ( #54324, #8640, #39584, #46707 ),
 .UNSPECIFIED., .F., .F.,
 ( 4, 4 ),
 ( 0.1406003993035798150, 0.1496068305756953765 ),
 .UNSPECIFIED. ) ;
#6623 = EDGE_LOOP ( 'NONE', ( #73423, #6029, #97349, #91716 ) ) ;
#6624 = ORIENTED_EDGE ( 'NONE', *, *, #34997, .F. ) ;
#6625 = FACE_OUTER_BOUND ( 'NONE', #25238, .T. ) ;
#6626 = CARTESIAN_POINT ( 'NONE',  ( 3.251543564379332008, -5.876774720514424288, 21.68810402963413964 ) ) ;
#6627 = ORIENTED_EDGE ( 'NONE', *, *, #36268, .F. ) ;
#6628 = ORIENTED_EDGE ( 'NONE', *, *, #14530, .F. ) ;
#6629 = CARTESIAN_POINT ( 'NONE',  ( -49.52287095715006870, -23.72773821059535848, 11.05748984161097681 ) ) ;
#6630 = CARTESIAN_POINT ( 'NONE',  ( -29.24636659181000198, -25.21267509515801564, 4.940287023516041209 ) ) ;
#6631 = CARTESIAN_POINT ( 'NONE',  ( -10.15938669249390180, 18.18672505111813464, -1.500000000000002220 ) ) ;
#6632 = CARTESIAN_POINT ( 'NONE',  ( -1.534710021792092594, -21.76038796025502009, 11.49999999999999645 ) ) ;
#6633 = CARTESIAN_POINT ( 'NONE',  ( -39.85957971240202369, -25.20729891577929394, 3.457629610838235834 ) ) ;
#6634 = CARTESIAN_POINT ( 'NONE',  ( -78.58811849685578466, -24.35071581493543391, 9.817618358456027039 ) ) ;
#6635 = CARTESIAN_POINT ( 'NONE',  ( 16.82713599508461400, -14.87465808564757808, 11.49999999999998934 ) ) ;
#6636 = CARTESIAN_POINT ( 'NONE',  ( -50.95636528269795207, -25.26334713686265943, 4.561343367844973962 ) ) ;
#6638 = ORIENTED_EDGE ( 'NONE', *, *, #47320, .T. ) ;
#6637 = EDGE_CURVE ( 'NONE', #58964, #52078, #27042, .T. ) ;
#6639 = LINE ( 'NONE', #91873, #29041 ) ;
#6640 = DIRECTION ( 'NONE',  ( -0.2425356250363331356, -0.9701425001453318764, 0.000000000000000000 ) ) ;
#6641 = ORIENTED_EDGE ( 'NONE', *, *, #7174, .T. ) ;
#6642 = ORIENTED_EDGE ( 'NONE', *, *, #23179, .F. ) ;
#6643 = AXIS2_PLACEMENT_3D ( 'NONE', #69206, #100120, #30641 ) ;
#6644 = CARTESIAN_POINT ( 'NONE',  ( -46.50016940544900024, -24.15620529776627379, 10.23563542870660825 ) ) ;
#6645 = EDGE_CURVE ( 'NONE', #28007, #93008, #59499, .T. ) ;
#6646 = ORIENTED_EDGE ( 'NONE', *, *, #18955, .T. ) ;
#6647 = CARTESIAN_POINT ( 'NONE',  ( 8.224165413489119558, 19.69228431130148493, -1.500000000000002220 ) ) ;
#6648 = ORIENTED_EDGE ( 'NONE', *, *, #11884, .F. ) ;
#6649 = CARTESIAN_POINT ( 'NONE',  ( -5.960145391809922089, -5.876774720514416295, 20.04104409779160534 ) ) ;
#6650 = CARTESIAN_POINT ( 'NONE',  ( -20.98013922110768448, -1.350454208470041273, -1.500000000000002220 ) ) ;
#6651 = CARTESIAN_POINT ( 'NONE',  ( -30.50823467185977833, -24.04845685762501617, -0.4713115009884517037 ) ) ;
#6652 = CARTESIAN_POINT ( 'NONE',  ( -100.3258897876286255, -25.18527973888543769, 3.296414269619829973 ) ) ;
#6653 = LINE ( 'NONE', #37609, #23878 ) ;
#6654 = CARTESIAN_POINT ( 'NONE',  ( -8.017166757594178961, 20.41873492177044724, -1.500000000000002220 ) ) ;
#6655 = DIRECTION ( 'NONE',  ( -3.773278334453079030E-23, 0.9999999999976377785, 2.173523156925979128E-06 ) ) ;
#6656 = VERTEX_POINT ( 'NONE', #51967 ) ;
#6657 = LINE ( 'NONE', #58472, #12953 ) ;
#6658 = B_SPLINE_CURVE_WITH_KNOTS ( 'NONE', 3,
 ( #32119, #94018, #39230, #47860, #46853, #70187, #94520, #671, #17904, #79792, #16897, #31618, #62583, #86410, #93009, #24504 ),
 .UNSPECIFIED., .F., .F.,
 ( 4, 2, 2, 2, 2, 2, 2, 4 ),
 ( 3.496446946337351263E-18, 0.0002171278225386873725, 0.0004342556450773712214, 0.0008685112901547389734, 0.001737022580309472743, 0.002171278225386841579, 0.002605533870464210415, 0.003474045160618947220 ),
 .UNSPECIFIED. ) ;
#6659 = CARTESIAN_POINT ( 'NONE',  ( 8.499999999999989342, 19.99999999999999289, 2.100000000000000089 ) ) ;
#6660 = AXIS2_PLACEMENT_3D ( 'NONE', #92543, #9301, #47885 ) ;
#6661 = CARTESIAN_POINT ( 'NONE',  ( -128.5228709571501611, -23.96127896942151736, -0.6493128930935507803 ) ) ;
#6662 = CARTESIAN_POINT ( 'NONE',  ( -30.58080440576787851, -25.30589263001944644, 6.147794833475635379 ) ) ;
#6663 = CARTESIAN_POINT ( 'NONE',  ( 20.49606604269246546, -5.804284187783010474, 11.49999999999998934 ) ) ;
#6664 = LINE ( 'NONE', #12775, #23920 ) ;
#6665 = CARTESIAN_POINT ( 'NONE',  ( -51.62287095715005592, -23.47596703998600631, 11.44779298504227505 ) ) ;
#6666 = CARTESIAN_POINT ( 'NONE',  ( 15.98199071239991120, -3.493868136757070975, -27.92664602931597884 ) ) ;
#6667 = B_SPLINE_CURVE_WITH_KNOTS ( 'NONE', 3,
 ( #41423, #57166, #17579, #56161, #1864, #17075, #94701, #33808, #87089, #28068, #48550, #64790, #81849, #88104, #19938, #36177, #4730, #66656 ),
 .UNSPECIFIED., .F., .F.,
 ( 4, 2, 2, 2, 2, 2, 2, 2, 4 ),
 ( 0.000000000000000000, 0.0002152204991354002641, 0.0004304409982708005283, 0.0008608819965415918408, 0.001291322994812383208, 0.001721763993083174574, 0.002582645989624761211, 0.003013086987895555180, 0.003443527986166349149 ),
 .UNSPECIFIED. ) ;
#6668 = CARTESIAN_POINT ( 'NONE',  ( -33.63539978109197648, -24.34968618360933235, 0.1864209137778845560 ) ) ;
#6669 = CC_DESIGN_PERSON_AND_ORGANIZATION_ASSIGNMENT ( #33270, #9433, ( #60221 ) ) ;
#6670 = CARTESIAN_POINT ( 'NONE',  ( -11.43049785330379997, -19.34545768653811493, -1.500000000000002220 ) ) ;
#6671 = CARTESIAN_POINT ( 'NONE',  ( 5.202077965628057576, 7.402934475628871785E-15, -2.038091937962834166 ) ) ;
#6672 = ORIENTED_EDGE ( 'NONE', *, *, #88387, .F. ) ;
#6673 = DIRECTION ( 'NONE',  ( -3.773278334453079618E-23, 0.9999999999976377785, 2.173523156925979975E-06 ) ) ;
#6674 = CARTESIAN_POINT ( 'NONE',  ( 16.84789977498956404, 10.09486508543780481, 11.49999999999999645 ) ) ;
#6675 = CARTESIAN_POINT ( 'NONE',  ( -125.6228709571500275, -23.85196035786900381, -0.8779234886475003607 ) ) ;
#6676 = CARTESIAN_POINT ( 'NONE',  ( -82.52287095715003318, -23.96127896942135393, -0.6493128930938705246 ) ) ;
#6677 = B_SPLINE_CURVE_WITH_KNOTS ( 'NONE', 3,
 ( #98077, #99566, #91469, #91974, #81875, #59047, #43325, #66682 ),
 .UNSPECIFIED., .F., .F.,
 ( 4, 2, 2, 4 ),
 ( 6.391158118955260688E-06, 0.002007136338672914442, 0.003007508928949895622, 0.004007881519226877236 ),
 .UNSPECIFIED. ) ;
#6678 = VERTEX_POINT ( 'NONE', #60089 ) ;
#6679 = CARTESIAN_POINT ( 'NONE',  ( -88.52215618628163440, -23.48786465467241413, 11.44779295918254469 ) ) ;
#6680 = CARTESIAN_POINT ( 'NONE',  ( -46.52287095715006160, -29.50248528299804818, 1.056150453629033370 ) ) ;
#6681 = EDGE_CURVE ( 'NONE', #92149, #93833, #59587, .T. ) ;
#6682 = DIRECTION ( 'NONE',  ( 0.000000000000000000, 0.000000000000000000, -1.000000000000000000 ) ) ;
#6683 = CARTESIAN_POINT ( 'NONE',  ( -25.63684490523837667, -24.87290554392149744, 6.232310010065051920 ) ) ;
#6684 = B_SPLINE_CURVE_WITH_KNOTS ( 'NONE', 3,
 ( #19473, #44328, #81383, #20965 ),
 .UNSPECIFIED., .F., .F.,
 ( 4, 4 ),
 ( 0.4908505043302913151, 0.4998569356024067378 ),
 .UNSPECIFIED. ) ;
#6685 = B_SPLINE_CURVE_WITH_KNOTS ( 'NONE', 3,
 ( #22146, #99281, #13542, #92665 ),
 .UNSPECIFIED., .F., .F.,
 ( 4, 4 ),
 ( 0.000000000000000000, 0.0001002978970080590907 ),
 .UNSPECIFIED. ) ;
#6686 = CARTESIAN_POINT ( 'NONE',  ( 7.987771016649366729, -18.01272016045900415, 11.49999999999998934 ) ) ;
#6687 = VERTEX_POINT ( 'NONE', #28623 ) ;
#6688 = FACE_OUTER_BOUND ( 'NONE', #67206, .T. ) ;
#6689 = FACE_OUTER_BOUND ( 'NONE', #94365, .T. ) ;
#6690 = APPLICATION_PROTOCOL_DEFINITION ( 'international standard', 'config_control_design', 1994, #18107 ) ;
#6691 = VERTEX_POINT ( 'NONE', #52465 ) ;
#6692 = CARTESIAN_POINT ( 'NONE',  ( -96.62287095715005592, -24.64898659630368272, 1.056161002820829697 ) ) ;
#6693 = CARTESIAN_POINT ( 'NONE',  ( -103.6228709571500701, -23.96177878511308990, 10.65340807706329862 ) ) ;
#6694 = CARTESIAN_POINT ( 'NONE',  ( -55.50250315067101070, -24.15503026093912808, -0.2815557561904589168 ) ) ;
#6695 = CARTESIAN_POINT ( 'NONE',  ( -99.09546795806416242, -25.03145021834298234, 6.840688129798706996 ) ) ;
#6696 = CARTESIAN_POINT ( 'NONE',  ( -6.720452724358975338, -6.376774720514411854, 19.46153846153846700 ) ) ;
#6697 = CARTESIAN_POINT ( 'NONE',  ( -69.64006105340874342, -25.31201646985301323, 5.573124239722496931 ) ) ;
#6698 = DIRECTION ( 'NONE',  ( 0.000000000000000000, 0.000000000000000000, -1.000000000000000000 ) ) ;
#6700 = ADVANCED_FACE ( 'NONE', ( #98620 ), #44082, .T. ) ;
#6699 = CARTESIAN_POINT ( 'NONE',  ( -19.24466553037914807, -5.328869878250761971, 11.49999999999998934 ) ) ;
#6701 = PLANE ( 'NONE',  #100161 ) ;
#6702 = CARTESIAN_POINT ( 'NONE',  ( -45.52798018843675010, -24.83644354573577928, 8.397322867130094792 ) ) ;
#6703 = ORIENTED_EDGE ( 'NONE', *, *, #91341, .T. ) ;
#6704 = CARTESIAN_POINT ( 'NONE',  ( -119.5193685554757792, -24.15543982623907837, -0.2315651400026547124 ) ) ;
#6705 = CARTESIAN_POINT ( 'NONE',  ( -80.58710785548036881, -24.63419186844610920, 9.035850630976915099 ) ) ;
#6706 = EDGE_CURVE ( 'NONE', #11463, #24959, #57261, .T. ) ;
#6707 = CARTESIAN_POINT ( 'NONE',  ( -124.7734026561379466, -25.27150408776893542, 5.922772873374069214 ) ) ;
#6708 = CARTESIAN_POINT ( 'NONE',  ( -39.52824657088962823, -24.65952944569304250, 1.056160979905697017 ) ) ;
#6709 = AXIS2_PLACEMENT_3D ( 'NONE', #53521, #6819, #61129 ) ;
#6710 = EDGE_CURVE ( 'NONE', #30746, #13059, #91193, .T. ) ;
#6711 = CARTESIAN_POINT ( 'NONE',  ( -119.6228709571500559, -24.64898659630368627, 1.056161002820833028 ) ) ;
#6712 = CARTESIAN_POINT ( 'NONE',  ( -51.44554956638231147, -25.31574398867087439, 4.646412717996129871 ) ) ;
#6713 = DIRECTION ( 'NONE',  ( 0.000000000000000000, 1.000000000000000000, 0.000000000000000000 ) ) ;
#6714 = CARTESIAN_POINT ( 'NONE',  ( 5.402409956206937203, -6.376774720514424288, 21.18719775722114917 ) ) ;
#6715 = ORIENTED_EDGE ( 'NONE', *, *, #19735, .F. ) ;
#6716 = CARTESIAN_POINT ( 'NONE',  ( -18.19507518397214341, 8.946258903265221107, -1.500000000000002220 ) ) ;
#6717 = PLANE ( 'NONE',  #25815 ) ;
#6718 = EDGE_CURVE ( 'NONE', #69295, #35481, #70678, .T. ) ;
#6719 = FACE_OUTER_BOUND ( 'NONE', #29940, .T. ) ;
#6720 = CARTESIAN_POINT ( 'NONE',  ( 30.53060340732035982, -4.594240983522013266, 19.84760796525321425 ) ) ;
#6721 = ORIENTED_EDGE ( 'NONE', *, *, #85622, .T. ) ;
#6722 = CARTESIAN_POINT ( 'NONE',  ( -94.62287095715005592, -23.47596703998600631, 11.44779298504227860 ) ) ;
#6723 = CARTESIAN_POINT ( 'NONE',  ( -1.345681049247692940, -5.876774720514409189, 19.69174559449348294 ) ) ;
#6724 = AXIS2_PLACEMENT_3D ( 'NONE', #87710, #17694, #71494 ) ;
#6725 = CARTESIAN_POINT ( 'NONE',  ( 18.53703574427524359, 7.882278514257341051, -1.500000000000002220 ) ) ;
#6726 = CARTESIAN_POINT ( 'NONE',  ( 3.661087877195506213, -20.73962600213626217, 11.49999999999999645 ) ) ;
#6727 = CC_DESIGN_APPROVAL ( #56303, ( #87801 ) ) ;
#6728 = CARTESIAN_POINT ( 'NONE',  ( -118.5562042904833930, -24.65952944569305316, 1.056160979905707009 ) ) ;
#6729 = CARTESIAN_POINT ( 'NONE',  ( 21.13397978930849064, -6.478279476769641221, -1.500000000000002220 ) ) ;
#6730 = CARTESIAN_POINT ( 'NONE',  ( -1.764913036440812322, 20.45846032914734280, -1.500000000000002220 ) ) ;
#6731 = CARTESIAN_POINT ( 'NONE',  ( -93.62287095715007013, -23.47596703998600631, 11.44779298504227860 ) ) ;
#6732 = CARTESIAN_POINT ( 'NONE',  ( 15.14080536460164694, 5.152774720514426754, -26.62908960815040516 ) ) ;
#6733 = ORIENTED_EDGE ( 'NONE', *, *, #4640, .F. ) ;
#6734 = CARTESIAN_POINT ( 'NONE',  ( 14.76093561896379214, -3.316774720514426456, -26.55548769130089681 ) ) ;
#6735 = ORIENTED_EDGE ( 'NONE', *, *, #3284, .T. ) ;
#6736 = CARTESIAN_POINT ( 'NONE',  ( 33.10875634548599322, -5.965225279485572685, -11.42349945801155719 ) ) ;
#6737 = LINE ( 'NONE', #37691, #77703 ) ;
#6738 = VERTEX_POINT ( 'NONE', #1676 ) ;
#6739 = ORIENTED_EDGE ( 'NONE', *, *, #93642, .T. ) ;
#6740 = ORIENTED_EDGE ( 'NONE', *, *, #52915, .F. ) ;
#6741 = CARTESIAN_POINT ( 'NONE',  ( -65.55620429048337883, -23.48783264082478439, -1.443836473390067487 ) ) ;
#6742 = CARTESIAN_POINT ( 'NONE',  ( -49.52287095715007581, -23.47593901973090169, -1.443836447538997092 ) ) ;
#6743 = CARTESIAN_POINT ( 'NONE',  ( -68.51606030823643323, -23.73791477778911840, 11.05961554403170943 ) ) ;
#6744 = CARTESIAN_POINT ( 'NONE',  ( 19.46067915675286386, 6.892634557253153105, -1.500000000000002220 ) ) ;
#6745 = CARTESIAN_POINT ( 'NONE',  ( -9.004746288917990782, -19.65190454534591069, 11.49999999999999645 ) ) ;
#6746 = ORIENTED_EDGE ( 'NONE', *, *, #92973, .T. ) ;
#6747 = FACE_OUTER_BOUND ( 'NONE', #34614, .T. ) ;
#6748 = CARTESIAN_POINT ( 'NONE',  ( -57.62287095715005592, -24.33927499327854704, 9.819080762295820719 ) ) ;
#6749 = CARTESIAN_POINT ( 'NONE',  ( -21.90463088927077706, -4.570550247397807908, 11.49999999999998934 ) ) ;
#6750 = CARTESIAN_POINT ( 'NONE',  ( 282.9764569301858046, -4.132774720514426292, 20.79159422840526616 ) ) ;
#6751 = CARTESIAN_POINT ( 'NONE',  ( -84.59926806605869842, -23.73766607897669445, -1.055555164236457566 ) ) ;
#6752 = EDGE_LOOP ( 'NONE', ( #10330, #97503, #47451, #94443 ) ) ;
#6753 = FACE_OUTER_BOUND ( 'NONE', #66928, .T. ) ;
#6754 = CARTESIAN_POINT ( 'NONE',  ( 6.546094359317672584, -5.876774720514411854, 19.73546617144828375 ) ) ;
#6755 = CARTESIAN_POINT ( 'NONE',  ( 20.33208665566141704, 4.825383418962623239, -1.500000000000002220 ) ) ;
#6756 = ORIENTED_EDGE ( 'NONE', *, *, #61276, .F. ) ;
#6758 = EDGE_LOOP ( 'NONE', ( #13345, #94360, #40559, #91126 ) ) ;
#6757 = CARTESIAN_POINT ( 'NONE',  ( -67.63597399538805632, -24.15620529776628800, 10.23563542870660115 ) ) ;
#6759 = EDGE_LOOP ( 'NONE', ( #39088, #99453, #60552, #59873 ) ) ;
#6760 = EDGE_CURVE ( 'NONE', #35231, #25716, #29365, .T. ) ;
#6761 = CARTESIAN_POINT ( 'NONE',  ( -109.5865558906285600, -24.66019654487200441, 8.947790411086113949 ) ) ;
#6762 = CARTESIAN_POINT ( 'NONE',  ( 7.804836024166685426, 19.70032748343534834, -1.500000000000002220 ) ) ;
#6763 = ORIENTED_EDGE ( 'NONE', *, *, #99474, .F. ) ;
#6764 = LINE ( 'NONE', #91006, #41407 ) ;
#6765 = CARTESIAN_POINT ( 'NONE',  ( -99.61078991697702634, -25.12215613712814744, 6.818453781472685549 ) ) ;
#6766 = CARTESIAN_POINT ( 'NONE',  ( -12.70408864715453667, 17.69581422525067183, -1.500000000000002220 ) ) ;
#6767 = CARTESIAN_POINT ( 'NONE',  ( -7.641025641025641413, -6.376774720514418959, 20.36458333333334636 ) ) ;
#6768 = CARTESIAN_POINT ( 'NONE',  ( -36.62287095715005592, -24.64898659630367916, 1.056161002820819261 ) ) ;
#6769 = CARTESIAN_POINT ( 'NONE',  ( -95.52287095715006160, -25.00158670708909980, 2.256160236439166411 ) ) ;
#6770 = CARTESIAN_POINT ( 'NONE',  ( -6.878457297428972161, 20.61903435171069532, -1.500000000000002220 ) ) ;
#6771 = DIRECTION ( 'NONE',  ( -3.773278334453079618E-23, 0.9999999999976377785, 2.173523156925979975E-06 ) ) ;
#6773 = ORIENTED_EDGE ( 'NONE', *, *, #81654, .F. ) ;
#6772 = CARTESIAN_POINT ( 'NONE',  ( -2.938769918389303459, -22.12206158279486345, 11.49999999999999645 ) ) ;
#6774 = CARTESIAN_POINT ( 'NONE',  ( -40.62287095715004170, -29.50248789122583659, 2.256150453626215580 ) ) ;
#6775 = CARTESIAN_POINT ( 'NONE',  ( -72.58953762381671027, -24.65952944569304250, 1.056160979905694131 ) ) ;
#6776 = CARTESIAN_POINT ( 'NONE',  ( 32.23945434255342235, -4.540774721353955989, 2.150384428877208709 ) ) ;
#6777 = ORIENTED_EDGE ( 'NONE', *, *, #22783, .T. ) ;
#6778 = ORIENTED_EDGE ( 'NONE', *, *, #16101, .F. ) ;
#6779 = ORIENTED_EDGE ( 'NONE', *, *, #95384, .F. ) ;
#6780 = CARTESIAN_POINT ( 'NONE',  ( -44.62287095715003460, -24.33832256527048088, 0.1851278514138565146 ) ) ;
#6781 = CARTESIAN_POINT ( 'NONE',  ( -14.68016216564755894, -15.32010671487267572, 11.49999999999998934 ) ) ;
#6782 = VECTOR ( 'NONE', #43663, 1000.000000000000114 ) ;
#6783 = DIRECTION ( 'NONE',  ( 0.000000000000000000, 0.000000000000000000, 1.000000000000000000 ) ) ;
#6784 = CARTESIAN_POINT ( 'NONE',  ( -79.38827465850120291, -25.27791877533765685, 7.124171434988036289 ) ) ;
#6785 = CARTESIAN_POINT ( 'NONE',  ( -99.52287095715006160, -24.64898659630529565, 1.056161002820829697 ) ) ;
#6786 = DIRECTION ( 'NONE',  ( -0.9951627101165076983, -0.09824042138329588947, -3.430045979798635096E-16 ) ) ;
#6787 = ADVANCED_FACE ( 'NONE', ( #86898 ), #47346, .F. ) ;
#6788 = CARTESIAN_POINT ( 'NONE',  ( -37.62287095715004881, -23.96177878511307568, 10.65340807706330395 ) ) ;
#6789 = CARTESIAN_POINT ( 'NONE',  ( -39.97837580656372580, -25.32724636324322987, 4.398074533285874388 ) ) ;
#6790 = ORIENTED_EDGE ( 'NONE', *, *, #10326, .T. ) ;
#6791 = CARTESIAN_POINT ( 'NONE',  ( 18.22972481837485859, -6.773019484731225504, 11.49999999999999645 ) ) ;
#6792 = DIRECTION ( 'NONE',  ( 0.000000000000000000, 2.173523156925980399E-06, -0.9999999999976378895 ) ) ;
#6793 = EDGE_CURVE ( 'NONE', #1776, #89773, #83814, .T. ) ;
#6794 = ORIENTED_EDGE ( 'NONE', *, *, #7716, .F. ) ;
#6795 = PLANE ( 'NONE',  #68598 ) ;
#6796 = CARTESIAN_POINT ( 'NONE',  ( 3.797776442307698286, -5.876774720514402084, 18.16025641025640525 ) ) ;
#6797 = EDGE_CURVE ( 'NONE', #12095, #38848, #1523, .T. ) ;
#6798 = CARTESIAN_POINT ( 'NONE',  ( -40.62287095715005592, -29.50250243563736774, 8.947779886222148704 ) ) ;
#6799 = EDGE_CURVE ( 'NONE', #1781, #89454, #56110, .T. ) ;
#6800 = CARTESIAN_POINT ( 'NONE',  ( 26.73860345374794534, -5.058662225110310828, -7.113848178280766099 ) ) ;
#6801 = VECTOR ( 'NONE', #28505, 1000.000000000000000 ) ;
#6802 = CARTESIAN_POINT ( 'NONE',  ( -15.21066300689680872, 12.40131300380995860, 11.49999999999998934 ) ) ;
#6803 = CARTESIAN_POINT ( 'NONE',  ( -120.2228709571500644, -23.47596703998600631, 11.44779298504227860 ) ) ;
#6806 = ADVANCED_FACE ( 'NONE', ( #69683 ), #23040, .T. ) ;
#6805 = ORIENTED_EDGE ( 'NONE', *, *, #61204, .T. ) ;
#6804 = LOCAL_TIME ( 0, 54, 15.00000000000000000, #51509 ) ;
#6807 = CARTESIAN_POINT ( 'NONE',  ( 21.48638754631891246, 1.654510534108022179, -1.500000000000002220 ) ) ;
#6808 = CARTESIAN_POINT ( 'NONE',  ( 10.28385788129874001, 1.335431525194933577, 19.26533332368850182 ) ) ;
#6809 = CARTESIAN_POINT ( 'NONE',  ( -40.62378909974164998, -25.00158670708910336, 2.256160236439222366 ) ) ;
#6810 = CARTESIAN_POINT ( 'NONE',  ( 29.73860345376319358, 1.682774720514426114, -8.849814207987163783 ) ) ;
#6811 = CARTESIAN_POINT ( 'NONE',  ( -18.27982475084466785, -14.08179083545084964, -1.500000000000002220 ) ) ;
#6812 = PERSON_AND_ORGANIZATION_ROLE ( 'creator' ) ;
#6813 = CARTESIAN_POINT ( 'NONE',  ( -93.50738165881485031, -24.51314013834316796, 0.6176544820404163971 ) ) ;
#6814 = CARTESIAN_POINT ( 'NONE',  ( -50.70464068992656337, -25.25249061358302782, 3.767456410489268936 ) ) ;
#6815 = CARTESIAN_POINT ( 'NONE',  ( 0.3675393366473880818, 20.13074986235200470, 11.49999999999999645 ) ) ;
#6816 = CARTESIAN_POINT ( 'NONE',  ( -121.5883697052726404, -24.66019654487200441, 8.947790411086119278 ) ) ;
#6817 = CARTESIAN_POINT ( 'NONE',  ( -5.366453405989236813, 0.000000000000000000, 18.35000000000000142 ) ) ;
#6818 = CARTESIAN_POINT ( 'NONE',  ( -111.4457194297752807, -25.29823926093160225, 3.361188652080160377 ) ) ;
#6819 = DIRECTION ( 'NONE',  ( 1.000000000000000000, 0.000000000000000000, -2.439088438507244272E-15 ) ) ;
#6820 = B_SPLINE_CURVE_WITH_KNOTS ( 'NONE', 3,
 ( #67148, #59521, #51910, #13319, #44299, #70119, #93951, #8727, #46785, #46280, #602, #32555, #77712, #63026, #38662, #8225, #31551, #79223, #17330 ),
 .UNSPECIFIED., .F., .F.,
 ( 4, 1, 1, 1, 1, 1, 1, 1, 1, 1, 1, 1, 1, 1, 1, 1, 4 ),
 ( 0.000000000000000000, 0.07560433049574548370, 0.1479650154827359954, 0.2187969985237009085, 0.2894704453213758910, 0.3597242180874983819, 0.4297077387530445769, 0.5004965198485837874, 0.5744290198679491422, 0.6139472962286710578, 0.6571552698261118319, 0.7039727697209380297, 0.7549389848168008843, 0.8097066112894878431, 0.8688329536985502921, 0.9323854739325977414, 1.000000000000000000 ),
 .UNSPECIFIED. ) ;
#6821 = CARTESIAN_POINT ( 'NONE',  ( 30.09341516180546350, -2.682774720514426559, -11.39311774897855933 ) ) ;
#6823 = EDGE_CURVE ( 'NONE', #20097, #22611, #10280, .T. ) ;
#6822 = CARTESIAN_POINT ( 'NONE',  ( 2.793900936927258272, 19.68708943014846469, 11.49999999999998934 ) ) ;
#6824 = DIRECTION ( 'NONE',  ( -1.000000000000000000, -0.000000000000000000, -0.000000000000000000 ) ) ;
#6825 = CARTESIAN_POINT ( 'NONE',  ( 2.545096341412688812, 19.61957628810408849, -1.500000000000002220 ) ) ;
#6826 = CARTESIAN_POINT ( 'NONE',  ( -42.62870416798130435, -24.51314013834315375, 0.6176544820404090697 ) ) ;
#6827 = FACE_OUTER_BOUND ( 'NONE', #92313, .T. ) ;
#6828 = FACE_OUTER_BOUND ( 'NONE', #44302, .T. ) ;
#6829 = CARTESIAN_POINT ( 'NONE',  ( -0.2510023010970363067, -20.70922355669356563, 11.49999999999999645 ) ) ;
#6830 = CARTESIAN_POINT ( 'NONE',  ( -58.52287095715006870, -24.33832256527049154, 0.1851278514138590403 ) ) ;
#6831 = EDGE_CURVE ( 'NONE', #47882, #25230, #74180, .T. ) ;
#6832 = CARTESIAN_POINT ( 'NONE',  ( -49.59985430115347071, -25.31439339618379947, 5.484775475632647002 ) ) ;
#6833 = B_SPLINE_CURVE_WITH_KNOTS ( 'NONE', 3,
 ( #86265, #77639, #71555, #1540 ),
 .UNSPECIFIED., .F., .F.,
 ( 4, 4 ),
 ( 0.000000000000000000, 9.999999999998206125E-05 ),
 .UNSPECIFIED. ) ;
#6834 = CARTESIAN_POINT ( 'NONE',  ( 19.36006514395606004, 11.85157241509795512, 11.49999999999999645 ) ) ;
#6835 = CONICAL_SURFACE ( 'NONE', #42506, 2.999999999999999112, 0.7853981633974412846 ) ;
#6836 = ORIENTED_EDGE ( 'NONE', *, *, #47177, .F. ) ;
#6837 = B_SPLINE_SURFACE_WITH_KNOTS ( 'NONE', 3, 3, ( 
 ( #81451, #25654, #42407, #19535 ),
 ( #87556, #42892, #56125, #87051 ),
 ( #9927, #40882, #18042, #71842 ),
 ( #64248, #49007, #52496, #98647 ),
 ( #21026, #44890, #66244, #67733 ),
 ( #5810, #67232, #5311, #51003 ),
 ( #97661, #60119, #44389, #27663 ) ),
 .UNSPECIFIED., .F., .F., .F.,
 ( 4, 3, 4 ),
 ( 4, 4 ),
 ( 0.0004766839783815690558, 0.1029713700210891647, 0.2054660560637967537 ),
 ( 0.8397076045168327951, 0.8411077686186837488 ),
 .UNSPECIFIED. ) ;
#6838 = CARTESIAN_POINT ( 'NONE',  ( -29.49875734969025842, 5.965225279485572685, 17.86602280011862476 ) ) ;
#6839 = ADVANCED_FACE ( 'NONE', ( #80798 ), #42748, .F. ) ;
#6840 = CARTESIAN_POINT ( 'NONE',  ( -69.90382545228106892, -25.13695321101799252, 7.020456727309716705 ) ) ;
#6841 = CARTESIAN_POINT ( 'NONE',  ( -13.64458216870221818, 14.86554040878868044, 11.49999999999998934 ) ) ;
#6842 = B_SPLINE_CURVE_WITH_KNOTS ( 'NONE', 3,
 ( #41546, #18686, #49663, #51146, #25812, #73000 ),
 .UNSPECIFIED., .F., .F.,
 ( 4, 2, 4 ),
 ( 1.570755371634013412E-05, 0.001396183895866086886, 0.002776660238015833410 ),
 .UNSPECIFIED. ) ;
#6843 = CARTESIAN_POINT ( 'NONE',  ( -63.55376365945738826, -23.96119346886879597, -0.6495511937832106897 ) ) ;
#6844 = EDGE_CURVE ( 'NONE', #38183, #84725, #75365, .T. ) ;
#6845 = PLANE ( 'NONE',  #26921 ) ;
#6846 = ORIENTED_EDGE ( 'NONE', *, *, #42811, .T. ) ;
#6847 = EDGE_CURVE ( 'NONE', #78994, #65732, #26002, .T. ) ;
#6848 = ORIENTED_EDGE ( 'NONE', *, *, #667, .F. ) ;
#6849 = CARTESIAN_POINT ( 'NONE',  ( 0.3376760108279234784, -5.876774720514417183, 20.09898898868105732 ) ) ;
#6850 = CARTESIAN_POINT ( 'NONE',  ( -17.51315278866654879, 14.73147661606379621, 11.49999999999998934 ) ) ;
#6852 = EDGE_CURVE ( 'NONE', #68551, #5650, #80292, .T. ) ;
#6851 = CARTESIAN_POINT ( 'NONE',  ( -40.62294849466940860, -25.12194742856580376, 2.840355672353660044 ) ) ;
#6853 = CARTESIAN_POINT ( 'NONE',  ( -11.89702471719568244, -18.04982639819725776, -1.500000000000002220 ) ) ;
#6854 = CARTESIAN_POINT ( 'NONE',  ( -123.5215661119650292, -23.73766607897670866, -1.055555164236449350 ) ) ;
#6855 = FACE_OUTER_BOUND ( 'NONE', #84966, .T. ) ;
#6856 = AXIS2_PLACEMENT_3D ( 'NONE', #79955, #58139, #72859 ) ;
#6857 = CARTESIAN_POINT ( 'NONE',  ( 10.02768300834196502, -18.34552750054021786, 11.49999999999999645 ) ) ;
#6858 = EDGE_LOOP ( 'NONE', ( #53462, #39057, #27222, #49591 ) ) ;
#6859 = CARTESIAN_POINT ( 'NONE',  ( 0.000000000000000000, -16.94322527948557422, 0.000000000000000000 ) ) ;
#6860 = VECTOR ( 'NONE', #49666, 1000.000000000000114 ) ;
#6861 = CARTESIAN_POINT ( 'NONE',  ( -10.13730173486854369, -19.54584281717935568, -1.500000000000002220 ) ) ;
#6862 = CARTESIAN_POINT ( 'NONE',  ( -105.5848496801880856, -25.00182538069147142, 7.747789668545044250 ) ) ;
#6863 = CARTESIAN_POINT ( 'NONE',  ( -29.00356289826891754, -24.79700109271441022, 6.647731354146906746 ) ) ;
#6864 = ORIENTED_EDGE ( 'NONE', *, *, #7552, .T. ) ;
#6865 = CARTESIAN_POINT ( 'NONE',  ( 4.263585034174699473, -6.376774720514402972, 18.26968045024142739 ) ) ;
#6866 = CARTESIAN_POINT ( 'NONE',  ( -90.64712538269208153, -23.48786465467241058, 11.44779295918254824 ) ) ;
#6867 = ORIENTED_EDGE ( 'NONE', *, *, #34132, .F. ) ;
#6868 = CARTESIAN_POINT ( 'NONE',  ( -80.52287095715006160, -29.50248789122583659, 2.256150453626215580 ) ) ;
#6869 = ORIENTED_EDGE ( 'NONE', *, *, #67803, .T. ) ;
#6870 = ORIENTED_EDGE ( 'NONE', *, *, #31195, .F. ) ;
#6871 = CARTESIAN_POINT ( 'NONE',  ( -41.52287095715006870, -24.64965694238406613, 8.947790433994205372 ) ) ;
#6872 = LINE ( 'NONE', #31709, #93993 ) ;
#6873 = CARTESIAN_POINT ( 'NONE',  ( -57.53788008658175102, -24.51314013834315375, 0.6176544820404114011 ) ) ;
#6874 = CARTESIAN_POINT ( 'NONE',  ( 12.80116962295325322, 15.99954467330607244, -1.500000000000002220 ) ) ;
#6875 = EDGE_LOOP ( 'NONE', ( #40375, #26746, #96574, #81758 ) ) ;
#6876 = DIRECTION ( 'NONE',  ( 0.000000000000000000, -1.000000000000000000, 0.000000000000000000 ) ) ;
#6877 = LINE ( 'NONE', #98726, #40081 ) ;
#6878 = CARTESIAN_POINT ( 'NONE',  ( 3.750000000000001332, 25.69999999999999574, 2.100000000000000089 ) ) ;
#6879 = CARTESIAN_POINT ( 'NONE',  ( 2.321567282091853812, -22.14299765706108403, 11.49999999999998934 ) ) ;
#6881 = CYLINDRICAL_SURFACE ( 'NONE', #67508, 91.74549126261076992 ) ;
#6880 = AXIS2_PLACEMENT_3D ( 'NONE', #78183, #73593, #87818 ) ;
#6882 = CARTESIAN_POINT ( 'NONE',  ( -85.52287095715006160, -29.50250786944525672, 11.44777988621623344 ) ) ;
#6883 = ORIENTED_EDGE ( 'NONE', *, *, #28067, .T. ) ;
#6884 = DIRECTION ( 'NONE',  ( 0.000000000000000000, 0.000000000000000000, -1.000000000000000000 ) ) ;
#6885 = CARTESIAN_POINT ( 'NONE',  ( -29.81116385467300489, -24.63645367248981799, 5.042946918296252079 ) ) ;
#6886 = CC_DESIGN_APPROVAL ( #90973, ( #91188 ) ) ;
#6887 = CARTESIAN_POINT ( 'NONE',  ( 14.74948264216024008, 14.65492983226340407, -1.500000000000002220 ) ) ;
#6888 = ORIENTED_EDGE ( 'NONE', *, *, #21469, .F. ) ;
#6890 = EDGE_LOOP ( 'NONE', ( #11507, #45357, #2658, #49101 ) ) ;
#6889 = PLANE ( 'NONE',  #77904 ) ;
#6891 = AXIS2_PLACEMENT_3D ( 'NONE', #87182, #42526, #48643 ) ;
#6892 = DIRECTION ( 'NONE',  ( -3.773278334453079030E-23, 0.9999999999976377785, 2.173523156925979128E-06 ) ) ;
#6893 = VERTEX_POINT ( 'NONE', #27008 ) ;
#6894 = ORIENTED_EDGE ( 'NONE', *, *, #93198, .F. ) ;
#6895 = CARTESIAN_POINT ( 'NONE',  ( 7.666860990600891768, 10.67251638830246918, -0.9337241952711420323 ) ) ;
#6896 = CARTESIAN_POINT ( 'NONE',  ( -43.62287095715004881, -29.50247984919015209, -1.443849546365060466 ) ) ;
#6897 = CARTESIAN_POINT ( 'NONE',  ( -117.5801323110720489, -25.21753527833458364, 3.539999278834443874 ) ) ;
#6898 = VECTOR ( 'NONE', #50962, 1000.000000000000114 ) ;
#6899 = CARTESIAN_POINT ( 'NONE',  ( -100.4979344782931037, -25.25419553985774712, 7.562057461207404963 ) ) ;
#6900 = CARTESIAN_POINT ( 'NONE',  ( -108.9621161194473871, -25.27386152548063691, 3.991943336111062113 ) ) ;
#6901 = DIRECTION ( 'NONE',  ( -1.000000000000000000, -3.773278334444166432E-23, -8.201307841325785021E-29 ) ) ;
#6903 = ORIENTED_EDGE ( 'NONE', *, *, #6911, .T. ) ;
#6902 = CARTESIAN_POINT ( 'NONE',  ( -22.12685673520133989, -0.1325007643398395663, 11.49999999999999645 ) ) ;
#6904 = CARTESIAN_POINT ( 'NONE',  ( -91.12544342272609299, -25.36326615310542465, 5.213196219967858092 ) ) ;
#6905 = CARTESIAN_POINT ( 'NONE',  ( -17.75566480456612695, 14.03706703302619374, 11.49999999999998934 ) ) ;
#6907 = VERTEX_POINT ( 'NONE', #88411 ) ;
#6906 = CARTESIAN_POINT ( 'NONE',  ( 26.73860345374794178, -1.682774720514426114, -1.272392034746785860 ) ) ;
#6908 = EDGE_LOOP ( 'NONE', ( #27920, #47981, #80057, #3712 ) ) ;
#6909 = CARTESIAN_POINT ( 'NONE',  ( -61.64687923781919920, -25.13069339737145214, 2.947789366383932297 ) ) ;
#6910 = CIRCLE ( 'NONE', #3670, 10.80000000000000782 ) ;
#6911 = EDGE_CURVE ( 'NONE', #45335, #84371, #40341, .T. ) ;
#6912 = CARTESIAN_POINT ( 'NONE',  ( -13.04681709000290013, -15.30929823114697541, -1.500000000000002220 ) ) ;
#6913 = CARTESIAN_POINT ( 'NONE',  ( -88.62287095715004170, -23.48783264082479150, -1.443836473390063935 ) ) ;
#6914 = ORIENTED_EDGE ( 'NONE', *, *, #53735, .F. ) ;
#6915 = EDGE_CURVE ( 'NONE', #11149, #77509, #66599, .T. ) ;
#6917 = B_SPLINE_CURVE_WITH_KNOTS ( 'NONE', 3,
 ( #98842, #23719, #45080, #6508 ),
 .UNSPECIFIED., .F., .F.,
 ( 4, 4 ),
 ( 1.173777234769030585E-05, 0.001966071429883386491 ),
 .UNSPECIFIED. ) ;
#6916 = CARTESIAN_POINT ( 'NONE',  ( -40.25541618970063240, -25.30507957132854102, 5.538673484309292405 ) ) ;
#6918 = CARTESIAN_POINT ( 'NONE',  ( 21.44611857939883137, 6.294191480875499067, -1.500000000000002220 ) ) ;
#6919 = EDGE_LOOP ( 'NONE', ( #23829, #62040, #57181, #18603 ) ) ;
#6920 = ORIENTED_EDGE ( 'NONE', *, *, #78393, .F. ) ;
#6921 = CARTESIAN_POINT ( 'NONE',  ( -101.5363578631102541, -25.16257311046121714, 6.270899588959630400 ) ) ;
#6922 = CARTESIAN_POINT ( 'NONE',  ( -81.85688277028242510, -25.21766921460215016, 6.464279381724344908 ) ) ;
#6923 = DIRECTION ( 'NONE',  ( -3.773278334453079030E-23, 0.9999999999976377785, 2.173523156925979128E-06 ) ) ;
#6924 = EDGE_CURVE ( 'NONE', #14228, #75250, #21865, .T. ) ;
#6925 = DIRECTION ( 'NONE',  ( 0.000000000000000000, 0.000000000000000000, -1.000000000000000000 ) ) ;
#6926 = EDGE_CURVE ( 'NONE', #80766, #2778, #82287, .T. ) ;
#6927 = LINE ( 'NONE', #61236, #47217 ) ;
#6928 = CARTESIAN_POINT ( 'NONE',  ( 14.87128047407919951, 12.67365258641725312, 11.49999999999998934 ) ) ;
#6929 = VECTOR ( 'NONE', #99030, 1000.000000000000000 ) ;
#6930 = DIRECTION ( 'NONE',  ( -0.8246584009594636333, 0.000000000000000000, -0.5656310827093756766 ) ) ;
#6931 = EDGE_CURVE ( 'NONE', #42578, #75743, #44731, .T. ) ;
#6932 = CARTESIAN_POINT ( 'NONE',  ( -16.43003769262999469, -13.82051474754189258, -1.500000000000002220 ) ) ;
#6933 = CARTESIAN_POINT ( 'NONE',  ( -25.74893805332498076, -24.57999845255926985, 3.231002331236078717 ) ) ;
#6934 = CARTESIAN_POINT ( 'NONE',  ( -107.5228709571500758, -29.50247984919015209, -1.443849546365048253 ) ) ;
#6935 = CARTESIAN_POINT ( 'NONE',  ( -47.62287095715004881, -23.47593901973091235, -1.443836447539009749 ) ) ;
#6936 = CARTESIAN_POINT ( 'NONE',  ( -14.01358469492184966, -18.07645309290061064, -1.500000000000002220 ) ) ;
#6937 = APPLICATION_PROTOCOL_DEFINITION ( 'international standard', 'config_control_design', 1994, #23272 ) ;
#6938 = LINE ( 'NONE', #92664, #1324 ) ;
#6939 = CARTESIAN_POINT ( 'NONE',  ( -108.5228709571500900, -24.34917612407030063, 0.1852690917476662869 ) ) ;
#6940 = CARTESIAN_POINT ( 'NONE',  ( 6.088051586893210576, -19.00464151315268424, 11.49999999999999645 ) ) ;
#6941 = PLANE ( 'NONE',  #90579 ) ;
#6942 = DIRECTION ( 'NONE',  ( 1.000000000000000000, 0.000000000000000000, 0.000000000000000000 ) ) ;
#6943 = CARTESIAN_POINT ( 'NONE',  ( 33.10875634548599322, 6.475225279485573360, -11.42349945801155719 ) ) ;
#6944 = VERTEX_POINT ( 'NONE', #12763 ) ;
#6945 = CARTESIAN_POINT ( 'NONE',  ( -27.24283614821936439, -24.59459705238057836, 1.681040237769488854 ) ) ;
#6946 = EDGE_CURVE ( 'NONE', #78995, #74863, #38103, .T. ) ;
#6947 = CARTESIAN_POINT ( 'NONE',  ( -96.52287095715010423, -23.48783264082477018, -1.443836473390086139 ) ) ;
#6948 = CARTESIAN_POINT ( 'NONE',  ( 16.02445091669267185, 14.69945503153335764, -1.500000000000002220 ) ) ;
#6949 = CARTESIAN_POINT ( 'NONE',  ( -56.62287095715008434, -24.35013146730203815, 9.818937971375106599 ) ) ;
#6950 = CARTESIAN_POINT ( 'NONE',  ( -18.73025074496528219, 5.678645368852136777, -1.500000000000002220 ) ) ;
#6951 = CARTESIAN_POINT ( 'NONE',  ( -61.52287095715006160, -29.50247984919015209, -1.443849546365056913 ) ) ;
#6952 = CIRCLE ( 'NONE', #29689, 1.249999999999997558 ) ;
#6953 = ADVANCED_FACE ( 'NONE', ( #7151 ), #45233, .T. ) ;
#6954 = B_SPLINE_CURVE_WITH_KNOTS ( 'NONE', 3,
 ( #69498, #100414, #75587, #7089 ),
 .UNSPECIFIED., .F., .F.,
 ( 4, 4 ),
 ( 0.000000000000000000, 9.999999999998900014E-05 ),
 .UNSPECIFIED. ) ;
#6955 = CALENDAR_DATE ( 2026, 9, 10 ) ;
#6956 = LOCAL_TIME ( 0, 54, 15.00000000000000000, #61262 ) ;
#6957 = CARTESIAN_POINT ( 'NONE',  ( -116.5228709571500616, -29.50248528299804818, 1.056150453629045360 ) ) ;
#6958 = LINE ( 'NONE', #22165, #97762 ) ;
#6959 = CARTESIAN_POINT ( 'NONE',  ( -16.48689143942861079, 12.14541645011370541, 11.49999999999999645 ) ) ;
#6960 = CARTESIAN_POINT ( 'NONE',  ( 30.61238849909758031, 3.934983946744459171, 27.21775687185679615 ) ) ;
#6961 = B_SPLINE_CURVE_WITH_KNOTS ( 'NONE', 3,
 ( #32783, #86068, #71859, #2348 ),
 .UNSPECIFIED., .F., .F.,
 ( 4, 4 ),
 ( 0.000000000000000000, 9.999999999998897304E-05 ),
 .UNSPECIFIED. ) ;
#6962 = ADVANCED_FACE ( 'NONE', ( #76156 ), #7675, .T. ) ;
#6963 = CARTESIAN_POINT ( 'NONE',  ( -37.52287095715006870, -29.50247984919015209, -1.443849546365060466 ) ) ;
#6964 = VECTOR ( 'NONE', #71993, 1000.000000000000000 ) ;
#6965 = ORIENTED_EDGE ( 'NONE', *, *, #78604, .T. ) ;
#6966 = FACE_OUTER_BOUND ( 'NONE', #8138, .T. ) ;
#6967 = DIRECTION ( 'NONE',  ( -0.000000000000000000, 1.000000000000000000, 0.000000000000000000 ) ) ;
#6968 = FACE_OUTER_BOUND ( 'NONE', #59418, .T. ) ;
#6969 = CARTESIAN_POINT ( 'NONE',  ( 14.61581676223891613, -3.316774720514426900, -27.35847991879931485 ) ) ;
#6970 = VECTOR ( 'NONE', #88293, 1000.000000000000114 ) ;
#6971 = CARTESIAN_POINT ( 'NONE',  ( 17.91726403014145319, -0.5000000000000000000, -1.691563534834430227 ) ) ;
#6972 = DIRECTION ( 'NONE',  ( 0.000000000000000000, 2.173523156925980399E-06, -0.9999999999976378895 ) ) ;
#6973 = EDGE_CURVE ( 'NONE', #99016, #51651, #52376, .T. ) ;
#6974 = CARTESIAN_POINT ( 'NONE',  ( 10.19088217375349892, 20.72639945755932800, 11.49999999999999645 ) ) ;
#6975 = CARTESIAN_POINT ( 'NONE',  ( 9.312063170398973355, -20.82641193498425025, 11.49999999999998934 ) ) ;
#6976 = CARTESIAN_POINT ( 'NONE',  ( -109.6228709571500559, -24.64965695001469115, 8.947790433994176951 ) ) ;
#6977 = B_SPLINE_SURFACE_WITH_KNOTS ( 'NONE', 3, 1, ( 
 ( #17061, #55647 ),
 ( #30793, #15061 ),
 ( #46030, #77942 ),
 ( #46520, #16550 ),
 ( #94180, #77448 ),
 ( #32291, #69860 ),
 ( #61261, #70357 ),
 ( #85073, #7445 ),
 ( #23157, #48028 ),
 ( #47527, #62765 ),
 ( #54150, #38401 ),
 ( #78953, #78450 ),
 ( #63261, #23666 ),
 ( #31286, #61760 ),
 ( #62254, #38902 ) ),
 .UNSPECIFIED., .F., .F., .F.,
 ( 4, 1, 1, 1, 1, 1, 1, 1, 1, 1, 1, 1, 4 ),
 ( 2, 2 ),
 ( 0.000000000000000000, 0.1108026438013187259, 0.2128292023477701411, 0.3061013098231112339, 0.3906473211160097492, 0.4669244693608501917, 0.5344810392840317892, 0.5935869409656733264, 0.6445570045087155586, 0.7362004526293723927, 0.8250240256188635657, 0.9119855848297575562, 1.000000000000000000 ),
 ( 0.000000000000000000, 1.000000000000000000 ),
 .UNSPECIFIED. ) ;
#6978 = DIRECTION ( 'NONE',  ( 1.000000000000000000, 0.000000000000000000, 0.000000000000000000 ) ) ;
#6979 = CARTESIAN_POINT ( 'NONE',  ( 13.91401389203221406, -3.316774720514426456, 28.26920385068457264 ) ) ;
#6980 = DIRECTION ( 'NONE',  ( 3.773278334444167608E-23, -1.000000000000000000, 0.000000000000000000 ) ) ;
#6981 = CARTESIAN_POINT ( 'NONE',  ( -8.499999999999987566, 18.74999999999999645, 2.100000000000000089 ) ) ;
#6982 = EDGE_CURVE ( 'NONE', #38959, #18132, #82781, .T. ) ;
#6983 = CARTESIAN_POINT ( 'NONE',  ( -8.322136096487577461, -20.27582920440508829, -1.500000000000002220 ) ) ;
#6984 = CARTESIAN_POINT ( 'NONE',  ( -5.205649524681222218, -5.876774720514406525, 19.16400979764067714 ) ) ;
#6985 = CARTESIAN_POINT ( 'NONE',  ( -109.6228709571500417, -24.65952944569305316, 1.056160979905704345 ) ) ;
#6986 = CARTESIAN_POINT ( 'NONE',  ( 10.95759398273795249, 4.132774720514426292, -26.86884997114579932 ) ) ;
#6987 = CARTESIAN_POINT ( 'NONE',  ( -78.63771738212270179, -23.96119346886880308, -0.6495511937832113558 ) ) ;
#6988 = CARTESIAN_POINT ( 'NONE',  ( -117.6228709571500559, -24.64898659630368627, 1.056161002820833028 ) ) ;
#6989 = VERTEX_POINT ( 'NONE', #75168 ) ;
#6990 = CARTESIAN_POINT ( 'NONE',  ( 18.81987132735423174, -8.002443037797982939, -1.500000000000002220 ) ) ;
#6991 =( BOUNDED_SURFACE ( )  B_SPLINE_SURFACE ( 3, 2, ( 
 ( #94402, #40122, #78159 ),
 ( #79173, #24388, #31498 ),
 ( #71580, #53850, #552 ),
 ( #54855, #40628, #62976 ),
 ( #55863, #8672, #9672 ),
 ( #30997, #61965, #85283 ),
 ( #1569, #86787, #38613 ),
 ( #85794, #39613, #17280 ),
 ( #2075, #69573, #47739 ),
 ( #33013, #15771, #62461 ),
 ( #63988, #46737, #84781 ),
 ( #77661, #15268, #8168 ),
 ( #46227, #70064, #16275 ),
 ( #1062, #77161, #70565 ),
 ( #93391, #93899, #7664 ),
 ( #39109, #23880, #55356 ) ),
 .UNSPECIFIED., .F., .F., .T. ) 
 B_SPLINE_SURFACE_WITH_KNOTS ( ( 4, 2, 2, 2, 2, 2, 2, 4 ),
 ( 3, 3 ),
 ( 5.963111948670274387E-19, 0.0002402527847056124086, 0.0004805055694112242209, 0.0007207583541168360603, 0.0009610111388224478997, 0.001201263923528059739, 0.001441516708233671470, 0.001922022277644895149 ),
 ( 0.000000000000000000, 1.000000000000000000 ),
 .UNSPECIFIED. ) 
 GEOMETRIC_REPRESENTATION_ITEM ( )  RATIONAL_B_SPLINE_SURFACE ( (
 ( 1.000000000000000000, 0.6532382444175202085, 1.000000000000000000),
 ( 1.000000000000000000, 0.6532394276814369460, 1.000000000000000000),
 ( 1.000000000000000000, 0.6536213453767286685, 1.000000000000000000),
 ( 1.000000000000000000, 0.6551141999105375424, 1.000000000000000000),
 ( 1.000000000000000000, 0.6562426621441458385, 1.000000000000000000),
 ( 1.000000000000000000, 0.6591574828660696772, 1.000000000000000000),
 ( 1.000000000000000000, 0.6609310395923536641, 1.000000000000000000),
 ( 1.000000000000000000, 0.6650742797341039347, 1.000000000000000000),
 ( 1.000000000000000000, 0.6674600455424170020, 1.000000000000000000),
 ( 1.000000000000000000, 0.6725980719960679144, 1.000000000000000000),
 ( 1.000000000000000000, 0.6753708636379929242, 1.000000000000000000),
 ( 1.000000000000000000, 0.6813027919944147914, 1.000000000000000000),
 ( 1.000000000000000000, 0.6844015431888567091, 1.000000000000000000),
 ( 1.000000000000000000, 0.6938890553659712301, 1.000000000000000000),
 ( 1.000000000000000000, 0.7006220437376852184, 1.000000000000000000),
 ( 1.000000000000000000, 0.7071067811865475727, 1.000000000000000000) ) ) 
 REPRESENTATION_ITEM ( '' )  SURFACE ( )  );
#6992 = ORIENTED_EDGE ( 'NONE', *, *, #2471, .T. ) ;
#6993 = ORIENTED_EDGE ( 'NONE', *, *, #54265, .T. ) ;
#6994 = ORIENTED_EDGE ( 'NONE', *, *, #57239, .T. ) ;
#6995 = ORIENTED_EDGE ( 'NONE', *, *, #37008, .T. ) ;
#6996 = CARTESIAN_POINT ( 'NONE',  ( 1.912052097559287844, -22.98750448113701239, 11.49999999999998934 ) ) ;
#6997 = CARTESIAN_POINT ( 'NONE',  ( -61.50413361299347770, -24.15543982623907127, -0.2315651400026656481 ) ) ;
#6998 = CARTESIAN_POINT ( 'NONE',  ( -6.993686169601437186, 18.98418669460116348, -1.500000000000002220 ) ) ;
#6999 = VECTOR ( 'NONE', #87776, 1000.000000000000000 ) ;
#7000 = ORIENTED_EDGE ( 'NONE', *, *, #71475, .T. ) ;
#7001 = CARTESIAN_POINT ( 'NONE',  ( -54.52287095715006870, -24.64965694238575011, 8.947790433994203596 ) ) ;
#7002 = CARTESIAN_POINT ( 'NONE',  ( 5.097264368844747651, -3.299463065352477908, -27.56135813788838718 ) ) ;
#7003 = CARTESIAN_POINT ( 'NONE',  ( 32.98733314340959311, 0.3587747205144265483, 2.074222136288530027 ) ) ;
#7004 = CARTESIAN_POINT ( 'NONE',  ( -70.50072534953635284, -24.40034930558990922, 0.3402023900116040167 ) ) ;
#7006 = ORIENTED_EDGE ( 'NONE', *, *, #93536, .T. ) ;
#7005 = CARTESIAN_POINT ( 'NONE',  ( 2.695732861974529104, -21.29187259674557708, 11.49999999999999645 ) ) ;
#7007 = CARTESIAN_POINT ( 'NONE',  ( -113.6228709571500559, -23.94994826722516379, -0.6494450866351674234 ) ) ;
#7009 = AXIS2_PLACEMENT_3D ( 'NONE', #25558, #95073, #39275 ) ;
#7008 = CARTESIAN_POINT ( 'NONE',  ( -110.6228709571500559, -23.47593901973091235, -1.443836447538999312 ) ) ;
#7010 = EDGE_LOOP ( 'NONE', ( #35681, #93467, #99571, #93739 ) ) ;
#7011 = CARTESIAN_POINT ( 'NONE',  ( 16.32338804990218151, -12.73490195939593406, 11.49999999999998934 ) ) ;
#7012 = ORIENTED_EDGE ( 'NONE', *, *, #33342, .T. ) ;
#7014 = ORIENTED_EDGE ( 'NONE', *, *, #94197, .T. ) ;
#7013 = FACE_OUTER_BOUND ( 'NONE', #65807, .T. ) ;
#7015 = CARTESIAN_POINT ( 'NONE',  ( 15.32643653063177958, -3.577630190450218350, -27.14485409495429380 ) ) ;
#7016 = VERTEX_POINT ( 'NONE', #59967 ) ;
#7017 = CARTESIAN_POINT ( 'NONE',  ( 4.948119756536996761, -5.876774720514408301, 19.52858994054604125 ) ) ;
#7018 = B_SPLINE_CURVE_WITH_KNOTS ( 'NONE', 3,
 ( #16194, #77584, #7087, #30423, #38038, #68989 ),
 .UNSPECIFIED., .F., .F.,
 ( 4, 2, 4 ),
 ( 0.000000000000000000, 0.001380901958385390062, 0.002761803916770780125 ),
 .UNSPECIFIED. ) ;
#7019 = CARTESIAN_POINT ( 'NONE',  ( -102.5228709571500758, -23.47596703998600631, 11.44779298504228215 ) ) ;
#7020 = CARTESIAN_POINT ( 'NONE',  ( 7.969717912702302343, -20.46423023992739942, 11.49999999999999645 ) ) ;
#7021 = CARTESIAN_POINT ( 'NONE',  ( -89.55819837874346945, -23.73791477778911840, 11.05961554403170410 ) ) ;
#7022 = CARTESIAN_POINT ( 'NONE',  ( 21.78986343443989071, 5.811249688775594002, 11.49999999999998934 ) ) ;
#7023 = CARTESIAN_POINT ( 'NONE',  ( -7.180602670292889123, -19.69607742855361465, -1.500000000000002220 ) ) ;
#7024 = CARTESIAN_POINT ( 'NONE',  ( -109.0053741199720747, -25.30783060902023252, 4.561566455935911257 ) ) ;
#7025 = VECTOR ( 'NONE', #57656, 1000.000000000000114 ) ;
#7026 = DIRECTION ( 'NONE',  ( 1.000000000000000000, 0.000000000000000000, 0.000000000000000000 ) ) ;
#7027 = ORIENTED_EDGE ( 'NONE', *, *, #95038, .T. ) ;
#7028 = ORIENTED_EDGE ( 'NONE', *, *, #34887, .T. ) ;
#7029 = ORIENTED_EDGE ( 'NONE', *, *, #66075, .F. ) ;
#7030 = CARTESIAN_POINT ( 'NONE',  ( -36.62287095715006302, -24.51283580621364067, 0.6167428607019720399 ) ) ;
#7031 = CARTESIAN_POINT ( 'NONE',  ( 13.13055478438326773, -17.03443908202477886, -1.500000000000002220 ) ) ;
#7032 = VECTOR ( 'NONE', #19060, 1000.000000000000000 ) ;
#7033 = CARTESIAN_POINT ( 'NONE',  ( -90.62287095715001328, -24.14406661707770851, 10.28769366152061870 ) ) ;
#7034 = ORIENTED_EDGE ( 'NONE', *, *, #93418, .T. ) ;
#7035 = CARTESIAN_POINT ( 'NONE',  ( -16.97324839047195866, 12.58421825509937442, 11.49999999999998934 ) ) ;
#7036 = DIRECTION ( 'NONE',  ( 1.000000000000000000, -0.000000000000000000, 0.000000000000000000 ) ) ;
#7037 = ADVANCED_FACE ( 'NONE', ( #5658 ), #98494, .T. ) ;
#7038 = CARTESIAN_POINT ( 'NONE',  ( -64.62365164054095601, -24.65952944569304250, 1.056160979905695685 ) ) ;
#7039 = CARTESIAN_POINT ( 'NONE',  ( -50.33479198164290125, -25.30263672226421079, 4.734682818538147764 ) ) ;
#7040 = CARTESIAN_POINT ( 'NONE',  ( 14.76093561896379214, 5.965225279485572685, -28.39148769130089889 ) ) ;
#7041 = CARTESIAN_POINT ( 'NONE',  ( -123.5895376238167387, -23.48783264082478794, -1.443836473390058606 ) ) ;
#7042 = CARTESIAN_POINT ( 'NONE',  ( 12.08182546098005972, -18.57710416600862402, -1.500000000000002220 ) ) ;
#7043 = ADVANCED_FACE ( 'NONE', ( #86283 ), #70559, .F. ) ;
#7044 = FACE_OUTER_BOUND ( 'NONE', #16373, .T. ) ;
#7045 = EDGE_CURVE ( 'NONE', #20245, #58804, #35026, .T. ) ;
#7046 = ORIENTED_EDGE ( 'NONE', *, *, #85647, .F. ) ;
#7047 = FACE_OUTER_BOUND ( 'NONE', #86258, .T. ) ;
#7048 = CARTESIAN_POINT ( 'NONE',  ( 32.66876533700883556, -5.965225279485572685, -12.58926540598386445 ) ) ;
#7049 = DIRECTION ( 'NONE',  ( 0.000000000000000000, -0.9999999999976377785, -2.173523156925979975E-06 ) ) ;
#7050 = ADVANCED_FACE ( 'NONE', ( #47733 ), #54847, .T. ) ;
#7051 = LINE ( 'NONE', #75050, #38188 ) ;
#7052 = CARTESIAN_POINT ( 'NONE',  ( 1.255614643274026276, -19.41590359075080841, 11.49999999999998934 ) ) ;
#7053 = CARTESIAN_POINT ( 'NONE',  ( 2.027878592902508270, 21.29203748114955985, -1.500000000000002220 ) ) ;
#7054 = CARTESIAN_POINT ( 'NONE',  ( -62.49105905257930260, -24.65952944569303895, 1.056160979905693686 ) ) ;
#7055 = DIRECTION ( 'NONE',  ( -0.000000000000000000, -0.9513357669802769978, 0.3081562241202474572 ) ) ;
#7056 = CARTESIAN_POINT ( 'NONE',  ( -27.96875734969026084, -3.316774720514426456, 23.50402280011861933 ) ) ;
#7057 = CARTESIAN_POINT ( 'NONE',  ( -109.5228709571500616, -29.50247984919015209, -1.443849546365048253 ) ) ;
#7058 = CARTESIAN_POINT ( 'NONE',  ( 1.118074629359579797, -22.68859683979520980, -1.500000000000002220 ) ) ;
#7059 = B_SPLINE_SURFACE_WITH_KNOTS ( 'NONE', 3, 3, ( 
 ( #24702, #72401, #31831, #86110 ),
 ( #17602, #88123, #9986, #25205 ),
 ( #33825, #56183, #2895, #64812 ),
 ( #49566, #16587, #26216, #18590 ),
 ( #47564, #55682, #80497, #78485 ),
 ( #8984, #70899, #86610, #1390 ),
 ( #17097, #36327, #72901, #5374 ) ),
 .UNSPECIFIED., .F., .F., .F.,
 ( 4, 3, 4 ),
 ( 4, 4 ),
 ( 0.7945040050992242531, 0.8970133687736503436, 0.9995227324480764342 ),
 ( 0.8197022949557353222, 0.8210934484848215753 ),
 .UNSPECIFIED. ) ;
#7060 = EDGE_CURVE ( 'NONE', #1645, #44267, #48801, .T. ) ;
#7061 = ORIENTED_EDGE ( 'NONE', *, *, #13673, .T. ) ;
#7062 = CARTESIAN_POINT ( 'NONE',  ( -87.52287095715006160, -24.66019654487200086, 8.947790411086115725 ) ) ;
#7063 = DIRECTION ( 'NONE',  ( 0.000000000000000000, 0.000000000000000000, -1.000000000000000000 ) ) ;
#7064 = CARTESIAN_POINT ( 'NONE',  ( 2.545096341412688812, 19.61957628810408849, 11.49999999999999645 ) ) ;
#7065 = DIRECTION ( 'NONE',  ( 3.773278334444166432E-23, -1.000000000000000000, 0.000000000000000000 ) ) ;
#7066 = VERTEX_POINT ( 'NONE', #85274 ) ;
#7067 = CARTESIAN_POINT ( 'NONE',  ( -59.52287095715004028, -23.94994826722564696, -0.6494450866342711404 ) ) ;
#7068 = VECTOR ( 'NONE', #47102, 1000.000000000000000 ) ;
#7069 = CARTESIAN_POINT ( 'NONE',  ( -61.64687923781919210, -25.21083105912962452, 3.409327675794633361 ) ) ;
#7070 = CARTESIAN_POINT ( 'NONE',  ( 14.58690015069645263, 15.99052346098381250, 11.49999999999998934 ) ) ;
#7071 = CARTESIAN_POINT ( 'NONE',  ( 2.750000000000001332, 27.59999999999999432, 0.000000000000000000 ) ) ;
#7072 = CARTESIAN_POINT ( 'NONE',  ( -16.37229413335033001, -10.43475415037859655, -1.500000000000002220 ) ) ;
#7073 = CARTESIAN_POINT ( 'NONE',  ( -129.6228709571500133, -23.73934037231757799, 11.05740245334328087 ) ) ;
#7074 = CARTESIAN_POINT ( 'NONE',  ( -40.58953762381671737, -24.99156044556120193, 7.747789690856344613 ) ) ;
#7075 = CARTESIAN_POINT ( 'NONE',  ( 18.95923836289803788, 5.684714004613049987, 11.49999999999998934 ) ) ;
#7076 = B_SPLINE_CURVE_WITH_KNOTS ( 'NONE', 3,
 ( #26179, #73856, #11949, #89082 ),
 .UNSPECIFIED., .F., .F.,
 ( 4, 4 ),
 ( 2.613633516198037533E-05, 0.004366793516964704441 ),
 .UNSPECIFIED. ) ;
#7077 = VERTEX_POINT ( 'NONE', #15264 ) ;
#7078 = AXIS2_PLACEMENT_3D ( 'NONE', #47787, #9206, #40168 ) ;
#7079 = CARTESIAN_POINT ( 'NONE',  ( -12.25758032491116367, 16.21837406056298292, 11.49999999999999645 ) ) ;
#7080 = FACE_OUTER_BOUND ( 'NONE', #74906, .T. ) ;
#7081 = CARTESIAN_POINT ( 'NONE',  ( -46.52287095715004028, -24.66019654487199375, 8.947790411086122830 ) ) ;
#7082 = ORIENTED_EDGE ( 'NONE', *, *, #57484, .F. ) ;
#7083 = CARTESIAN_POINT ( 'NONE',  ( -30.60515864328932878, -24.57438384523503672, 0.5319095616429414530 ) ) ;
#7084 = CARTESIAN_POINT ( 'NONE',  ( -116.4728709594060092, -25.21147767946276019, 8.000950762517433645 ) ) ;
#7085 = CARTESIAN_POINT ( 'NONE',  ( -48.87464133331025806, -25.31602070427312867, 6.106124868286230800 ) ) ;
#7086 = CARTESIAN_POINT ( 'NONE',  ( -40.48178299873823960, -24.63419186844611630, 9.035850630976923981 ) ) ;
#7087 = CARTESIAN_POINT ( 'NONE',  ( -127.6228709571500559, -23.95044443724992078, 10.65354141964649415 ) ) ;
#7088 = CARTESIAN_POINT ( 'NONE',  ( -18.95788008782500356, -6.583919088883305015, 11.49999999999998934 ) ) ;
#7089 = CARTESIAN_POINT ( 'NONE',  ( -95.52287095715006160, -24.99132157543166954, 2.256160258750667502 ) ) ;
#7090 = EDGE_LOOP ( 'NONE', ( #23115, #21331, #372, #53139 ) ) ;
#7091 = DIRECTION ( 'NONE',  ( 0.000000000000000000, -1.000000000000000000, 0.000000000000000000 ) ) ;
#7092 = EDGE_CURVE ( 'NONE', #5624, #22977, #78150, .T. ) ;
#7093 = B_SPLINE_CURVE_WITH_KNOTS ( 'NONE', 3,
 ( #97043, #51877, #83304, #89930, #8067, #36148, #50881, #5687 ),
 .UNSPECIFIED., .F., .F.,
 ( 4, 2, 2, 4 ),
 ( 0.000000000000000000, 0.002001098010032677579, 0.003001647015049018104, 0.004002196020065359496 ),
 .UNSPECIFIED. ) ;
#7094 = CARTESIAN_POINT ( 'NONE',  ( -22.64140897529919272, -3.284158816904186651, 11.49999999999999645 ) ) ;
#7095 = CARTESIAN_POINT ( 'NONE',  ( -5.793434319722853054, -21.96748078227757617, 11.49999999999998934 ) ) ;
#7096 = CARTESIAN_POINT ( 'NONE',  ( -49.94769165354211538, -25.31297195507654507, 4.634772910520919886 ) ) ;
#7097 = CARTESIAN_POINT ( 'NONE',  ( -50.62287095715005592, -23.47596703998600631, 11.44779298504227505 ) ) ;
#7098 = CARTESIAN_POINT ( 'NONE',  ( -38.66565014046062032, -23.48786465467240347, 11.44779295918255002 ) ) ;
#7099 = CARTESIAN_POINT ( 'NONE',  ( 6.377880655330028681, -5.876774720514424288, 21.48000012937543346 ) ) ;
#7100 = EDGE_CURVE ( 'NONE', #61887, #10751, #35498, .T. ) ;
#7101 = CARTESIAN_POINT ( 'NONE',  ( -128.5556214221262223, -24.35071581493544102, 9.817618358456019934 ) ) ;
#7102 = AXIS2_PLACEMENT_3D ( 'NONE', #46134, #98902, #100385 ) ;
#7103 = CARTESIAN_POINT ( 'NONE',  ( 0.000000000000000000, 5.356774720514425603, 0.000000000000000000 ) ) ;
#7104 = VERTEX_POINT ( 'NONE', #23872 ) ;
#7105 = CARTESIAN_POINT ( 'NONE',  ( 19.36038471569032993, -6.267470172042458820, 11.49999999999998934 ) ) ;
#7106 = AXIS2_PLACEMENT_3D ( 'NONE', #42648, #33516, #65995 ) ;
#7107 = ORIENTED_EDGE ( 'NONE', *, *, #37970, .F. ) ;
#7108 = CARTESIAN_POINT ( 'NONE',  ( -21.75629724252761577, 7.406401271465676395, 11.49999999999998934 ) ) ;
#7109 = CARTESIAN_POINT ( 'NONE',  ( -32.47729921221014138, -24.65952944569304606, 1.056160979905696351 ) ) ;
#7110 = EDGE_LOOP ( 'NONE', ( #95330, #98715, #97541, #67051 ) ) ;
#7111 = DIRECTION ( 'NONE',  ( 1.000000000000000000, -0.000000000000000000, 0.000000000000000000 ) ) ;
#7112 = CARTESIAN_POINT ( 'NONE',  ( -94.58953762381672448, -23.48783264082478794, -1.443836473390063491 ) ) ;
#7113 = CARTESIAN_POINT ( 'NONE',  ( 0.02224039135773590858, 0.3828044741864786715, 0.3828044741864790046 ) ) ;
#7115 = EDGE_LOOP ( 'NONE', ( #83697, #23480, #62003, #60217 ) ) ;
#7114 = CARTESIAN_POINT ( 'NONE',  ( -19.44786352930952233, -8.617208915446557427, 11.49999999999999645 ) ) ;
#7116 = ORIENTED_EDGE ( 'NONE', *, *, #20946, .F. ) ;
#7117 = CARTESIAN_POINT ( 'NONE',  ( 21.18294168759468832, 6.642818831845659133, 11.49999999999998934 ) ) ;
#7118 = CARTESIAN_POINT ( 'NONE',  ( -18.09956831669839872, 9.893135806712603397, 11.49999999999998934 ) ) ;
#7119 = ORIENTED_EDGE ( 'NONE', *, *, #78191, .F. ) ;
#7120 = ORIENTED_EDGE ( 'NONE', *, *, #31626, .T. ) ;
#7121 = CARTESIAN_POINT ( 'NONE',  ( -109.1250679552890830, -25.27682725309280087, 4.858945224259093365 ) ) ;
#7122 = DIRECTION ( 'NONE',  ( 0.000000000000000000, -1.000000000000000000, 0.000000000000000000 ) ) ;
#7123 = VERTEX_POINT ( 'NONE', #31997 ) ;
#7124 = CARTESIAN_POINT ( 'NONE',  ( -49.74249510286006171, -25.16055632220097138, 6.938864448453002431 ) ) ;
#7125 = ORIENTED_EDGE ( 'NONE', *, *, #92475, .F. ) ;
#7126 = CARTESIAN_POINT ( 'NONE',  ( -39.52287095715006160, -24.50321055353803956, 9.387540953477529371 ) ) ;
#7127 = CARTESIAN_POINT ( 'NONE',  ( -35.62287095715005592, -23.48786465467240347, 11.44779295918255180 ) ) ;
#7128 = CARTESIAN_POINT ( 'NONE',  ( 18.76864855846692492, -9.085702381504452418, -1.500000000000002220 ) ) ;
#7129 = CARTESIAN_POINT ( 'NONE',  ( -19.23829340896090656, 10.21096329589227025, 11.49999999999999645 ) ) ;
#7130 = TOROIDAL_SURFACE ( 'NONE', #34672, 1.049999999999998934, 0.5999999999999999778 ) ;
#7131 = CARTESIAN_POINT ( 'NONE',  ( -100.5372941577377617, -25.18545306133426465, 3.297626459260741161 ) ) ;
#7132 = CARTESIAN_POINT ( 'NONE',  ( -78.52212882731420507, -23.48786465467241058, 11.44779295918254469 ) ) ;
#7133 = CARTESIAN_POINT ( 'NONE',  ( 21.16529133594374557, -7.503415950508986576, -1.500000000000002220 ) ) ;
#7134 = CARTESIAN_POINT ( 'NONE',  ( -43.62287095715004881, -24.66019654487199020, 8.947790411086135265 ) ) ;
#7135 = EDGE_CURVE ( 'NONE', #66209, #98373, #22858, .T. ) ;
#7136 = EDGE_LOOP ( 'NONE', ( #20316, #63931, #70856, #50141 ) ) ;
#7137 = LINE ( 'NONE', #38087, #100371 ) ;
#7138 = CARTESIAN_POINT ( 'NONE',  ( -101.8161100070499572, -25.24282061761980955, 6.236250683194342059 ) ) ;
#7139 = B_SPLINE_CURVE_WITH_KNOTS ( 'NONE', 3,
 ( #61006, #75704, #98542, #30031, #60015, #91940, #84321, #91430 ),
 .UNSPECIFIED., .F., .F.,
 ( 4, 2, 2, 4 ),
 ( -0.001224554619866340642, -0.0002241820295893614135, 0.0007761905606876178150, 0.002776935741241576272 ),
 .UNSPECIFIED. ) ;
#7140 = VERTEX_POINT ( 'NONE', #46730 ) ;
#7141 = VERTEX_POINT ( 'NONE', #8665 ) ;
#7142 = ORIENTED_EDGE ( 'NONE', *, *, #35331, .T. ) ;
#7143 = CARTESIAN_POINT ( 'NONE',  ( -21.34312709018487553, 1.176582458498846462, -1.500000000000002220 ) ) ;
#7144 = ORIENTED_EDGE ( 'NONE', *, *, #77814, .T. ) ;
#7145 = CARTESIAN_POINT ( 'NONE',  ( -19.96636262075925927, 6.592627302904066511, -1.500000000000002220 ) ) ;
#7146 = CARTESIAN_POINT ( 'NONE',  ( -30.58285789377789499, -25.15082570009304064, 2.712646531854225440 ) ) ;
#7147 = ADVANCED_FACE ( 'NONE', ( #8163 ), #62967, .F. ) ;
#7148 = CARTESIAN_POINT ( 'NONE',  ( -99.91491574289003097, -25.20057459230137198, 3.406812263743608682 ) ) ;
#7149 = CARTESIAN_POINT ( 'NONE',  ( 9.566520649354789185, -3.316774720514426011, -27.03026789950428110 ) ) ;
#7150 = CARTESIAN_POINT ( 'NONE',  ( 14.26656746985186608, 16.74056184347216458, -1.500000000000002220 ) ) ;
#7151 = FACE_OUTER_BOUND ( 'NONE', #87779, .T. ) ;
#7152 = ORIENTED_EDGE ( 'NONE', *, *, #54736, .T. ) ;
#7153 = PLANE ( 'NONE',  #56516 ) ;
#7154 = EDGE_CURVE ( 'NONE', #2401, #100041, #7623, .T. ) ;
#7155 = CARTESIAN_POINT ( 'NONE',  ( -41.62287095715006302, -24.64965695001467694, 8.947790433994187609 ) ) ;
#7156 = ADVANCED_FACE ( 'NONE', ( #71072 ), #55855, .F. ) ;
#7157 = CARTESIAN_POINT ( 'NONE',  ( -84.52214524269466267, -23.48786465467241769, 11.44779295918254647 ) ) ;
#7158 = EDGE_CURVE ( 'NONE', #77786, #13179, #30622, .T. ) ;
#7159 = CARTESIAN_POINT ( 'NONE',  ( 2.246611357655420083, 0.1632191352058106337, 0.1632191352058112166 ) ) ;
#7160 = CARTESIAN_POINT ( 'NONE',  ( -30.60887394897559943, -24.57243507446463937, 9.174899246800711339 ) ) ;
#7161 = CARTESIAN_POINT ( 'NONE',  ( 6.557060941508195739, 20.25493142521265355, -1.500000000000002220 ) ) ;
#7162 = LINE ( 'NONE', #47744, #57998 ) ;
#7163 = EDGE_CURVE ( 'NONE', #63553, #32600, #2791, .T. ) ;
#7164 = CARTESIAN_POINT ( 'NONE',  ( -107.6280293522714260, -24.15620529776628800, 10.23563542870659759 ) ) ;
#7165 = CARTESIAN_POINT ( 'NONE',  ( -9.299999999999991829, 12.00000000000002309, 0.000000000000000000 ) ) ;
#7166 = CARTESIAN_POINT ( 'NONE',  ( -33.64272878514460530, -24.15543982623906771, -0.2315651400026580431 ) ) ;
#7167 = CARTESIAN_POINT ( 'NONE',  ( 8.356338879324495039, -20.90460381316865934, -1.500000000000002220 ) ) ;
#7168 = CARTESIAN_POINT ( 'NONE',  ( 2.449489742783178770, -1.473225279485573358, 2.499999999999999556 ) ) ;
#7169 = ORIENTED_EDGE ( 'NONE', *, *, #81947, .F. ) ;
#7170 = CARTESIAN_POINT ( 'NONE',  ( -76.62287095715007013, -23.48786465467241058, 11.44779295918254469 ) ) ;
#7171 = CARTESIAN_POINT ( 'NONE',  ( -15.04504930077994196, -12.58455232801425794, 11.49999999999999645 ) ) ;
#7172 = CARTESIAN_POINT ( 'NONE',  ( -55.52287095715006870, -25.00182538069145011, 7.747789668545106423 ) ) ;
#7173 = DIRECTION ( 'NONE',  ( 0.000000000000000000, 0.000000000000000000, -1.000000000000000000 ) ) ;
#7174 = EDGE_CURVE ( 'NONE', #64559, #40372, #1028, .T. ) ;
#7175 = ORIENTED_EDGE ( 'NONE', *, *, #30050, .F. ) ;
#7176 = CARTESIAN_POINT ( 'NONE',  ( -88.50535495414969489, -24.51419770103157703, 9.386484678747176957 ) ) ;
#7177 = CARTESIAN_POINT ( 'NONE',  ( -126.8950052880273063, -25.34772655306150924, 6.200157639293698786 ) ) ;
#7178 = CARTESIAN_POINT ( 'NONE',  ( -100.3128489789178559, -25.31439539913989378, 5.229225532754338879 ) ) ;
#7179 = CARTESIAN_POINT ( 'NONE',  ( -6.756748142665309764, -18.51622224137248907, -1.500000000000002220 ) ) ;
#7180 = ORIENTED_EDGE ( 'NONE', *, *, #93757, .F. ) ;
#7181 = CARTESIAN_POINT ( 'NONE',  ( 6.783277369150963132, 3.316774720515097030, -28.31678455703255892 ) ) ;
#7182 = CARTESIAN_POINT ( 'NONE',  ( -66.62287095715005592, -29.50248528299804818, 1.056150453629036701 ) ) ;
#7183 = CIRCLE ( 'NONE', #80140, 130.2784398600581710 ) ;
#7184 = CALENDAR_DATE ( 2026, 9, 10 ) ;
#7185 = ORIENTED_EDGE ( 'NONE', *, *, #36612, .F. ) ;
#7186 = DIRECTION ( 'NONE',  ( 0.000000000000000000, -2.173523156925980399E-06, 0.9999999999976378895 ) ) ;
#7187 = CARTESIAN_POINT ( 'NONE',  ( -16.22218391600152643, -6.475225279485573360, -54.85883559227303863 ) ) ;
#7188 = CYLINDRICAL_SURFACE ( 'NONE', #70183, 1.699999999999999289 ) ;
#7189 = CARTESIAN_POINT ( 'NONE',  ( -29.49875734969025842, 5.965225279485572685, 25.61802280011862720 ) ) ;
#7190 = CARTESIAN_POINT ( 'NONE',  ( -86.62287095715004170, -29.50250243563736774, 8.947779886222139822 ) ) ;
#7191 = PLANE ( 'NONE',  #84577 ) ;
#7192 = CARTESIAN_POINT ( 'NONE',  ( 13.10664265030973930, 0.3587747205144256601, -28.64597719988137570 ) ) ;
#7193 = CARTESIAN_POINT ( 'NONE',  ( -14.92271332039470444, 13.28099397388983327, -1.500000000000002220 ) ) ;
#7194 = EDGE_CURVE ( 'NONE', #5494, #93024, #15867, .T. ) ;
#7195 = AXIS2_PLACEMENT_3D ( 'NONE', #94229, #31335, #55696 ) ;
#7196 = CARTESIAN_POINT ( 'NONE',  ( -100.3793702452611285, -25.10935038052450352, 2.834178115470032289 ) ) ;
#7197 = CARTESIAN_POINT ( 'NONE',  ( -51.57235953973243880, -25.30441124943957476, 4.474666492193762224 ) ) ;
#7198 = VERTEX_POINT ( 'NONE', #47712 ) ;
#7199 = ADVANCED_FACE ( 'NONE', ( #54828 ), #40600, .T. ) ;
#7200 = CARTESIAN_POINT ( 'NONE',  ( -119.5930743455675582, -23.48783264082477018, -1.443836473390087916 ) ) ;
#7201 = CARTESIAN_POINT ( 'NONE',  ( -80.54147481932388075, -24.73531770709095312, 8.716586749053508498 ) ) ;
#7202 = CARTESIAN_POINT ( 'NONE',  ( 29.73860345376319358, 5.356774720514428267, 17.72811383290910570 ) ) ;
#7203 = CARTESIAN_POINT ( 'NONE',  ( -108.5228709571500758, -23.72747288104470442, -1.053458166803225682 ) ) ;
#7204 = CARTESIAN_POINT ( 'NONE',  ( -28.41293738586069040, -24.60093919842945098, 1.764153402501565715 ) ) ;
#7205 = CARTESIAN_POINT ( 'NONE',  ( -1.380763273332680896, -6.376774720514418959, 20.28973052848695602 ) ) ;
#7206 = CYLINDRICAL_SURFACE ( 'NONE', #75452, 1.399999999999999911 ) ;
#7207 = EDGE_CURVE ( 'NONE', #66840, #16463, #31697, .T. ) ;
#7208 = CARTESIAN_POINT ( 'NONE',  ( 5.359050311451609261, -6.376774720514420736, 21.05346524168807676 ) ) ;
#7209 = ORIENTED_EDGE ( 'NONE', *, *, #78573, .F. ) ;
#7210 = CARTESIAN_POINT ( 'NONE',  ( -2.356373108420451334, 20.14613781377289214, 11.49999999999998934 ) ) ;
#7211 = CARTESIAN_POINT ( 'NONE',  ( -85.62287095715004170, -24.99132157543083821, 2.256160258750667502 ) ) ;
#7212 = ADVANCED_FACE ( 'NONE', ( #9134 ), #54328, .F. ) ;
#7213 = FACE_OUTER_BOUND ( 'NONE', #33224, .T. ) ;
#7214 = DIRECTION ( 'NONE',  ( 1.000000000000000000, 3.773278334444167608E-23, 8.201307833595939069E-29 ) ) ;
#7215 = VERTEX_POINT ( 'NONE', #39082 ) ;
#7216 = FACE_OUTER_BOUND ( 'NONE', #34924, .T. ) ;
#7217 = CARTESIAN_POINT ( 'NONE',  ( -20.11654390397962544, -0.4351469013266864860, -1.500000000000002220 ) ) ;
#7218 = CARTESIAN_POINT ( 'NONE',  ( 7.532573551308565207, 19.69859070278346991, 11.49999999999999645 ) ) ;
#7219 = VECTOR ( 'NONE', #13913, 1000.000000000000000 ) ;
#7220 = CARTESIAN_POINT ( 'NONE',  ( -32.52287095715006160, -24.65952944569304606, 1.056160979905690134 ) ) ;
#7221 = CARTESIAN_POINT ( 'NONE',  ( 7.643743511751816655, -20.74876368896106271, -1.500000000000002220 ) ) ;
#7223 = CARTESIAN_POINT ( 'NONE',  ( 19.85418835109896563, -5.301297255791479479, -1.500000000000002220 ) ) ;
#7222 = APPROVAL ( #24534, 'UNSPECIFIED' ) ;
#7224 = CARTESIAN_POINT ( 'NONE',  ( -35.52287095715006870, -24.99132157543083821, 2.256160258750667502 ) ) ;
#7225 = CARTESIAN_POINT ( 'NONE',  ( -126.6228709571500559, -24.64898659630529565, 1.056161002820834804 ) ) ;
#7226 = ORIENTED_EDGE ( 'NONE', *, *, #43174, .T. ) ;
#7227 = CYLINDRICAL_SURFACE ( 'NONE', #12005, 0.8160000000000007248 ) ;
#7228 = ORIENTED_EDGE ( 'NONE', *, *, #84407, .F. ) ;
#7229 = CARTESIAN_POINT ( 'NONE',  ( 9.150000000000003908, -5.876774720514426953, 11.88602120139451834 ) ) ;
#7230 = B_SPLINE_SURFACE_WITH_KNOTS ( 'NONE', 3, 3, ( 
 ( #99870, #54735, #54236, #53734 ),
 ( #69940, #84160, #22750, #428 ),
 ( #30377, #78034, #23759, #22250 ),
 ( #15152, #84664, #61349, #93270 ),
 ( #7543, #91768, #61847, #68449 ),
 ( #38990, #77541, #85669, #46620 ),
 ( #45616, #37497, #100365, #60850 ) ),
 .UNSPECIFIED., .F., .F., .F.,
 ( 4, 3, 4 ),
 ( 4, 4 ),
 ( 0.0004766839783818845044, 0.1029713700210894839, 0.2054660560637970868 ),
 ( 0.5896439926061133319, 0.5909287778169047822 ),
 .UNSPECIFIED. ) ;
#7231 = DIRECTION ( 'NONE',  ( 1.000000000000000000, 3.773278334444167608E-23, 8.201307833595939069E-29 ) ) ;
#7232 = VERTEX_POINT ( 'NONE', #524 ) ;
#7233 = ORIENTED_EDGE ( 'NONE', *, *, #37404, .F. ) ;
#7234 = ORIENTED_EDGE ( 'NONE', *, *, #86589, .F. ) ;
#7235 = CARTESIAN_POINT ( 'NONE',  ( -118.6228709571500559, -24.33832256526968862, 0.1851278514119937824 ) ) ;
#7236 = CARTESIAN_POINT ( 'NONE',  ( 282.9764569301858046, -6.475225279485573360, 20.79159422840526616 ) ) ;
#7237 = CARTESIAN_POINT ( 'NONE',  ( 0.1739078616027790736, -6.376774720514415407, 19.75705121608222115 ) ) ;
#7238 = CARTESIAN_POINT ( 'NONE',  ( -19.97286373971314433, -5.326668811655218327, -1.500000000000002220 ) ) ;
#7239 = CARTESIAN_POINT ( 'NONE',  ( -7.206546067468990735, 20.34698395366585189, 11.49999999999999645 ) ) ;
#7240 = ORIENTED_EDGE ( 'NONE', *, *, #46132, .T. ) ;
#7241 = CARTESIAN_POINT ( 'NONE',  ( -81.55620429048337883, -24.66019654487199730, 8.947790411086124607 ) ) ;
#7242 = CARTESIAN_POINT ( 'NONE',  ( 3.632744579681756569, -5.876774720514403860, 18.17103827887095946 ) ) ;
#7243 = CARTESIAN_POINT ( 'NONE',  ( -1.374798071107336206, -22.32369649477951512, 11.49999999999998934 ) ) ;
#7244 = CARTESIAN_POINT ( 'NONE',  ( -80.26303174456680267, -25.27875086665990878, 7.082509052535141514 ) ) ;
#7245 = CARTESIAN_POINT ( 'NONE',  ( -104.5228709571500758, -24.64898659630529565, 1.056161002820829697 ) ) ;
#7246 = ORIENTED_EDGE ( 'NONE', *, *, #6473, .T. ) ;
#7247 = CARTESIAN_POINT ( 'NONE',  ( -116.5120762170639637, -25.40067276019392395, 5.394074047000503747 ) ) ;
#7248 = CARTESIAN_POINT ( 'NONE',  ( 6.727764423076923350, -5.876774720514413630, 19.76442307692307665 ) ) ;
#7249 = LINE ( 'NONE', #61566, #97286 ) ;
#7250 = CARTESIAN_POINT ( 'NONE',  ( -20.37482282770194075, 4.769447832466558346, -1.500000000000002220 ) ) ;
#7251 = ORIENTED_EDGE ( 'NONE', *, *, #75219, .T. ) ;
#7252 = VECTOR ( 'NONE', #87087, 1000.000000000000000 ) ;
#7254 = VERTEX_POINT ( 'NONE', #55329 ) ;
#7253 = CARTESIAN_POINT ( 'NONE',  ( -86.54257510269528098, -24.65952944569304961, 1.056160979905701680 ) ) ;
#7255 = ORIENTED_EDGE ( 'NONE', *, *, #75443, .T. ) ;
#7256 = CARTESIAN_POINT ( 'NONE',  ( -109.5495832072082720, -24.66019654487200441, 8.947790411086113949 ) ) ;
#7257 = CARTESIAN_POINT ( 'NONE',  ( -12.03079493616482765, -17.41531974249929249, -1.500000000000002220 ) ) ;
#7258 = ORIENTED_EDGE ( 'NONE', *, *, #90223, .T. ) ;
#7259 = CARTESIAN_POINT ( 'NONE',  ( -117.6281488526506678, -23.73766607897670511, -1.055555164236445798 ) ) ;
#7260 = CARTESIAN_POINT ( 'NONE',  ( -99.37409858214790859, -25.26221189400888889, 6.508816812834683496 ) ) ;
#7261 = CARTESIAN_POINT ( 'NONE',  ( -19.23829340896090656, 10.21096329589227025, -1.500000000000002220 ) ) ;
#7262 = CARTESIAN_POINT ( 'NONE',  ( -7.536766146225033047, -6.376774720514411854, 19.63296556618507438 ) ) ;
#7263 = CARTESIAN_POINT ( 'NONE',  ( 19.24418710706453339, -0.5000000000000000000, -2.153101996372891236 ) ) ;
#7264 = CARTESIAN_POINT ( 'NONE',  ( 7.402957069319889172, -5.876774720514418071, 20.34212842306459024 ) ) ;
#7265 = CARTESIAN_POINT ( 'NONE',  ( 18.38516380405726736, -11.72527425286322611, -1.500000000000002220 ) ) ;
#7266 = CARTESIAN_POINT ( 'NONE',  ( -71.53293015653792963, -25.24674183039172704, 5.453599235397658340 ) ) ;
#7267 = ADVANCED_FACE ( 'NONE', ( #31475 ), #61975, .T. ) ;
#7268 = ORIENTED_EDGE ( 'NONE', *, *, #70406, .T. ) ;
#7269 = CARTESIAN_POINT ( 'NONE',  ( 11.22434917415779054, -4.132774715458839232, -26.87660878605755599 ) ) ;
#7270 = CARTESIAN_POINT ( 'NONE',  ( -117.5228709571500474, -23.94994826722565762, -0.6494450866342728057 ) ) ;
#7271 = DIRECTION ( 'NONE',  ( 0.000000000000000000, -0.000000000000000000, -1.000000000000000000 ) ) ;
#7272 = ORIENTED_EDGE ( 'NONE', *, *, #39596, .T. ) ;
#7273 = CIRCLE ( 'NONE', #21819, 1.836000000000000743 ) ;
#7274 = VERTEX_POINT ( 'NONE', #56339 ) ;
#7275 = B_SPLINE_CURVE_WITH_KNOTS ( 'NONE', 3,
 ( #74816, #29146, #13414, #98146 ),
 .UNSPECIFIED., .F., .F.,
 ( 4, 4 ),
 ( 1.387778780781445676E-17, 0.0001000000000000028779 ),
 .UNSPECIFIED. ) ;
#7276 = ORIENTED_EDGE ( 'NONE', *, *, #45884, .F. ) ;
#7277 = ADVANCED_FACE ( 'NONE', ( #64962 ), #19243, .F. ) ;
#7278 = CARTESIAN_POINT ( 'NONE',  ( -124.5228709571500190, -24.66019654487200441, 8.947790411086112172 ) ) ;
#7279 = CARTESIAN_POINT ( 'NONE',  ( 20.46717832272283033, -5.532298862796615424, 11.49999999999998934 ) ) ;
#7280 = CARTESIAN_POINT ( 'NONE',  ( -94.59134195305344406, -24.15543982623907482, -0.2315651400026595141 ) ) ;
#7281 = EDGE_CURVE ( 'NONE', #71450, #36701, #96573, .T. ) ;
#7282 = CARTESIAN_POINT ( 'NONE',  ( -30.64427850938830389, -23.56000036390796737, -1.497999999999532816 ) ) ;
#7283 = CARTESIAN_POINT ( 'NONE',  ( 16.09831413233135677, -3.622774720514429614, -27.82446136760824018 ) ) ;
#7284 = DIRECTION ( 'NONE',  ( -3.773278334453079618E-23, 0.9999999999976377785, 2.173523156925979975E-06 ) ) ;
#7285 = CARTESIAN_POINT ( 'NONE',  ( -18.22047185089115828, 6.579378235550767506, 11.49999999999998934 ) ) ;
#7286 = CARTESIAN_POINT ( 'NONE',  ( 26.25551457520356635, -1.682774720514426114, -10.59759736550662446 ) ) ;
#7287 = ORIENTED_EDGE ( 'NONE', *, *, #81984, .T. ) ;
#7288 = CARTESIAN_POINT ( 'NONE',  ( -17.22176335520693158, -9.073154711715998744, 11.49999999999999645 ) ) ;
#7289 = CARTESIAN_POINT ( 'NONE',  ( -42.52287095715005449, -23.47596703998600631, 11.44779298504229281 ) ) ;
#7290 = CARTESIAN_POINT ( 'NONE',  ( -49.62287095715004170, -23.47596703998600631, 11.44779298504227505 ) ) ;
#7291 = ADVANCED_FACE ( 'NONE', ( #19733 ), #96376, .T. ) ;
#7292 = ORIENTED_EDGE ( 'NONE', *, *, #24680, .F. ) ;
#7293 = CARTESIAN_POINT ( 'NONE',  ( 3.475076759263674209, -6.376774720514401196, 18.20843037655054530 ) ) ;
#7294 = CARTESIAN_POINT ( 'NONE',  ( -70.27422298781921484, -25.30465073045868252, 4.851635164186505200 ) ) ;
#7295 = DIRECTION ( 'NONE',  ( -3.773278334444167608E-23, 1.000000000000000000, 0.000000000000000000 ) ) ;
#7296 = CARTESIAN_POINT ( 'NONE',  ( -93.50972247225219292, -24.35071581493543746, 9.817618358456018157 ) ) ;
#7297 = CARTESIAN_POINT ( 'NONE',  ( -19.61951575358169819, -0.1233725505697131491, 11.49999999999998934 ) ) ;
#7298 = CARTESIAN_POINT ( 'NONE',  ( -41.08147698621603894, -25.27806096597225505, 4.883364703189866596 ) ) ;
#7299 = ORIENTED_EDGE ( 'NONE', *, *, #11842, .T. ) ;
#7300 = CIRCLE ( 'NONE', #25125, 1.325999999999990298 ) ;
#7301 = CARTESIAN_POINT ( 'NONE',  ( -15.49073194614445015, 15.02706685249526686, 11.49999999999998934 ) ) ;
#7302 = PLANE ( 'NONE',  #60958 ) ;
#7303 = CARTESIAN_POINT ( 'NONE',  ( -40.46892904929547541, -25.00158670708910336, 2.256160236439222366 ) ) ;
#7304 = CARTESIAN_POINT ( 'NONE',  ( -121.5895376238167245, -24.64898659630368627, 1.056161002820393602 ) ) ;
#7305 = CARTESIAN_POINT ( 'NONE',  ( -4.971178678486217528, -22.47594730032828281, -1.500000000000002220 ) ) ;
#7306 = PERSON_AND_ORGANIZATION_ROLE ( 'design_supplier' ) ;
#7307 = DIRECTION ( 'NONE',  ( -3.773278334453079030E-23, 0.9999999999976377785, 2.173523156925979128E-06 ) ) ;
#7308 = CARTESIAN_POINT ( 'NONE',  ( -89.62287095715004170, -29.50250243563736774, 8.947779886222139822 ) ) ;
#7309 = CARTESIAN_POINT ( 'NONE',  ( -4.116507902937485142, 19.75820112358731251, 11.49999999999999645 ) ) ;
#7310 = CARTESIAN_POINT ( 'NONE',  ( -121.5222464708741938, -23.48786465467241769, 11.44779295918253759 ) ) ;
#7311 = DIRECTION ( 'NONE',  ( 0.000000000000000000, 0.000000000000000000, -1.000000000000000000 ) ) ;
#7312 = CARTESIAN_POINT ( 'NONE',  ( 22.02124265030973760, 7.743225279485574042, 18.45402280011862217 ) ) ;
#7313 = FACE_OUTER_BOUND ( 'NONE', #49930, .T. ) ;
#7314 = CARTESIAN_POINT ( 'NONE',  ( -111.1810695982967161, -25.18425674466588760, 3.716321248519699694 ) ) ;
#7315 = CARTESIAN_POINT ( 'NONE',  ( 9.006517291608927778, -17.75031788249398446, 11.49999999999998934 ) ) ;
#7316 = DIRECTION ( 'NONE',  ( -3.445208383210904608E-15, 0.9940716917543757081, -0.1087265912856350686 ) ) ;
#7317 = CARTESIAN_POINT ( 'NONE',  ( -13.31955177964949755, -14.60123061082138385, -1.500000000000002220 ) ) ;
#7318 = CARTESIAN_POINT ( 'NONE',  ( -81.52287095715010423, -23.47593901973090524, -1.443836447538996648 ) ) ;
#7319 = EDGE_CURVE ( 'NONE', #94825, #43365, #81152, .T. ) ;
#7320 = CARTESIAN_POINT ( 'NONE',  ( -39.32379795506943054, -25.29116634425743726, 3.365606283317699621 ) ) ;
#7321 = DIRECTION ( 'NONE',  ( -0.000000000000000000, 0.000000000000000000, 1.000000000000000000 ) ) ;
#7322 = CARTESIAN_POINT ( 'NONE',  ( -17.23291202157775359, 11.51834372740795231, 11.49999999999999645 ) ) ;
#7323 = CARTESIAN_POINT ( 'NONE',  ( -56.62287095715005592, -23.47593901973091235, -1.443836447539007972 ) ) ;
#7324 = VECTOR ( 'NONE', #24821, 1000.000000000000227 ) ;
#7325 = EDGE_CURVE ( 'NONE', #77908, #68025, #81305, .T. ) ;
#7326 = CARTESIAN_POINT ( 'NONE',  ( -106.5222054704709649, -23.48783264082477373, -1.443836473390085695 ) ) ;
#7328 = EDGE_CURVE ( 'NONE', #73980, #37074, #56838, .T. ) ;
#7327 = CARTESIAN_POINT ( 'NONE',  ( -22.17926634000774655, 4.976981427743210951, 11.49999999999999645 ) ) ;
#7329 = VERTEX_POINT ( 'NONE', #26367 ) ;
#7330 = LINE ( 'NONE', #30677, #21918 ) ;
#7331 = FACE_OUTER_BOUND ( 'NONE', #92671, .T. ) ;
#7332 = CARTESIAN_POINT ( 'NONE',  ( -19.70923665959843873, 4.302044407003456250, -1.500000000000002220 ) ) ;
#7333 = DIRECTION ( 'NONE',  ( 0.000000000000000000, 0.9999999999976377785, 2.173523156925979975E-06 ) ) ;
#7334 = CIRCLE ( 'NONE', #20303, 2.249999999999998668 ) ;
#7335 = CARTESIAN_POINT ( 'NONE',  ( -50.62287095715005592, -24.99132157543083821, 2.256160258750667502 ) ) ;
#7336 = EDGE_LOOP ( 'NONE', ( #94266, #96149, #63303, #25912, #14216 ) ) ;
#7337 = AXIS2_PLACEMENT_3D ( 'NONE', #18591, #42460, #35336 ) ;
#7338 = ORIENTED_EDGE ( 'NONE', *, *, #31572, .T. ) ;
#7339 = DIRECTION ( 'NONE',  ( -3.773278334453080206E-23, 0.9999999999976377785, 2.173523156925979975E-06 ) ) ;
#7340 = CARTESIAN_POINT ( 'NONE',  ( 18.56524475492553705, -13.42312393814442650, -1.500000000000002220 ) ) ;
#7341 = CARTESIAN_POINT ( 'NONE',  ( -51.19827071096799642, -25.27420643956589785, 3.666039933461763489 ) ) ;
#7342 = CARTESIAN_POINT ( 'NONE',  ( -7.614213781628100364, -20.28429660096114517, -1.500000000000002220 ) ) ;
#7343 = CARTESIAN_POINT ( 'NONE',  ( -123.5557606486684676, -23.96119346886881019, -0.6495511937832023630 ) ) ;
#7344 = LINE ( 'NONE', #45438, #25790 ) ;
#7345 = CARTESIAN_POINT ( 'NONE',  ( 20.66465755290784401, -3.126920214821775623, 11.49999999999999645 ) ) ;
#7346 = ORIENTED_EDGE ( 'NONE', *, *, #4097, .F. ) ;
#7347 = CARTESIAN_POINT ( 'NONE',  ( -69.32616065491644974, -25.31612503761393285, 5.234946770129553784 ) ) ;
#7348 = CARTESIAN_POINT ( 'NONE',  ( -6.199593828526920092, 21.14725108817225419, 11.49999999999998934 ) ) ;
#7349 = ADVANCED_FACE ( 'NONE', ( #49722 ), #45740, .T. ) ;
#7350 = EDGE_CURVE ( 'NONE', #95505, #42298, #43594, .T. ) ;
#7351 = CARTESIAN_POINT ( 'NONE',  ( -105.5110081277101983, -24.63419186844610920, 9.035850630976920428 ) ) ;
#7352 = CARTESIAN_POINT ( 'NONE',  ( -40.62732473945732181, -25.29087035909526904, 2.839335978436782870 ) ) ;
#7353 = VERTEX_POINT ( 'NONE', #5517 ) ;
#7354 = CARTESIAN_POINT ( 'NONE',  ( 33.96422015159436114, -5.965225279485572685, -7.233236000911337449 ) ) ;
#7355 = DIRECTION ( 'NONE',  ( 0.000000000000000000, 0.9999999999976377785, 2.173523156925979128E-06 ) ) ;
#7356 = ORIENTED_EDGE ( 'NONE', *, *, #18724, .T. ) ;
#7357 = CARTESIAN_POINT ( 'NONE',  ( -62.52287095715006160, -29.50250243563736774, 8.947779886222145151 ) ) ;
#7358 = ORIENTED_EDGE ( 'NONE', *, *, #2614, .F. ) ;
#7359 = ORIENTED_EDGE ( 'NONE', *, *, #36750, .F. ) ;
#7360 = CARTESIAN_POINT ( 'NONE',  ( -71.59236747742473028, -24.15620529776628445, 10.23563542870660115 ) ) ;
#7361 = B_SPLINE_CURVE_WITH_KNOTS ( 'NONE', 3,
 ( #3005, #4985, #33941, #42068, #83592, #46055 ),
 .UNSPECIFIED., .F., .F.,
 ( 4, 2, 4 ),
 ( 6.391158118961560919E-06, 0.001387004593080787230, 0.002767618028042612838 ),
 .UNSPECIFIED. ) ;
#7362 = CARTESIAN_POINT ( 'NONE',  ( -12.64432969575900323, 5.965225279485592225, -26.13179214487284696 ) ) ;
#7363 = CARTESIAN_POINT ( 'NONE',  ( -36.48447499359400581, -24.51314013834317151, 0.6176544820404150649 ) ) ;
#7364 = CARTESIAN_POINT ( 'NONE',  ( -0.3173379506236611580, 20.48240526196808631, -1.500000000000002220 ) ) ;
#7365 = ORIENTED_EDGE ( 'NONE', *, *, #37071, .F. ) ;
#7366 = CARTESIAN_POINT ( 'NONE',  ( -3.071531057816138333, -5.876774720514412742, 19.86545874326175110 ) ) ;
#7367 = ADVANCED_FACE ( 'NONE', ( #4540 ), #66458, .F. ) ;
#7368 = CARTESIAN_POINT ( 'NONE',  ( -44.60756723058806017, -23.73766607897669800, -1.055555164236458898 ) ) ;
#7369 = CARTESIAN_POINT ( 'NONE',  ( 8.971512145086506962, -2.028487854913504140, -5.500000000000000000 ) ) ;
#7370 = CARTESIAN_POINT ( 'NONE',  ( 6.212073114426278408, 21.40951068830820958, 11.49999999999998934 ) ) ;
#7371 = EDGE_CURVE ( 'NONE', #87883, #34838, #98861, .T. ) ;
#7372 = CARTESIAN_POINT ( 'NONE',  ( -4.743266218460161276, -6.376774720514413630, 19.49357334786887108 ) ) ;
#7373 = CARTESIAN_POINT ( 'NONE',  ( -28.58953762381672092, -24.49418409732524538, 8.947790446961807476 ) ) ;
#7374 = ORIENTED_EDGE ( 'NONE', *, *, #10830, .F. ) ;
#7375 = LINE ( 'NONE', #86006, #87349 ) ;
#7376 = CARTESIAN_POINT ( 'NONE',  ( -39.52287095715006160, -23.73934037231757088, 11.05740245334329153 ) ) ;
#7377 = CONICAL_SURFACE ( 'NONE', #13812, 1.249999999999996003, 0.7853981633974514986 ) ;
#7378 = CARTESIAN_POINT ( 'NONE',  ( -20.21371806590929410, -4.994250807877889109, -1.500000000000002220 ) ) ;
#7379 = ORIENTED_EDGE ( 'NONE', *, *, #9893, .T. ) ;
#7381 = ORIENTED_EDGE ( 'NONE', *, *, #47429, .F. ) ;
#7380 = LINE ( 'NONE', #30218, #13081 ) ;
#7382 = CARTESIAN_POINT ( 'NONE',  ( -98.52287095714999055, -23.73934037231757088, 11.05740245334328087 ) ) ;
#7383 = ORIENTED_EDGE ( 'NONE', *, *, #60257, .T. ) ;
#7384 = VERTEX_POINT ( 'NONE', #67938 ) ;
#7385 = CARTESIAN_POINT ( 'NONE',  ( 8.035386273831683468, 10.29654910626257802, -0.9008313202359966576 ) ) ;
#7386 = LINE ( 'NONE', #24112, #46410 ) ;
#7387 = PLANE ( 'NONE',  #77294 ) ;
#7388 = DIRECTION ( 'NONE',  ( 3.773278334444167608E-23, -1.000000000000000000, 0.000000000000000000 ) ) ;
#7389 = CARTESIAN_POINT ( 'NONE',  ( -109.6272648782309886, -25.14892542572373202, 2.994947275832184896 ) ) ;
#7390 = DIRECTION ( 'NONE',  ( 0.000000000000000000, 0.000000000000000000, 1.000000000000000000 ) ) ;
#7391 = ADVANCED_FACE ( 'NONE', ( #82641 ), #46586, .T. ) ;
#7393 = ORIENTED_EDGE ( 'NONE', *, *, #89661, .T. ) ;
#7392 = CARTESIAN_POINT ( 'NONE',  ( -18.93877658415168241, -11.43451605920036052, 11.49999999999999645 ) ) ;
#7394 = DIRECTION ( 'NONE',  ( 0.000000000000000000, 1.000000000000000000, 0.000000000000000000 ) ) ;
#7395 = EDGE_LOOP ( 'NONE', ( #58564, #62674, #90943, #12069 ) ) ;
#7396 = CARTESIAN_POINT ( 'NONE',  ( 20.10346781357453949, 10.43426432342431553, -1.500000000000002220 ) ) ;
#7398 = ORIENTED_EDGE ( 'NONE', *, *, #77021, .T. ) ;
#7397 = CARTESIAN_POINT ( 'NONE',  ( -29.23546583316962710, -25.19426066751507065, 5.521667863429778222 ) ) ;
#7399 = ORIENTED_EDGE ( 'NONE', *, *, #60163, .F. ) ;
#7400 = CARTESIAN_POINT ( 'NONE',  ( -57.55620429048340725, -23.47596703998600276, 11.44779298504227505 ) ) ;
#7401 = EDGE_CURVE ( 'NONE', #72936, #99871, #52193, .T. ) ;
#7402 = B_SPLINE_CURVE_WITH_KNOTS ( 'NONE', 3,
 ( #43358, #20990, #45351, #4786 ),
 .UNSPECIFIED., .F., .F.,
 ( 4, 4 ),
 ( 0.000000000000000000, 9.999999999998897304E-05 ),
 .UNSPECIFIED. ) ;
#7403 = CARTESIAN_POINT ( 'NONE',  ( -17.82723130383223165, -9.322377578706960932, -1.500000000000002220 ) ) ;
#7404 = ADVANCED_FACE ( 'NONE', ( #59826 ), #400, .T. ) ;
#7405 = DIRECTION ( 'NONE',  ( -0.03244919754393515293, 0.000000000000000000, 0.9994733861282923959 ) ) ;
#7406 = EDGE_LOOP ( 'NONE', ( #58456, #19362 ) ) ;
#7407 = VECTOR ( 'NONE', #90643, 1000.000000000000114 ) ;
#7408 = DIRECTION ( 'NONE',  ( -1.000000000000000000, -0.000000000000000000, -0.000000000000000000 ) ) ;
#7409 = CARTESIAN_POINT ( 'NONE',  ( -2.124831620219566730, 22.23837930986240607, -1.500000000000002220 ) ) ;
#7410 = AXIS2_PLACEMENT_3D ( 'NONE', #73833, #10429, #41390 ) ;
#7411 = EDGE_CURVE ( 'NONE', #84489, #65436, #15131, .T. ) ;
#7412 = CIRCLE ( 'NONE', #77089, 253.2618649670780826 ) ;
#7413 = ORIENTED_EDGE ( 'NONE', *, *, #7498, .T. ) ;
#7414 = VERTEX_POINT ( 'NONE', #61825 ) ;
#7415 = CARTESIAN_POINT ( 'NONE',  ( -101.2134684488937069, -25.25341235495022474, 6.841542769133510227 ) ) ;
#7416 = DIRECTION ( 'NONE',  ( 0.000000000000000000, 2.173523156925980399E-06, -0.9999999999976378895 ) ) ;
#7417 = PLANE ( 'NONE',  #29541 ) ;
#7418 = CARTESIAN_POINT ( 'NONE',  ( 32.45853543194704116, 0.3587747205144265483, 9.169203677920338080 ) ) ;
#7419 = VECTOR ( 'NONE', #95825, 1000.000000000000000 ) ;
#7420 = EDGE_CURVE ( 'NONE', #83680, #92224, #69425, .T. ) ;
#7421 = FACE_OUTER_BOUND ( 'NONE', #84530, .T. ) ;
#7422 = CARTESIAN_POINT ( 'NONE',  ( -8.292788067677484776, 17.68049324621676632, -1.500000000000002220 ) ) ;
#7423 = CARTESIAN_POINT ( 'NONE',  ( -38.62287095715005592, -23.47596703998600276, 11.44779298504227505 ) ) ;
#7424 = CARTESIAN_POINT ( 'NONE',  ( 11.86944616785735818, -17.87650476368427732, -1.500000000000002220 ) ) ;
#7425 = CARTESIAN_POINT ( 'NONE',  ( -25.53098197642538736, -24.58000217321816194, 4.942812437106832490 ) ) ;
#7426 = LINE ( 'NONE', #6934, #71374 ) ;
#7427 = CARTESIAN_POINT ( 'NONE',  ( -126.6228709571500559, -29.50247984919015209, -1.443849546365044922 ) ) ;
#7428 = CARTESIAN_POINT ( 'NONE',  ( 2.875404258304424143, 22.71175023210845012, -1.500000000000002220 ) ) ;
#7429 = COORDINATED_UNIVERSAL_TIME_OFFSET ( 0, 0, .AHEAD. ) ;
#7430 = CARTESIAN_POINT ( 'NONE',  ( -104.6228709571500559, -24.66019654487200086, 8.947790411086124607 ) ) ;
#7431 = CARTESIAN_POINT ( 'NONE',  ( -108.5228709571500758, -24.51283580621449687, 0.6167428607045382094 ) ) ;
#7432 = CARTESIAN_POINT ( 'NONE',  ( 2.879247915899910470, -19.84986158617241614, 11.49999999999999645 ) ) ;
#7433 = CARTESIAN_POINT ( 'NONE',  ( -79.34156256387794315, -25.31594405533091674, 4.917719298043063958 ) ) ;
#7434 = CARTESIAN_POINT ( 'NONE',  ( -64.55620429048339304, -24.64898659630529210, 1.056161002820825923 ) ) ;
#7435 = CARTESIAN_POINT ( 'NONE',  ( 3.797776442307698286, -5.876774720514402084, 18.16025641025640525 ) ) ;
#7436 = CARTESIAN_POINT ( 'NONE',  ( -104.5228709571500758, -29.50250243563736774, 8.947779886222138046 ) ) ;
#7437 = ORIENTED_EDGE ( 'NONE', *, *, #52311, .T. ) ;
#7438 = CARTESIAN_POINT ( 'NONE',  ( -26.36100103624393753, -24.65813067085167631, 2.183744232383703299 ) ) ;
#7439 = CARTESIAN_POINT ( 'NONE',  ( 13.91401389203221406, -5.965225279485572685, 28.26920385068457264 ) ) ;
#7440 = CARTESIAN_POINT ( 'NONE',  ( 1.329761939549756855, 21.69843865049760367, -1.500000000000002220 ) ) ;
#7441 = CARTESIAN_POINT ( 'NONE',  ( -1.358974358974357921, -6.376774720514420736, 20.75510817307693046 ) ) ;
#7442 = CARTESIAN_POINT ( 'NONE',  ( 5.347671334029483248, -18.86178030415664963, -1.500000000000002220 ) ) ;
#7443 = LINE ( 'NONE', #76947, #55581 ) ;
#7444 = ADVANCED_FACE ( 'NONE', ( #30859 ), #44724, .F. ) ;
#7445 = CARTESIAN_POINT ( 'NONE',  ( -109.6235167689328591, -25.27925821723561128, 4.923693497153672993 ) ) ;
#7446 = CONTEXT_DEPENDENT_SHAPE_REPRESENTATION ( #26556, #12601 ) ;
#7447 = CARTESIAN_POINT ( 'NONE',  ( -124.5228709571500616, -29.50248528299804818, 1.056150453629045360 ) ) ;
#7448 = CARTESIAN_POINT ( 'NONE',  ( -47.52287095715006160, -24.50321055353805377, 9.387540953477525818 ) ) ;
#7449 = CARTESIAN_POINT ( 'NONE',  ( 19.83930831332124001, -5.160774681608516268, 11.49999999999999645 ) ) ;
#7450 = CARTESIAN_POINT ( 'NONE',  ( -94.52287095715004739, -24.50216790748205042, 0.6166512839542538371 ) ) ;
#7451 = CARTESIAN_POINT ( 'NONE',  ( -120.6253545820920294, -24.52300882791530512, 0.6510814631126412566 ) ) ;
#7452 = ORIENTED_EDGE ( 'NONE', *, *, #2398, .F. ) ;
#7453 = SHAPE_REPRESENTATION_RELATIONSHIP ( 'NONE' , 'NONE' ,  #26923, #64713 ) ;
#7454 = CARTESIAN_POINT ( 'NONE',  ( 0.1645010273463769490, -1.417169167140626129, -0.3687607960183705291 ) ) ;
#7455 = LINE ( 'NONE', #38412, #91491 ) ;
#7456 = CARTESIAN_POINT ( 'NONE',  ( -125.5551857379501541, -24.40133493613050675, 9.663955038902798833 ) ) ;
#7457 = DIRECTION ( 'NONE',  ( 0.000000000000000000, -2.173523156925979552E-06, 0.9999999999976378895 ) ) ;
#7458 = CARTESIAN_POINT ( 'NONE',  ( 22.02124265030973760, -4.543225279485573864, 18.45402280011862217 ) ) ;
#7459 = CARTESIAN_POINT ( 'NONE',  ( 32.34323322234308762, 6.036341485554500785, 0.7979233379450167973 ) ) ;
#7460 = VECTOR ( 'NONE', #60259, 1000.000000000000114 ) ;
#7461 = B_SPLINE_CURVE_WITH_KNOTS ( 'NONE', 3,
 ( #74200, #35641, #12781, #90914 ),
 .UNSPECIFIED., .F., .F.,
 ( 4, 4 ),
 ( 0.000000000000000000, 1.000000000000000000 ),
 .UNSPECIFIED. ) ;
#7462 = CARTESIAN_POINT ( 'NONE',  ( 16.10802587768190008, -16.50329280669357246, 11.49999999999999645 ) ) ;
#7463 = CARTESIAN_POINT ( 'NONE',  ( 22.53581206741051446, 3.480912172000575122, 11.49999999999998934 ) ) ;
#7464 = CARTESIAN_POINT ( 'NONE',  ( -125.6228709571500843, -25.00158670708909625, 2.256160236439166855 ) ) ;
#7465 = FACE_OUTER_BOUND ( 'NONE', #29334, .T. ) ;
#7466 = LINE ( 'NONE', #31310, #82493 ) ;
#7467 = CARTESIAN_POINT ( 'NONE',  ( 21.53444271425275858, 6.169869319618734416, 11.49999999999999645 ) ) ;
#7468 = ORIENTED_EDGE ( 'NONE', *, *, #93457, .T. ) ;
#7469 = DIRECTION ( 'NONE',  ( -1.000000000000000000, 0.000000000000000000, 0.000000000000000000 ) ) ;
#7470 = FACE_OUTER_BOUND ( 'NONE', #77145, .T. ) ;
#7471 = CARTESIAN_POINT ( 'NONE',  ( -16.24880213243413607, 14.73142910551002238, -1.500000000000002220 ) ) ;
#7472 = CARTESIAN_POINT ( 'NONE',  ( -5.378122165843598701, -6.376774720514411854, 19.21968329462762526 ) ) ;
#7473 = TOROIDAL_SURFACE ( 'NONE', #64227, 253.2618649670780826, 1.835999999999999854 ) ;
#7474 = EDGE_CURVE ( 'NONE', #34973, #14282, #14628, .T. ) ;
#7475 = CYLINDRICAL_SURFACE ( 'NONE', #65752, 1.149999999999998135 ) ;
#7476 = CARTESIAN_POINT ( 'NONE',  ( -34.52287095715004739, -24.66019654487199730, 8.947790411086121054 ) ) ;
#7477 = CARTESIAN_POINT ( 'NONE',  ( 32.45853543194704116, 0.3587747205144265483, 9.169203677920338080 ) ) ;
#7478 = CARTESIAN_POINT ( 'NONE',  ( -117.6228709571500559, -23.94994826722515668, -0.6494450866351687557 ) ) ;
#7479 = VERTEX_POINT ( 'NONE', #409 ) ;
#7480 = AXIS2_PLACEMENT_3D ( 'NONE', #8358, #56431, #31189 ) ;
#7481 = CARTESIAN_POINT ( 'NONE',  ( -9.379331868514380943, 18.20734191464070406, 11.49999999999998934 ) ) ;
#7482 = EDGE_LOOP ( 'NONE', ( #54312, #64331, #3876, #29456 ) ) ;
#7483 = VECTOR ( 'NONE', #33095, 1000.000000000000114 ) ;
#7484 = EDGE_LOOP ( 'NONE', ( #68401, #7116, #10610, #77647 ) ) ;
#7485 = ORIENTED_EDGE ( 'NONE', *, *, #68898, .F. ) ;
#7486 = B_SPLINE_CURVE_WITH_KNOTS ( 'NONE', 3,
 ( #624, #32573, #55932, #63554 ),
 .UNSPECIFIED., .F., .F.,
 ( 4, 4 ),
 ( 2.775557561562891043E-17, 9.999999999998898659E-05 ),
 .UNSPECIFIED. ) ;
#7487 = VERTEX_POINT ( 'NONE', #46596 ) ;
#7488 = CARTESIAN_POINT ( 'NONE',  ( -23.05830607064937965, -0.9945063503333604338, 11.49999999999998934 ) ) ;
#7489 = DIRECTION ( 'NONE',  ( -3.773278334453079618E-23, 0.9999999999976377785, 2.173523156925979975E-06 ) ) ;
#7490 = CARTESIAN_POINT ( 'NONE',  ( -18.77428246231291808, -7.638711222589018135, -1.500000000000002220 ) ) ;
#7491 = CIRCLE ( 'NONE', #47993, 252.4458649670781085 ) ;
#7492 = EDGE_LOOP ( 'NONE', ( #57604, #23239, #76064, #44842 ) ) ;
#7493 = ADVANCED_FACE ( 'NONE', ( #78518, #8527, #9026, #77521, #8020 ), #37971, .T. ) ;
#7494 = CARTESIAN_POINT ( 'NONE',  ( -90.55620429048337883, -25.00182538069145721, 7.747789668545099317 ) ) ;
#7495 = EDGE_CURVE ( 'NONE', #5872, #64045, #77084, .T. ) ;
#7496 = CARTESIAN_POINT ( 'NONE',  ( -127.5895376238166961, -24.64965694238408034, 8.947790433994645909 ) ) ;
#7497 = CIRCLE ( 'NONE', #70659, 11.85241003308275864 ) ;
#7498 = EDGE_CURVE ( 'NONE', #40585, #51301, #39478, .T. ) ;
#7499 = LINE ( 'NONE', #61805, #31870 ) ;
#7500 = CARTESIAN_POINT ( 'NONE',  ( -70.60486894837754335, -23.85016227208580730, -0.8807180028928335291 ) ) ;
#7502 = ORIENTED_EDGE ( 'NONE', *, *, #9009, .T. ) ;
#7501 = CARTESIAN_POINT ( 'NONE',  ( -21.12015818079280649, -3.594773940630530795, 11.49999999999999645 ) ) ;
#7503 = CARTESIAN_POINT ( 'NONE',  ( -75.49320323011643552, -24.83618233451450763, 1.606449574219540599 ) ) ;
#7504 = LINE ( 'NONE', #14109, #66921 ) ;
#7505 = EDGE_CURVE ( 'NONE', #72155, #88376, #53714, .T. ) ;
#7506 = ORIENTED_EDGE ( 'NONE', *, *, #54767, .F. ) ;
#7507 = CARTESIAN_POINT ( 'NONE',  ( -0.2510023010970363067, -20.70922355669356563, 11.49999999999998934 ) ) ;
#7508 = ORIENTED_EDGE ( 'NONE', *, *, #18593, .T. ) ;
#7510 = EDGE_LOOP ( 'NONE', ( #52672, #41872, #14007, #28461 ) ) ;
#7509 = CARTESIAN_POINT ( 'NONE',  ( 27.53860345374808105, -1.477225279485574028, 19.84760796525321780 ) ) ;
#7511 = CARTESIAN_POINT ( 'NONE',  ( -102.6228709571500559, -23.47593901973091235, -1.443836447539001089 ) ) ;
#7512 = ORIENTED_EDGE ( 'NONE', *, *, #44637, .T. ) ;
#7513 = EDGE_LOOP ( 'NONE', ( #86537, #61319, #9067, #31998 ) ) ;
#7514 = CARTESIAN_POINT ( 'NONE',  ( 3.960454120839856706, -5.876774720514401196, 18.17119035270509997 ) ) ;
#7515 = PLANE ( 'NONE',  #74066 ) ;
#7516 = CARTESIAN_POINT ( 'NONE',  ( -65.62787674017165784, -24.83618233451449697, 1.606449574219540155 ) ) ;
#7517 = ADVANCED_FACE ( 'NONE', ( #76515 ), #16130, .F. ) ;
#7518 = CARTESIAN_POINT ( 'NONE',  ( -20.77788740438921522, -7.151594987469691134, 11.49999999999999645 ) ) ;
#7519 = CARTESIAN_POINT ( 'NONE',  ( -89.62850461461094653, -24.35071581493543391, 9.817618358456025263 ) ) ;
#7520 = CARTESIAN_POINT ( 'NONE',  ( 17.82461400791848405, -13.82690402418615960, -1.500000000000002220 ) ) ;
#7521 = TOROIDAL_SURFACE ( 'NONE', #70683, 80.18232118519038920, 9.179999999999999716 ) ;
#7522 = CARTESIAN_POINT ( 'NONE',  ( -18.73635099073748833, 9.434554061794083069, 11.49999999999998934 ) ) ;
#7523 = CARTESIAN_POINT ( 'NONE',  ( 5.471383689419962337, 5.965225279485594001, -29.02273493113403902 ) ) ;
#7524 = CARTESIAN_POINT ( 'NONE',  ( 8.456965425111588885, -0.2003331576018184679, -3.712238059855192951 ) ) ;
#7526 = EDGE_CURVE ( 'NONE', #71823, #44958, #99847, .T. ) ;
#7525 = EDGE_LOOP ( 'NONE', ( #53611, #77228, #80081, #6569, #90860, #79894 ) ) ;
#7527 = VERTEX_POINT ( 'NONE', #72937 ) ;
#7528 = ORIENTED_EDGE ( 'NONE', *, *, #96630, .F. ) ;
#7529 = CARTESIAN_POINT ( 'NONE',  ( -112.5228709571500616, -24.65952944569304961, 1.056160979905704123 ) ) ;
#7530 = B_SPLINE_CURVE_WITH_KNOTS ( 'NONE', 3,
 ( #2077, #45007, #81687, #19273, #66491, #97404 ),
 .UNSPECIFIED., .F., .F.,
 ( 4, 2, 4 ),
 ( 6.384118678612105596E-06, 0.001386860460828374117, 0.002767336802978135821 ),
 .UNSPECIFIED. ) ;
#7531 = EDGE_CURVE ( 'NONE', #57717, #83300, #42000, .T. ) ;
#7532 = B_SPLINE_CURVE_WITH_KNOTS ( 'NONE', 3,
 ( #31228, #63711, #17507, #39841 ),
 .UNSPECIFIED., .F., .F.,
 ( 4, 4 ),
 ( 0.000000000000000000, 9.999999999999591193E-05 ),
 .UNSPECIFIED. ) ;
#7533 = CARTESIAN_POINT ( 'NONE',  ( 7.367719877546908158, -20.20905560389912026, -1.500000000000002220 ) ) ;
#7534 = CARTESIAN_POINT ( 'NONE',  ( 30.09341516180546350, -1.477225279485574028, -11.39311774897855756 ) ) ;
#7535 = ORIENTED_EDGE ( 'NONE', *, *, #96338, .T. ) ;
#7536 = CARTESIAN_POINT ( 'NONE',  ( 0.3207198112191017025, -21.10926996749724083, 11.49999999999998934 ) ) ;
#7537 = DIRECTION ( 'NONE',  ( 3.773278334444167608E-23, -1.000000000000000000, 0.000000000000000000 ) ) ;
#7538 = CARTESIAN_POINT ( 'NONE',  ( -60.73059407482809036, -25.14083923594472125, 2.947789366366679875 ) ) ;
#7539 = DIRECTION ( 'NONE',  ( 0.6599726524652347326, 0.000000000000000000, -0.7512896232465895441 ) ) ;
#7540 = CARTESIAN_POINT ( 'NONE',  ( -89.52287095715006160, -29.50250243563736774, 8.947779886222139822 ) ) ;
#7541 = LINE ( 'NONE', #55737, #76186 ) ;
#7542 = CARTESIAN_POINT ( 'NONE',  ( 14.67205787815721862, 16.58792043909384262, -1.500000000000002220 ) ) ;
#7543 = CARTESIAN_POINT ( 'NONE',  ( -71.63072430240342214, -24.34968618360933945, 0.1864209137778822800 ) ) ;
#7544 = EDGE_CURVE ( 'NONE', #21016, #91623, #68014, .T. ) ;
#7545 = ORIENTED_EDGE ( 'NONE', *, *, #16805, .F. ) ;
#7546 = CARTESIAN_POINT ( 'NONE',  ( -20.27875734969026311, 6.143225279485574397, 24.00402280011862288 ) ) ;
#7547 = CARTESIAN_POINT ( 'NONE',  ( 12.00135123753652877, 5.092666038735283784, -26.74699110798160007 ) ) ;
#7548 = LINE ( 'NONE', #1951, #63104 ) ;
#7549 = VECTOR ( 'NONE', #55378, 1000.000000000000000 ) ;
#7550 = EDGE_CURVE ( 'NONE', #15460, #69866, #71944, .T. ) ;
#7551 = CARTESIAN_POINT ( 'NONE',  ( -100.5087677528688062, -24.63355581998385091, 0.9682620441943978751 ) ) ;
#7552 = EDGE_CURVE ( 'NONE', #62807, #896, #59572, .T. ) ;
#7553 = CARTESIAN_POINT ( 'NONE',  ( -7.499459838998954631, -17.95702976299720532, -1.500000000000002220 ) ) ;
#7554 = CARTESIAN_POINT ( 'NONE',  ( -18.12654925440673637, -11.31956730046968751, 11.49999999999998934 ) ) ;
#7555 = CARTESIAN_POINT ( 'NONE',  ( -68.93918693012690824, -25.25799956426409665, 6.184868438663939649 ) ) ;
#7556 = CARTESIAN_POINT ( 'NONE',  ( -106.6228709571500559, -23.48783264082479150, -1.443836473390060382 ) ) ;
#7557 = DIRECTION ( 'NONE',  ( 0.7512896232465892110, 0.000000000000000000, 0.6599726524652351767 ) ) ;
#7558 = LINE ( 'NONE', #55253, #89762 ) ;
#7559 = CARTESIAN_POINT ( 'NONE',  ( -22.35490716430079061, -3.811827842488555440, -1.500000000000002220 ) ) ;
#7560 = VECTOR ( 'NONE', #98553, 1000.000000000000114 ) ;
#7561 = AXIS2_PLACEMENT_3D ( 'NONE', #48955, #79885, #2785 ) ;
#7562 = LINE ( 'NONE', #100384, #14194 ) ;
#7563 = CARTESIAN_POINT ( 'NONE',  ( -24.90875734969025501, 5.965225279485572685, 19.84760796525321780 ) ) ;
#7564 = CARTESIAN_POINT ( 'NONE',  ( 17.16143643543069075, 9.858047367376444825, 11.49999999999999645 ) ) ;
#7565 = AXIS2_PLACEMENT_3D ( 'NONE', #14631, #30358, #17006 ) ;
#7566 = CARTESIAN_POINT ( 'NONE',  ( 8.197725756732245017, -0.4963810196290943111, 3.727086380289611700 ) ) ;
#7567 = EDGE_LOOP ( 'NONE', ( #41051, #39856, #88816, #95732 ) ) ;
#7568 = PLANE ( 'NONE',  #89887 ) ;
#7569 = CARTESIAN_POINT ( 'NONE',  ( -6.181720432442950219, -5.876774720514410077, 19.67464842890028720 ) ) ;
#7570 = CARTESIAN_POINT ( 'NONE',  ( -71.52287095715007581, -24.64965694238408034, 8.947790433994200043 ) ) ;
#7571 = CARTESIAN_POINT ( 'NONE',  ( 21.56569437331729233, -1.927008741106717604, 11.49999999999998934 ) ) ;
#7572 = CARTESIAN_POINT ( 'NONE',  ( -66.58953762381672448, -24.65952944569304606, 1.056160979905694131 ) ) ;
#7574 = CIRCLE ( 'NONE', #18935, 4.080000000000000071 ) ;
#7573 = CARTESIAN_POINT ( 'NONE',  ( -19.39930850525863804, 0.8904154686948315689, -1.500000000000002220 ) ) ;
#7575 = CARTESIAN_POINT ( 'NONE',  ( -80.52287095715006160, -24.15516710230293995, 10.28746687063725851 ) ) ;
#7576 = CARTESIAN_POINT ( 'NONE',  ( -55.48002222786107041, -24.92592662359561118, 8.075495903017996469 ) ) ;
#7577 = CARTESIAN_POINT ( 'NONE',  ( 12.34629653512297409, 15.52844579862587437, 11.49999999999998934 ) ) ;
#7578 = EDGE_LOOP ( 'NONE', ( #15889, #49427, #3170, #75376 ) ) ;
#7579 = CARTESIAN_POINT ( 'NONE',  ( -18.82647582233506611, 7.659846263794035437, 11.49999999999999645 ) ) ;
#7580 = CARTESIAN_POINT ( 'NONE',  ( -80.63078619424426563, -24.63355581998386157, 0.9682620441943954326 ) ) ;
#7581 = LINE ( 'NONE', #84698, #2027 ) ;
#7582 = ORIENTED_EDGE ( 'NONE', *, *, #15332, .F. ) ;
#7583 = CARTESIAN_POINT ( 'NONE',  ( -102.5854978320862045, -24.66019654487200086, 8.947790411086115725 ) ) ;
#7584 = DIRECTION ( 'NONE',  ( 0.000000000000000000, 0.000000000000000000, -1.000000000000000000 ) ) ;
#7585 = CARTESIAN_POINT ( 'NONE',  ( -96.62287095715005592, -24.33927499327854704, 9.819080762295817166 ) ) ;
#7586 = CARTESIAN_POINT ( 'NONE',  ( -40.52986559551381873, -24.73531770709094957, 8.716586749053510275 ) ) ;
#7587 = CARTESIAN_POINT ( 'NONE',  ( -0.8502773128684013582, -5.876774720514413630, 19.61227901093089798 ) ) ;
#7588 = CARTESIAN_POINT ( 'NONE',  ( -18.81522532469529452, 6.996975221643539911, 11.49999999999998934 ) ) ;
#7589 = CARTESIAN_POINT ( 'NONE',  ( -85.52287095715010423, -24.82558206586148941, 1.605769216559626678 ) ) ;
#7590 = ORIENTED_EDGE ( 'NONE', *, *, #93052, .F. ) ;
#7591 = CARTESIAN_POINT ( 'NONE',  ( 1.600000000000000755, 0.000000000000000000, 0.000000000000000000 ) ) ;
#7592 = AXIS2_PLACEMENT_3D ( 'NONE', #81395, #27107, #97607 ) ;
#7593 = CARTESIAN_POINT ( 'NONE',  ( -21.74799678179195794, 7.114197580472080951, 11.49999999999999645 ) ) ;
#7594 = CARTESIAN_POINT ( 'NONE',  ( 9.518656604726816184, -20.62229310799655124, 11.49999999999998934 ) ) ;
#7595 = ORIENTED_EDGE ( 'NONE', *, *, #43839, .F. ) ;
#7596 = CARTESIAN_POINT ( 'NONE',  ( -30.47287095715007865, -24.48302893026593452, 9.401871521831095535 ) ) ;
#7597 = CARTESIAN_POINT ( 'NONE',  ( 12.66784028006542151, 2.682774720514427003, -27.12025593822526304 ) ) ;
#7598 = CARTESIAN_POINT ( 'NONE',  ( -39.96950833219506904, -25.20884380724118401, 3.393814871506949604 ) ) ;
#7599 = CARTESIAN_POINT ( 'NONE',  ( -73.62287095715005592, -23.48783264082478084, -1.443836473390067487 ) ) ;
#7600 = CARTESIAN_POINT ( 'NONE',  ( -128.5553789593330976, -24.66019654487200441, 8.947790411086112172 ) ) ;
#7601 = B_SPLINE_CURVE_WITH_KNOTS ( 'NONE', 3,
 ( #40979, #26251, #50098, #97256, #33352, #95758 ),
 .UNSPECIFIED., .F., .F.,
 ( 4, 2, 4 ),
 ( 1.570887131794795405E-05, 0.001396322306279761940, 0.002776935741241575838 ),
 .UNSPECIFIED. ) ;
#7602 = CARTESIAN_POINT ( 'NONE',  ( -44.52287095715006160, -29.50248528299804818, 1.056150453629031594 ) ) ;
#7603 = ORIENTED_EDGE ( 'NONE', *, *, #34567, .F. ) ;
#7604 = EDGE_CURVE ( 'NONE', #17917, #70388, #30437, .T. ) ;
#7605 = CARTESIAN_POINT ( 'NONE',  ( 11.27307661227339430, 16.98952936956587934, 11.49999999999998934 ) ) ;
#7607 = EDGE_CURVE ( 'NONE', #15338, #47721, #51172, .T. ) ;
#7606 = VERTEX_POINT ( 'NONE', #42500 ) ;
#7608 = CARTESIAN_POINT ( 'NONE',  ( 14.37299948674089123, 17.95305339730678185, 11.49999999999998934 ) ) ;
#7610 = LINE ( 'NONE', #47187, #66385 ) ;
#7609 = B_SPLINE_CURVE_WITH_KNOTS ( 'NONE', 3,
 ( #78671, #57388, #40645, #65005 ),
 .UNSPECIFIED., .F., .F.,
 ( 4, 4 ),
 ( 0.000000000000000000, 9.999999999998897304E-05 ),
 .UNSPECIFIED. ) ;
#7611 = ADVANCED_FACE ( 'NONE', ( #57719 ), #69240, .T. ) ;
#7612 = EDGE_LOOP ( 'NONE', ( #45086, #26156, #34346, #90365 ) ) ;
#7613 = FACE_OUTER_BOUND ( 'NONE', #90014, .T. ) ;
#7614 = ADVANCED_FACE ( 'NONE', ( #2933 ), #22222, .T. ) ;
#7615 = VECTOR ( 'NONE', #36378, 1000.000000000000000 ) ;
#7617 = EDGE_CURVE ( 'NONE', #86729, #13348, #82529, .T. ) ;
#7616 = DIRECTION ( 'NONE',  ( -0.000000000000000000, 1.000000000000000000, -0.000000000000000000 ) ) ;
#7618 = CARTESIAN_POINT ( 'NONE',  ( -51.53189091124832544, -24.66019654487199730, 8.947790411086117501 ) ) ;
#7620 = ORIENTED_EDGE ( 'NONE', *, *, #31195, .T. ) ;
#7619 = CARTESIAN_POINT ( 'NONE',  ( 20.85495618715548716, -4.085033163991189653, 11.49999999999999645 ) ) ;
#7621 = ORIENTED_EDGE ( 'NONE', *, *, #26435, .T. ) ;
#7622 = CARTESIAN_POINT ( 'NONE',  ( 22.14152233036116257, 1.636640089565777334, -1.500000000000002220 ) ) ;
#7623 = B_SPLINE_CURVE_WITH_KNOTS ( 'NONE', 3,
 ( #93894, #24382, #78649, #24878, #9156, #40116 ),
 .UNSPECIFIED., .F., .F.,
 ( 4, 2, 4 ),
 ( 0.000000000000000000, 0.001380764517854764749, 0.002761529035709529498 ),
 .UNSPECIFIED. ) ;
#7624 = CARTESIAN_POINT ( 'NONE',  ( -18.80638259998596951, 8.471300643254643603, -1.500000000000002220 ) ) ;
#7625 = AXIS2_PLACEMENT_3D ( 'NONE', #24323, #69999, #486 ) ;
#7626 = VERTEX_POINT ( 'NONE', #98750 ) ;
#7627 = ORIENTED_EDGE ( 'NONE', *, *, #28127, .F. ) ;
#7628 = DIRECTION ( 'NONE',  ( 0.000000000000000000, -1.000000000000000000, 0.000000000000000000 ) ) ;
#7629 = CARTESIAN_POINT ( 'NONE',  ( -39.08636289603285974, -25.26169826439894806, 3.855163135067930735 ) ) ;
#7630 = ORIENTED_EDGE ( 'NONE', *, *, #83330, .F. ) ;
#7631 = CIRCLE ( 'NONE', #64383, 1.399999999999999911 ) ;
#7632 = CARTESIAN_POINT ( 'NONE',  ( -91.54631484340760039, -24.51314013834315375, 0.6176544820404143987 ) ) ;
#7633 = AXIS2_PLACEMENT_3D ( 'NONE', #11769, #5160, #42743 ) ;
#7634 = VERTEX_POINT ( 'NONE', #81548 ) ;
#7635 = CARTESIAN_POINT ( 'NONE',  ( -10.34999999999997833, 27.69999999999999929, 0.000000000000000000 ) ) ;
#7636 = LINE ( 'NONE', #93358, #92488 ) ;
#7637 = CARTESIAN_POINT ( 'NONE',  ( -18.77111393065419875, 9.022841878967760465, -1.500000000000002220 ) ) ;
#7638 = EDGE_CURVE ( 'NONE', #85757, #21942, #33350, .T. ) ;
#7639 = CARTESIAN_POINT ( 'NONE',  ( -21.76810506448615712, 0.6044244127108716613, 11.49999999999999645 ) ) ;
#7640 = CARTESIAN_POINT ( 'NONE',  ( 25.20501588964928885, -4.845993637035629575, -10.40696522542261171 ) ) ;
#7641 = CARTESIAN_POINT ( 'NONE',  ( -78.54307297471228821, -24.51419770103157347, 9.386484678747175181 ) ) ;
#7642 = CARTESIAN_POINT ( 'NONE',  ( -22.32441756149717094, -2.617931739244098388, -1.500000000000002220 ) ) ;
#7643 = LINE ( 'NONE', #84759, #27078 ) ;
#7644 = VERTEX_POINT ( 'NONE', #74907 ) ;
#7645 = CARTESIAN_POINT ( 'NONE',  ( -32.30247028140506416, -1.684774720514426560, 27.60502002861223048 ) ) ;
#7646 = CARTESIAN_POINT ( 'NONE',  ( -51.52287095715006870, -29.50248528299804818, 1.056150453629033370 ) ) ;
#7647 = EDGE_CURVE ( 'NONE', #89693, #59659, #5412, .T. ) ;
#7648 = ORIENTED_EDGE ( 'NONE', *, *, #52348, .F. ) ;
#7649 = ORIENTED_EDGE ( 'NONE', *, *, #34556, .F. ) ;
#7650 = ORIENTED_EDGE ( 'NONE', *, *, #24822, .T. ) ;
#7651 = CARTESIAN_POINT ( 'NONE',  ( 16.79701800048795590, -13.18750964578662455, -1.500000000000002220 ) ) ;
#7652 = ORIENTED_EDGE ( 'NONE', *, *, #10898, .F. ) ;
#7653 = CARTESIAN_POINT ( 'NONE',  ( 12.99892964944760543, 16.54660993828877125, 11.49999999999998934 ) ) ;
#7654 = CARTESIAN_POINT ( 'NONE',  ( -30.53944614433371640, -24.75758798069637123, 1.363670884829966123 ) ) ;
#7655 = CARTESIAN_POINT ( 'NONE',  ( -99.52764846858842418, -25.26416398485831749, 3.999772271414141489 ) ) ;
#7656 = CARTESIAN_POINT ( 'NONE',  ( -28.62287095715004881, -23.31957264754183967, 11.44779298504227860 ) ) ;
#7657 = CARTESIAN_POINT ( 'NONE',  ( 2.959355296939036872, -21.81356824310248399, -1.500000000000002220 ) ) ;
#7658 = DIRECTION ( 'NONE',  ( 0.000000000000000000, -0.9999999999976377785, -2.173523156925979128E-06 ) ) ;
#7659 = ORIENTED_EDGE ( 'NONE', *, *, #47736, .F. ) ;
#7660 = CARTESIAN_POINT ( 'NONE',  ( -65.62370081105176212, -25.00182538069147142, 7.747789668545043362 ) ) ;
#7661 = CYLINDRICAL_SURFACE ( 'NONE', #99939, 0.3000000000000016542 ) ;
#7662 = VECTOR ( 'NONE', #65097, 1000.000000000000114 ) ;
#7663 = EDGE_CURVE ( 'NONE', #11406, #49490, #67320, .T. ) ;
#7664 = CARTESIAN_POINT ( 'NONE',  ( 31.61046577166746374, -4.540774708561928108, 26.28065669267635585 ) ) ;
#7665 = CARTESIAN_POINT ( 'NONE',  ( 8.160000000000000142, -10.65233964170348635, -1.621096496867198589 ) ) ;
#7666 = AXIS2_PLACEMENT_3D ( 'NONE', #16403, #77793, #47374 ) ;
#7667 = CARTESIAN_POINT ( 'NONE',  ( -0.04482400408598174318, -22.46971804258298633, 8.370978854367624677 ) ) ;
#7668 = CARTESIAN_POINT ( 'NONE',  ( -12.14505723179402530, 17.47690347785001919, -1.500000000000002220 ) ) ;
#7669 = FACE_OUTER_BOUND ( 'NONE', #14096, .T. ) ;
#7670 = CARTESIAN_POINT ( 'NONE',  ( -107.5594716292221449, -23.48786465467241769, 11.44779295918253936 ) ) ;
#7671 = EDGE_CURVE ( 'NONE', #98207, #39922, #80352, .T. ) ;
#7672 = DIRECTION ( 'NONE',  ( 1.000000000000000000, 0.000000000000000000, 0.000000000000000000 ) ) ;
#7673 = CARTESIAN_POINT ( 'NONE',  ( -5.000686017310577824, -5.876774720514411854, 19.46274624311237034 ) ) ;
#7674 = CARTESIAN_POINT ( 'NONE',  ( -0.06565682164858396841, -22.51586213336150166, -1.500000000000002220 ) ) ;
#7675 = B_SPLINE_SURFACE_WITH_KNOTS ( 'NONE', 3, 3, ( 
 ( #14757, #22359, #99982, #37611 ),
 ( #68563, #90897, #75655, #91886 ),
 ( #45726, #76649, #60961, #59457 ),
 ( #43734, #37109, #91388, #99494 ),
 ( #36116, #30491, #29989, #74668 ),
 ( #53348, #5165, #67577, #68071 ),
 ( #84275, #83280, #29486, #61460 ) ),
 .UNSPECIFIED., .F., .F., .F.,
 ( 4, 3, 4 ),
 ( 4, 4 ),
 ( 0.0004766839783843789826, 0.1029713700210909827, 0.2054660560637975864 ),
 ( 0.4296032809832535659, 0.4308142237037666522 ),
 .UNSPECIFIED. ) ;
#7676 = LINE ( 'NONE', #99506, #87970 ) ;
#7677 = ORIENTED_EDGE ( 'NONE', *, *, #3122, .F. ) ;
#7678 = CARTESIAN_POINT ( 'NONE',  ( -79.71056221673293862, -25.30034170514263892, 4.643640274121591638 ) ) ;
#7679 = CARTESIAN_POINT ( 'NONE',  ( 18.24227566675094181, -7.298356753547692755, 11.49999999999999645 ) ) ;
#7680 = CARTESIAN_POINT ( 'NONE',  ( -55.55620429048338593, -25.00182538069145011, 7.747789668545099317 ) ) ;
#7681 = DIRECTION ( 'NONE',  ( -6.217671308086683664E-14, 0.000000000000000000, -1.000000000000000000 ) ) ;
#7682 = ORIENTED_EDGE ( 'NONE', *, *, #86241, .T. ) ;
#7683 = CARTESIAN_POINT ( 'NONE',  ( -50.52287095715006160, -23.48783264082477018, -1.443836473390095021 ) ) ;
#7684 = CARTESIAN_POINT ( 'NONE',  ( -126.1692191815178319, -25.31364695005282428, 6.500946884335763620 ) ) ;
#7685 = CARTESIAN_POINT ( 'NONE',  ( -90.93633033381745179, -25.06732983082694233, 7.447789526168957508 ) ) ;
#7686 = CIRCLE ( 'NONE', #2861, 2.499999999999995115 ) ;
#7687 = CARTESIAN_POINT ( 'NONE',  ( 19.26447527235507451, 4.322997736827044690, 11.49999999999998934 ) ) ;
#7688 = ORIENTED_EDGE ( 'NONE', *, *, #53630, .T. ) ;
#7689 = CARTESIAN_POINT ( 'NONE',  ( 5.271800844967073907, 6.376774720514426953, -28.56638892015272546 ) ) ;
#7690 = CARTESIAN_POINT ( 'NONE',  ( -70.62287095715001328, -24.92579138211020862, 1.929029949965668456 ) ) ;
#7691 = VECTOR ( 'NONE', #37680, 1000.000000000000114 ) ;
#7692 = ADVANCED_BREP_SHAPE_REPRESENTATION ( '', ( #11338, #37391 ), #11455 ) ;
#7693 = PERSON_AND_ORGANIZATION ( #70597, #27821 ) ;
#7694 = EDGE_LOOP ( 'NONE', ( #47699, #58568, #11614, #54187 ) ) ;
#7695 = CARTESIAN_POINT ( 'NONE',  ( -45.92287095715006728, -23.47593901973090880, -1.443836447538998202 ) ) ;
#7696 = LINE ( 'NONE', #8204, #42593 ) ;
#7697 = CARTESIAN_POINT ( 'NONE',  ( -88.52287095715006160, -24.64965694238407323, 8.947790433994196491 ) ) ;
#7698 = CARTESIAN_POINT ( 'NONE',  ( -69.55126625704997423, -29.50248967467915051, 3.076686136236004732 ) ) ;
#7699 = CARTESIAN_POINT ( 'NONE',  ( -1.488488975859286523, -5.876774720514411854, 19.49847411603315095 ) ) ;
#7700 = VECTOR ( 'NONE', #96393, 1000.000000000000000 ) ;
#7701 = CARTESIAN_POINT ( 'NONE',  ( -56.58953762381673158, -24.65952944569303895, 1.056160979905694575 ) ) ;
#7702 = CARTESIAN_POINT ( 'NONE',  ( -43.58953762381671737, -23.48786465467241058, 11.44779295918255180 ) ) ;
#7703 = CARTESIAN_POINT ( 'NONE',  ( -19.95465934538571062, -0.7993260556091378310, -1.500000000000002220 ) ) ;
#7704 = DIRECTION ( 'NONE',  ( -1.000000000000000000, 0.000000000000000000, 0.000000000000000000 ) ) ;
#7705 = CARTESIAN_POINT ( 'NONE',  ( -51.22152257355241289, -25.31467655261325334, 4.840581831727154061 ) ) ;
#7706 = EDGE_LOOP ( 'NONE', ( #84740, #66784, #19809, #8181 ) ) ;
#7707 = CARTESIAN_POINT ( 'NONE',  ( -79.54332137893563015, -24.51419770103157347, 9.386484678747176957 ) ) ;
#7708 = CARTESIAN_POINT ( 'NONE',  ( -109.7130628311247591, -25.29012770170046309, 3.499763135497069744 ) ) ;
#7709 = CARTESIAN_POINT ( 'NONE',  ( -58.52287095715009713, -24.66019654487199730, 8.947790411086121054 ) ) ;
#7710 = CARTESIAN_POINT ( 'NONE',  ( -108.5228709571500616, -24.64898659630528854, 1.056161002820831474 ) ) ;
#7711 = CARTESIAN_POINT ( 'NONE',  ( -27.85310647731327904, -24.60093890951422679, 1.631228552719281577 ) ) ;
#7712 = CARTESIAN_POINT ( 'NONE',  ( -83.51347087090108801, -23.96119346886880663, -0.6495511937832110227 ) ) ;
#7713 = PLANE ( 'NONE',  #44692 ) ;
#7714 = LINE ( 'NONE', #84332, #43688 ) ;
#7715 = ORIENTED_EDGE ( 'NONE', *, *, #89580, .T. ) ;
#7716 = EDGE_CURVE ( 'NONE', #18728, #55102, #18075, .T. ) ;
#7717 = APPLICATION_CONTEXT ( 'configuration controlled 3d designs of mechanical parts and assemblies' ) ;
#7718 = CARTESIAN_POINT ( 'NONE',  ( -15.58492919356500650, -12.95507736684500699, 11.49999999999998934 ) ) ;
#7719 = CARTESIAN_POINT ( 'NONE',  ( -49.62287095715005592, -23.48786465467241058, 11.44779295918254824 ) ) ;
#7720 = ADVANCED_FACE ( 'NONE', ( #35376 ), #73930, .F. ) ;
#7721 = AXIS2_PLACEMENT_3D ( 'NONE', #89517, #58091, #27631 ) ;
#7722 = LINE ( 'NONE', #92949, #13571 ) ;
#7723 = EDGE_CURVE ( 'NONE', #11910, #73893, #82558, .T. ) ;
#7724 = ORIENTED_EDGE ( 'NONE', *, *, #33510, .F. ) ;
#7725 = LINE ( 'NONE', #36684, #87422 ) ;
#7726 = CARTESIAN_POINT ( 'NONE',  ( 14.24339680280927567, 14.23919408161895284, -1.500000000000002220 ) ) ;
#7727 = ADVANCED_FACE ( 'NONE', ( #52585 ), #14008, .F. ) ;
#7728 = CARTESIAN_POINT ( 'NONE',  ( -19.04630365209304799, -9.011775662611203330, 11.49999999999999645 ) ) ;
#7729 = CARTESIAN_POINT ( 'NONE',  ( -18.93877658415168241, -11.43451605920036052, 11.49999999999998934 ) ) ;
#7730 = EDGE_CURVE ( 'NONE', #38181, #41241, #90152, .T. ) ;
#7731 = CARTESIAN_POINT ( 'NONE',  ( -10.66544979547405347, 17.54311462378693420, 11.49999999999998934 ) ) ;
#7732 = LINE ( 'NONE', #56818, #81946 ) ;
#7733 = CARTESIAN_POINT ( 'NONE',  ( 16.04643365539530109, 3.607965404481768612, -27.87003593022056691 ) ) ;
#7734 = EDGE_LOOP ( 'NONE', ( #15362, #49646, #49473, #73429 ) ) ;
#7735 = CARTESIAN_POINT ( 'NONE',  ( -36.52287095715006870, -29.50248528299804818, 1.056150453629031594 ) ) ;
#7736 = ORIENTED_EDGE ( 'NONE', *, *, #54021, .F. ) ;
#7737 = CARTESIAN_POINT ( 'NONE',  ( -51.62287095715007723, -23.94994826722565762, -0.6494450866342734718 ) ) ;
#7738 = CARTESIAN_POINT ( 'NONE',  ( -85.62287095715008434, -24.83620972994592080, 8.398175272781367440 ) ) ;
#7739 = ORIENTED_EDGE ( 'NONE', *, *, #13208, .F. ) ;
#7740 = ORIENTED_EDGE ( 'NONE', *, *, #30392, .T. ) ;
#7741 = ORIENTED_EDGE ( 'NONE', *, *, #97312, .F. ) ;
#7742 = CARTESIAN_POINT ( 'NONE',  ( -2.188401442307694289, -6.376774720514411854, 19.46153846153846700 ) ) ;
#7743 = CARTESIAN_POINT ( 'NONE',  ( -63.62287095715004881, -24.34917612406837861, 0.1852690917426589035 ) ) ;
#7744 = CARTESIAN_POINT ( 'NONE',  ( 0.3910256410256418569, -6.376774720514420736, 20.67377804487180271 ) ) ;
#7745 = CARTESIAN_POINT ( 'NONE',  ( 4.765357849511589805, 20.07956653139741121, -1.500000000000002220 ) ) ;
#7746 = CARTESIAN_POINT ( 'NONE',  ( -16.54959454218438708, 13.92943311328891554, 11.49999999999999645 ) ) ;
#7747 = ORIENTED_EDGE ( 'NONE', *, *, #64519, .F. ) ;
#7748 = DIRECTION ( 'NONE',  ( 0.000000000000000000, -0.9999999999976377785, -2.173523156925979128E-06 ) ) ;
#7749 = CARTESIAN_POINT ( 'NONE',  ( -57.62287095715004881, -24.50321055353805022, 9.387540953477532923 ) ) ;
#7750 = CARTESIAN_POINT ( 'NONE',  ( 0.3464652362752086434, -22.36268665536068667, -1.500000000000002220 ) ) ;
#7751 = AXIS2_PLACEMENT_3D ( 'NONE', #23650, #54623, #55128 ) ;
#7752 = EDGE_CURVE ( 'NONE', #2928, #31571, #82886, .T. ) ;
#7753 = CARTESIAN_POINT ( 'NONE',  ( -79.47715298469661604, -25.12205682912399141, 6.508607931329533969 ) ) ;
#7754 = CARTESIAN_POINT ( 'NONE',  ( -74.92287095715006728, -23.47596703998600631, 11.44779298504227860 ) ) ;
#7755 = ORIENTED_EDGE ( 'NONE', *, *, #24441, .F. ) ;
#7756 = CARTESIAN_POINT ( 'NONE',  ( -99.53743757535663406, -25.28407026395041868, 4.125266664010103668 ) ) ;
#7757 = CARTESIAN_POINT ( 'NONE',  ( -49.50095828120969799, -24.15620529776627379, 10.23563542870661003 ) ) ;
#7758 = FACE_OUTER_BOUND ( 'NONE', #71089, .T. ) ;
#7759 = CARTESIAN_POINT ( 'NONE',  ( -19.94816486946033507, 6.322790147265108018, 11.49999999999998934 ) ) ;
#7760 = VERTEX_POINT ( 'NONE', #76892 ) ;
#7761 = CARTESIAN_POINT ( 'NONE',  ( -98.62287095715008434, -24.50216790748097040, 0.6166512839513733635 ) ) ;
#7762 = VECTOR ( 'NONE', #70541, 1000.000000000000000 ) ;
#7763 = ORIENTED_EDGE ( 'NONE', *, *, #65280, .F. ) ;
#7764 = CARTESIAN_POINT ( 'NONE',  ( -128.6228709571500417, -23.72773821059536559, 11.05748984161097326 ) ) ;
#7765 = CARTESIAN_POINT ( 'NONE',  ( 20.98173926746349238, 2.650078317256617577, -1.500000000000002220 ) ) ;
#7766 = VERTEX_POINT ( 'NONE', #54585 ) ;
#7767 = LINE ( 'NONE', #93494, #51110 ) ;
#7768 = CARTESIAN_POINT ( 'NONE',  ( -100.4005007646339891, -25.26221318079232603, 7.100843378255928151 ) ) ;
#7769 = CARTESIAN_POINT ( 'NONE',  ( 17.22188757068894915, 13.35947340969901198, 11.49999999999998934 ) ) ;
#7770 = CARTESIAN_POINT ( 'NONE',  ( -7.421417143192116761, -6.376774720514411854, 19.43823095447975291 ) ) ;
#7771 = VECTOR ( 'NONE', #41760, 1000.000000000000000 ) ;
#7772 = CARTESIAN_POINT ( 'NONE',  ( -28.98875734969026396, -5.965225279485572685, 0.1180228001186258285 ) ) ;
#7773 = CARTESIAN_POINT ( 'NONE',  ( -79.91092262079529007, -25.15690873672783923, 6.961915921126503370 ) ) ;
#7774 = CARTESIAN_POINT ( 'NONE',  ( -19.95566455537076678, 8.849265345510103131, -1.500000000000002220 ) ) ;
#7775 = CARTESIAN_POINT ( 'NONE',  ( -30.57287095715004099, -23.47593903913510260, -1.434903445928520149 ) ) ;
#7776 = ORIENTED_EDGE ( 'NONE', *, *, #59886, .F. ) ;
#7777 = DIRECTION ( 'NONE',  ( 0.000000000000000000, -1.000000000000000000, 0.000000000000000000 ) ) ;
#7778 = CARTESIAN_POINT ( 'NONE',  ( -72.52287095715007581, -24.65952944569304606, 1.056160979905697239 ) ) ;
#7779 = DIRECTION ( 'NONE',  ( 0.000000000000000000, 0.000000000000000000, 1.000000000000000000 ) ) ;
#7780 = ORIENTED_EDGE ( 'NONE', *, *, #68614, .T. ) ;
#7781 = VERTEX_POINT ( 'NONE', #77897 ) ;
#7782 = ORIENTED_EDGE ( 'NONE', *, *, #50163, .F. ) ;
#7783 = DIRECTION ( 'NONE',  ( -0.9951627101165078093, 0.000000000000000000, 0.09824042138329590335 ) ) ;
#7784 = CARTESIAN_POINT ( 'NONE',  ( 19.29917393477590437, 8.764703196630867055, 11.49999999999998934 ) ) ;
#7785 = CARTESIAN_POINT ( 'NONE',  ( -94.59719327492638286, -23.73766607897670866, -1.055555164236451349 ) ) ;
#7786 = CARTESIAN_POINT ( 'NONE',  ( -79.53726446675389639, -25.27791906091428231, 7.255560248500635190 ) ) ;
#7787 = CARTESIAN_POINT ( 'NONE',  ( 20.65876267092793128, -4.278775337050348959, -17.77048666223835127 ) ) ;
#7788 = CARTESIAN_POINT ( 'NONE',  ( 32.18888049830260911, 5.126885235861809775, -11.87322522691203908 ) ) ;
#7789 = CARTESIAN_POINT ( 'NONE',  ( 12.39309347844599252, 14.90900669795185252, -1.500000000000002220 ) ) ;
#7790 = B_SPLINE_CURVE_WITH_KNOTS ( 'NONE', 3,
 ( #82381, #58560, #82871, #12860, #43828, #44831, #44334 ),
 .UNSPECIFIED., .F., .F.,
 ( 4, 1, 1, 1, 4 ),
 ( 0.000000000000000000, 0.2835948081386949760, 0.5433948405759660982, 0.7806456291745647036, 1.000000000000000000 ),
 .UNSPECIFIED. ) ;
#7791 = EDGE_CURVE ( 'NONE', #32600, #11368, #38878, .T. ) ;
#7792 = CARTESIAN_POINT ( 'NONE',  ( -41.88608634761866512, -25.31392318313163514, 5.203682277190879724 ) ) ;
#7793 = EDGE_LOOP ( 'NONE', ( #30952, #89238, #1317, #47045 ) ) ;
#7794 = B_SPLINE_CURVE_WITH_KNOTS ( 'NONE', 3,
 ( #9176, #61978, #8687, #22876 ),
 .UNSPECIFIED., .F., .F.,
 ( 4, 4 ),
 ( 0.6802716898399019385, 0.6892781211120175833 ),
 .UNSPECIFIED. ) ;
#7795 = CARTESIAN_POINT ( 'NONE',  ( 11.34002819025610087, 15.78594478779102950, 11.49999999999999645 ) ) ;
#7796 = CARTESIAN_POINT ( 'NONE',  ( -76.52287095715007581, -29.50250786944525672, 11.44777988621623521 ) ) ;
#7797 = CARTESIAN_POINT ( 'NONE',  ( -84.55620429048339304, -24.65952944569304606, 1.056160979905699460 ) ) ;
#7798 = ADVANCED_FACE ( 'NONE', ( #30234 ), #46974, .T. ) ;
#7799 = ORIENTED_EDGE ( 'NONE', *, *, #77588, .F. ) ;
#7800 = PLANE ( 'NONE',  #70111 ) ;
#7801 = DIRECTION ( 'NONE',  ( 3.773278334444167608E-23, -1.000000000000000000, 0.000000000000000000 ) ) ;
#7802 = DIRECTION ( 'NONE',  ( 1.000000000000000000, -0.000000000000000000, 0.000000000000000000 ) ) ;
#7803 = CARTESIAN_POINT ( 'NONE',  ( -93.51856267089354446, -23.73791477778911840, 11.05961554403170410 ) ) ;
#7804 = CARTESIAN_POINT ( 'NONE',  ( -18.14765110722914798, -7.448729197826248871, -1.500000000000002220 ) ) ;
#7805 = B_SPLINE_SURFACE_WITH_KNOTS ( 'NONE', 3, 1, ( 
 ( #64624, #65616 ),
 ( #56499, #41770 ),
 ( #2702, #3701 ),
 ( #87930, #40751 ),
 ( #94532, #18414 ),
 ( #10804, #17919 ),
 ( #27028, #95036 ),
 ( #49886, #71709 ),
 ( #2207, #78792 ),
 ( #96534, #64116 ),
 ( #49382, #25527 ),
 ( #57997, #9800 ),
 ( #25016, #80314 ),
 ( #9290, #72713 ),
 ( #34152, #41259 ),
 ( #71205, #40255 ),
 ( #73213, #18906 ),
 ( #65119, #96039 ),
 ( #26533, #17413 ) ),
 .UNSPECIFIED., .F., .F., .F.,
 ( 4, 1, 1, 1, 1, 1, 1, 1, 1, 1, 1, 1, 1, 1, 1, 1, 4 ),
 ( 2, 2 ),
 ( 0.000000000000000000, 0.07269466619231546023, 0.1413526962021423028, 0.2082288969497897435, 0.2736894576468444917, 0.3380517659755423177, 0.4009220982745038686, 0.4636163844951728397, 0.5278777255384772271, 0.5636262148099121516, 0.6061036626598776955, 0.6545011613018618668, 0.7100543472033251646, 0.7722619378848213367, 0.8412211450824307324, 0.9174702961779349630, 1.000000000000000000 ),
 ( 0.000000000000000000, 1.000000000000000000 ),
 .UNSPECIFIED. ) ;
#7806 = CARTESIAN_POINT ( 'NONE',  ( -117.6228709571500559, -23.48786465467241769, 11.44779295918253759 ) ) ;
#7807 = ORIENTED_EDGE ( 'NONE', *, *, #634, .T. ) ;
#7808 = CARTESIAN_POINT ( 'NONE',  ( 17.73057777116804701, 12.32922261165129285, -1.500000000000002220 ) ) ;
#7809 = DIRECTION ( 'NONE',  ( 1.000000000000000000, 3.773278334444167608E-23, 8.201307833595939069E-29 ) ) ;
#7810 = CARTESIAN_POINT ( 'NONE',  ( -40.58503138813161115, -24.63355581998383670, 0.9682620441943914358 ) ) ;
#7811 = CARTESIAN_POINT ( 'NONE',  ( -65.55620429048339304, -25.00182538069145011, 7.747789668545099317 ) ) ;
#7812 = CARTESIAN_POINT ( 'NONE',  ( -8.497478458550677516, -21.44862750780143656, -1.500000000000002220 ) ) ;
#7813 = CC_DESIGN_PERSON_AND_ORGANIZATION_ASSIGNMENT ( #14295, #76193, ( #5326 ) ) ;
#7814 = DATE_AND_TIME ( #47387, #45714 ) ;
#7815 = CARTESIAN_POINT ( 'NONE',  ( -93.64041077057362372, -23.48783264082477018, -1.443836473390090580 ) ) ;
#7816 = DIRECTION ( 'NONE',  ( 0.9951627101165076983, 0.000000000000000000, 0.09824042138329622254 ) ) ;
#7817 = CARTESIAN_POINT ( 'NONE',  ( -121.5908097038916509, -23.96169478059713498, 10.65365249895717525 ) ) ;
#7818 = CARTESIAN_POINT ( 'NONE',  ( -101.9507253916653440, -25.25287247409162816, 6.236250661346385726 ) ) ;
#7819 = CARTESIAN_POINT ( 'NONE',  ( -111.5321115232925564, -25.10921514312168767, 3.478177734133227172 ) ) ;
#7820 = CARTESIAN_POINT ( 'NONE',  ( -98.52287095715001897, -24.33832256527049154, 0.1851278514138618714 ) ) ;
#7821 = CARTESIAN_POINT ( 'NONE',  ( -111.3157468039189695, -25.18425734897106594, 3.994351493279697518 ) ) ;
#7822 = CARTESIAN_POINT ( 'NONE',  ( 3.219775368129482285, -19.64489633315863770, 11.49999999999998934 ) ) ;
#7823 = FACE_OUTER_BOUND ( 'NONE', #57908, .T. ) ;
#7824 = CARTESIAN_POINT ( 'NONE',  ( -15.99800673754971037, 11.70972097625665675, -1.500000000000002220 ) ) ;
#7825 = AXIS2_PLACEMENT_3D ( 'NONE', #87, #39142, #99029 ) ;
#7826 = CARTESIAN_POINT ( 'NONE',  ( 0.3180806761505774460, -5.876774720514415407, 20.02963804100705403 ) ) ;
#7827 = CARTESIAN_POINT ( 'NONE',  ( 33.96422015159436114, 5.965225279485572685, -7.233236000911337449 ) ) ;
#7828 = CARTESIAN_POINT ( 'NONE',  ( -109.6228709571500559, -29.50247984919015209, -1.443849546365048253 ) ) ;
#7829 = CARTESIAN_POINT ( 'NONE',  ( 18.78520451414993531, -8.817701518030307994, 11.49999999999999645 ) ) ;
#7830 = DIRECTION ( 'NONE',  ( -3.773278334453079618E-23, 0.9999999999976377785, 2.173523156925979975E-06 ) ) ;
#7831 = B_SPLINE_CURVE_WITH_KNOTS ( 'NONE', 3,
 ( #63037, #93959, #24450, #86357 ),
 .UNSPECIFIED., .F., .F.,
 ( 4, 4 ),
 ( 0.6392306918040256969, 0.6402314388447910565 ),
 .UNSPECIFIED. ) ;
#7832 = CARTESIAN_POINT ( 'NONE',  ( -106.6300389066096841, -23.96119346886880308, -0.6495511937832030291 ) ) ;
#7833 = CARTESIAN_POINT ( 'NONE',  ( 17.68435195917723490, -14.24712819257710095, 11.49999999999999645 ) ) ;
#7834 = ORIENTED_EDGE ( 'NONE', *, *, #64947, .F. ) ;
#7835 = DIRECTION ( 'NONE',  ( -3.773278334453079030E-23, 0.9999999999976377785, 2.173523156925979128E-06 ) ) ;
#7836 = B_SPLINE_CURVE_WITH_KNOTS ( 'NONE', 3,
 ( #45480, #46463, #46968, #6408 ),
 .UNSPECIFIED., .F., .F.,
 ( 4, 4 ),
 ( 0.000000000000000000, 9.999999999999592548E-05 ),
 .UNSPECIFIED. ) ;
#7837 = CARTESIAN_POINT ( 'NONE',  ( 5.395440699609677537, -5.965225279485594001, -28.51842087987364138 ) ) ;
#7838 = VERTEX_POINT ( 'NONE', #31238 ) ;
#7839 = CIRCLE ( 'NONE', #74344, 3.549999999999999378 ) ;
#7840 = CARTESIAN_POINT ( 'NONE',  ( -1.055277534996966970, 20.15608268182561247, -1.500000000000002220 ) ) ;
#7841 = DIRECTION ( 'NONE',  ( 0.000000000000000000, 2.173523156925980399E-06, -0.9999999999976378895 ) ) ;
#7842 = FACE_OUTER_BOUND ( 'NONE', #68154, .T. ) ;
#7843 = ORIENTED_EDGE ( 'NONE', *, *, #44196, .T. ) ;
#7844 = EDGE_LOOP ( 'NONE', ( #2309, #70142, #65286, #85719 ) ) ;
#7845 = CARTESIAN_POINT ( 'NONE',  ( -8.160000000000000142, -10.15233964170348457, 0.003711184059992174607 ) ) ;
#7846 = CARTESIAN_POINT ( 'NONE',  ( -16.32851894532483783, 16.03542138455653898, -1.500000000000002220 ) ) ;
#7847 = CARTESIAN_POINT ( 'NONE',  ( -51.15490599271181082, -25.18439718008375650, 3.607700338875335699 ) ) ;
#7848 = CARTESIAN_POINT ( 'NONE',  ( 10.18377579766961283, -19.05927572544859672, -1.500000000000002220 ) ) ;
#7849 = AXIS2_PLACEMENT_3D ( 'NONE', #36301, #60645, #44418 ) ;
#7850 = CARTESIAN_POINT ( 'NONE',  ( -8.676776695296464226, 18.57322330470350735, 2.100000000000000089 ) ) ;
#7851 = ADVANCED_FACE ( 'NONE', ( #16006 ), #62206, .T. ) ;
#7852 = CARTESIAN_POINT ( 'NONE',  ( 18.75483278694074940, -9.228467059531109129, 11.49999999999999645 ) ) ;
#7853 = ORIENTED_EDGE ( 'NONE', *, *, #70527, .T. ) ;
#7854 = CARTESIAN_POINT ( 'NONE',  ( -68.93918693012690824, -25.31612710229039109, 6.184868312322417516 ) ) ;
#7855 = CARTESIAN_POINT ( 'NONE',  ( 4.628415685485613551, -21.52068878818806752, 11.49999999999998934 ) ) ;
#7856 = EDGE_CURVE ( 'NONE', #82017, #50385, #66777, .T. ) ;
#7857 = LINE ( 'NONE', #56051, #67331 ) ;
#7858 = FACE_OUTER_BOUND ( 'NONE', #20505, .T. ) ;
#7859 = EDGE_LOOP ( 'NONE', ( #91303, #10786, #58487, #18127, #84528, #98235 ) ) ;
#7860 = DIRECTION ( 'NONE',  ( 0.000000000000000000, -2.173523156925980399E-06, 0.9999999999976378895 ) ) ;
#7861 = FACE_OUTER_BOUND ( 'NONE', #61913, .T. ) ;
#7862 = EDGE_LOOP ( 'NONE', ( #8187, #56997, #22115, #70143 ) ) ;
#7863 = CARTESIAN_POINT ( 'NONE',  ( -72.50260992981964137, -24.35071581493542681, 9.817618358456032368 ) ) ;
#7864 = EDGE_LOOP ( 'NONE', ( #1820, #51676, #76599, #97515 ) ) ;
#7865 = ORIENTED_EDGE ( 'NONE', *, *, #91115, .T. ) ;
#7866 = CARTESIAN_POINT ( 'NONE',  ( -71.50674337012141280, -24.15620529776628445, 10.23563542870660115 ) ) ;
#7867 = FACE_OUTER_BOUND ( 'NONE', #37829, .T. ) ;
#7869 = EDGE_CURVE ( 'NONE', #43640, #76269, #98180, .T. ) ;
#7868 = CARTESIAN_POINT ( 'NONE',  ( -36.53864600885722780, -24.34968618360933235, 0.1864209137778783110 ) ) ;
#7870 = CARTESIAN_POINT ( 'NONE',  ( 20.35601985306173134, -1.938729116259007679, -1.500000000000002220 ) ) ;
#7871 = EDGE_LOOP ( 'NONE', ( #2626, #71266, #92908, #4929 ) ) ;
#7872 = CARTESIAN_POINT ( 'NONE',  ( -110.6228709571500559, -24.99156045073393173, 7.747789690856161648 ) ) ;
#7873 = CARTESIAN_POINT ( 'NONE',  ( -10.27832545704433365, 4.855524038559839717, 28.80005113363453972 ) ) ;
#7874 = LINE ( 'NONE', #78374, #19145 ) ;
#7875 = CARTESIAN_POINT ( 'NONE',  ( -18.06118310651259407, 13.05043149098080058, 11.49999999999998934 ) ) ;
#7876 = CARTESIAN_POINT ( 'NONE',  ( -4.854568188115255367, -6.376774720514410077, 19.46611907402017394 ) ) ;
#7877 = CARTESIAN_POINT ( 'NONE',  ( -1.845912073933368536, -5.876774720514409189, 19.53740760792477360 ) ) ;
#7878 = EDGE_LOOP ( 'NONE', ( #69927, #26381, #25146, #38208 ) ) ;
#7879 = DIRECTION ( 'NONE',  ( 0.000000000000000000, 0.000000000000000000, 1.000000000000000000 ) ) ;
#7880 = CARTESIAN_POINT ( 'NONE',  ( -29.01900995608618317, -24.63645947259608704, 7.711474408511321599 ) ) ;
#7881 = CARTESIAN_POINT ( 'NONE',  ( -5.744250498300313090, 20.02623800365557472, 11.49999999999998934 ) ) ;
#7882 = ORIENTED_EDGE ( 'NONE', *, *, #83132, .T. ) ;
#7884 = ORIENTED_EDGE ( 'NONE', *, *, #85072, .T. ) ;
#7883 = LINE ( 'NONE', #29230, #32513 ) ;
#7885 = B_SPLINE_SURFACE_WITH_KNOTS ( 'NONE', 3, 3, ( 
 ( #25171, #11452, #10448, #96199 ),
 ( #88089, #56146, #50033, #80968 ),
 ( #71865, #42430, #3858, #2354 ),
 ( #33283, #33793, #79961, #64271 ),
 ( #51024, #6333, #76327, #4842 ),
 ( #6826, #28181, #27685, #35795 ),
 ( #37290, #82457, #36791, #58634 ) ),
 .UNSPECIFIED., .F., .F., .F.,
 ( 4, 3, 4 ),
 ( 4, 4 ),
 ( 0.0004766839783834107900, 0.1029713700210899974, 0.2054660560637965871 ),
 ( 0.8797177824225477227, 0.8811364071469682813 ),
 .UNSPECIFIED. ) ;
#7886 = LINE ( 'NONE', #76390, #82769 ) ;
#7887 = CARTESIAN_POINT ( 'NONE',  ( -14.15979099334852798, -15.53166555317341135, -1.500000000000002220 ) ) ;
#7888 = EDGE_LOOP ( 'NONE', ( #45994, #3919 ) ) ;
#7889 = CARTESIAN_POINT ( 'NONE',  ( 15.00000000000000533, 0.000000000000000000, 0.000000000000000000 ) ) ;
#7890 = LINE ( 'NONE', #99722, #2685 ) ;
#7891 = CARTESIAN_POINT ( 'NONE',  ( 11.16000000000000014, -10.15233964170348457, 0.003711184059992174607 ) ) ;
#7892 = AXIS2_PLACEMENT_3D ( 'NONE', #69447, #15651, #8546 ) ;
#7893 = DIRECTION ( 'NONE',  ( 0.000000000000000000, -1.000000000000000000, 0.000000000000000000 ) ) ;
#7894 = CARTESIAN_POINT ( 'NONE',  ( -92.51514722113715550, -23.96169478059712787, 10.65365249895717525 ) ) ;
#7895 = FACE_OUTER_BOUND ( 'NONE', #37736, .T. ) ;
#7897 = ORIENTED_EDGE ( 'NONE', *, *, #62600, .T. ) ;
#7896 = CARTESIAN_POINT ( 'NONE',  ( -5.848988146064017180, 21.40304369876291446, 11.49999999999999645 ) ) ;
#7898 = CARTESIAN_POINT ( 'NONE',  ( -98.92109765663163046, -25.28792679843457236, 5.825529105375064631 ) ) ;
#7899 = LINE ( 'NONE', #38851, #92662 ) ;
#7900 = VERTEX_POINT ( 'NONE', #84524 ) ;
#7901 = CARTESIAN_POINT ( 'NONE',  ( 21.71957326813621592, -6.446789169762093152, 11.49999999999998934 ) ) ;
#7902 = VECTOR ( 'NONE', #78823, 1000.000000000000114 ) ;
#7904 = ORIENTED_EDGE ( 'NONE', *, *, #57831, .F. ) ;
#7903 = PLANE ( 'NONE',  #95985 ) ;
#7905 = EDGE_CURVE ( 'NONE', #52694, #21736, #57055, .T. ) ;
#7906 = EDGE_LOOP ( 'NONE', ( #97873, #75706, #57661, #27596 ) ) ;
#7907 = AXIS2_PLACEMENT_3D ( 'NONE', #7837, #55026, #16441 ) ;
#7908 = DIRECTION ( 'NONE',  ( 0.000000000000000000, 0.000000000000000000, -1.000000000000000000 ) ) ;
#7909 = ADVANCED_FACE ( 'NONE', ( #68811 ), #31743, .T. ) ;
#7910 = B_SPLINE_CURVE_WITH_KNOTS ( 'NONE', 3,
 ( #38715, #92499, #52458, #48224 ),
 .UNSPECIFIED., .F., .F.,
 ( 4, 4 ),
 ( 0.000000000000000000, 9.999999999998206125E-05 ),
 .UNSPECIFIED. ) ;
#7911 = B_SPLINE_CURVE_WITH_KNOTS ( 'NONE', 3,
 ( #75605, #6613, #99938, #15720, #68027, #52796, #8119, #39061, #68516, #38565 ),
 .UNSPECIFIED., .F., .F.,
 ( 4, 2, 2, 2, 4 ),
 ( 1.734723475976807094E-18, 0.0001825288931172122913, 0.0003650577862344228479, 0.0005475866793516334045, 0.0007301155724688439611 ),
 .UNSPECIFIED. ) ;
#7912 = CARTESIAN_POINT ( 'NONE',  ( -4.233023369943174075, 19.68221892606961987, -1.500000000000002220 ) ) ;
#7913 = DIRECTION ( 'NONE',  ( 0.9994733861282923959, 0.000000000000000000, 0.03244919754393515293 ) ) ;
#7914 = ORIENTED_EDGE ( 'NONE', *, *, #96771, .T. ) ;
#7915 = CARTESIAN_POINT ( 'NONE',  ( 14.97946386127337881, -3.496757005395663587, -28.37921330198104641 ) ) ;
#7916 = CARTESIAN_POINT ( 'NONE',  ( -9.622923231576368863, -20.19340101508991125, -1.500000000000002220 ) ) ;
#7917 = VERTEX_POINT ( 'NONE', #53098 ) ;
#7918 = ORIENTED_EDGE ( 'NONE', *, *, #89295, .F. ) ;
#7919 = CARTESIAN_POINT ( 'NONE',  ( -8.499999999999987566, 18.74999999999999645, 2.100000000000000089 ) ) ;
#7920 = CARTESIAN_POINT ( 'NONE',  ( -94.62560501205011576, -24.51419770103156281, 9.386484678747184063 ) ) ;
#7921 = CARTESIAN_POINT ( 'NONE',  ( -85.52287095715006160, -23.47596703998600631, 11.44779298504228393 ) ) ;
#7922 = FACE_OUTER_BOUND ( 'NONE', #13229, .T. ) ;
#7923 = CARTESIAN_POINT ( 'NONE',  ( -97.25306485665333867, -24.26743686635980879, 0.04347934593174130474 ) ) ;
#7924 = CARTESIAN_POINT ( 'NONE',  ( 18.00893756148942870, 7.586210683597776949, 11.49999999999998934 ) ) ;
#7925 = CARTESIAN_POINT ( 'NONE',  ( -102.5228709571500758, -24.65952944569305316, 1.056160979905702346 ) ) ;
#7926 = CARTESIAN_POINT ( 'NONE',  ( 18.54456287915894563, -10.88813254144886322, -1.500000000000002220 ) ) ;
#7927 = CARTESIAN_POINT ( 'NONE',  ( -36.52287095715006160, -24.34917612406836795, 0.1852690917426497719 ) ) ;
#7928 = DIRECTION ( 'NONE',  ( -0.000000000000000000, 1.000000000000000000, -0.000000000000000000 ) ) ;
#7929 = PLANE ( 'NONE',  #37896 ) ;
#7930 = CARTESIAN_POINT ( 'NONE',  ( 10.34999999999998010, 27.69999999999999929, 2.100000000000000089 ) ) ;
#7931 = CARTESIAN_POINT ( 'NONE',  ( -11.09240565882118368, -20.00103931635436538, -1.500000000000002220 ) ) ;
#7932 = EDGE_CURVE ( 'NONE', #23364, #94830, #54097, .T. ) ;
#7933 = CALENDAR_DATE ( 2026, 9, 10 ) ;
#7934 = DIRECTION ( 'NONE',  ( 0.000000000000000000, 0.9999999999976377785, 2.173523156925979128E-06 ) ) ;
#7935 = CARTESIAN_POINT ( 'NONE',  ( -2.780940648273603433, -5.876774720514414518, 20.02088365235843881 ) ) ;
#7936 = CARTESIAN_POINT ( 'NONE',  ( -10.42242239376218116, -17.14354752861867937, 11.49999999999999645 ) ) ;
#7937 = CARTESIAN_POINT ( 'NONE',  ( 14.23870388848190771, -5.152774720514427642, -26.44223458220801248 ) ) ;
#7938 = PLANE ( 'NONE',  #79203 ) ;
#7939 = CARTESIAN_POINT ( 'NONE',  ( 4.115763745420833786, -5.876774720514403860, 18.20859014712428348 ) ) ;
#7940 = CARTESIAN_POINT ( 'NONE',  ( -103.6228709571500559, -24.64898659630368627, 1.056161002820829697 ) ) ;
#7941 = VERTEX_POINT ( 'NONE', #24122 ) ;
#7942 = PLANE ( 'NONE',  #21851 ) ;
#7943 = CARTESIAN_POINT ( 'NONE',  ( -92.62287095715008434, -24.51283580621364067, 0.6167428607019841413 ) ) ;
#7944 = CARTESIAN_POINT ( 'NONE',  ( -3.653784360050144286, 21.42803128968991544, -1.500000000000002220 ) ) ;
#7945 = EDGE_CURVE ( 'NONE', #48682, #89740, #14511, .T. ) ;
#7946 = CARTESIAN_POINT ( 'NONE',  ( -106.6228709571500559, -24.64965695001469115, 8.947790433994176951 ) ) ;
#7947 = CARTESIAN_POINT ( 'NONE',  ( -17.63651738508609412, 8.604534254076446231, -1.500000000000002220 ) ) ;
#7948 = CARTESIAN_POINT ( 'NONE',  ( -38.55620429048340725, -23.48786465467240347, 11.44779295918255180 ) ) ;
#7949 = CARTESIAN_POINT ( 'NONE',  ( -104.5562042904833930, -23.48786465467241769, 11.44779295918253759 ) ) ;
#7950 = APPROVAL_STATUS ( 'not_yet_approved' ) ;
#7951 = CARTESIAN_POINT ( 'NONE',  ( -91.50656180577668408, -24.51419770103159124, 9.386484678747176957 ) ) ;
#7952 = CARTESIAN_POINT ( 'NONE',  ( 2.745953332610513442, -6.376774720514418959, 21.05053573504278575 ) ) ;
#7953 = CARTESIAN_POINT ( 'NONE',  ( -6.273408026305254737, 19.60348359158234288, 11.49999999999999645 ) ) ;
#7954 = CARTESIAN_POINT ( 'NONE',  ( 2.230654205607476293, -6.505213034913026604E-16, -0.1647943925233646134 ) ) ;
#7955 = CARTESIAN_POINT ( 'NONE',  ( -47.62287095715004881, -23.48783264082478084, -1.443836473390070596 ) ) ;
#7956 = ORIENTED_EDGE ( 'NONE', *, *, #78154, .F. ) ;
#7957 = CARTESIAN_POINT ( 'NONE',  ( -70.32380231474228083, -25.12219144746705268, 7.101635560771297762 ) ) ;
#7958 = CARTESIAN_POINT ( 'NONE',  ( -39.89668141102733756, -25.18430903175396907, 3.440461233786359596 ) ) ;
#7959 = AXIS2_PLACEMENT_3D ( 'NONE', #46053, #8479, #6483 ) ;
#7960 = CARTESIAN_POINT ( 'NONE',  ( -74.52287095715003318, -23.95044443724992078, 10.65354141964648882 ) ) ;
#7961 = CARTESIAN_POINT ( 'NONE',  ( -69.52287095715006160, -24.64965694238407323, 8.947790433994200043 ) ) ;
#7962 = CIRCLE ( 'NONE', #100287, 2.040000000000000036 ) ;
#7963 = ADVANCED_FACE ( 'NONE', ( #45486 ), #791, .T. ) ;
#7964 = CARTESIAN_POINT ( 'NONE',  ( -25.56960729154874556, -24.93063093467123181, 5.760627416161578473 ) ) ;
#7965 = FACE_OUTER_BOUND ( 'NONE', #33857, .T. ) ;
#7966 = CIRCLE ( 'NONE', #4799, 2.499999999999995115 ) ;
#7967 = CARTESIAN_POINT ( 'NONE',  ( -14.58522200957802184, -17.87834940746265389, 11.49999999999999645 ) ) ;
#7968 = CARTESIAN_POINT ( 'NONE',  ( 22.53581206741051446, 3.480912172000575122, -1.500000000000002220 ) ) ;
#7969 = CARTESIAN_POINT ( 'NONE',  ( -74.51178750762115044, -23.96119346886879953, -0.6495511937832119109 ) ) ;
#7970 = AXIS2_PLACEMENT_3D ( 'NONE', #30556, #53911, #5726 ) ;
#7971 = CARTESIAN_POINT ( 'NONE',  ( -105.6228709571500701, -24.82558206586147875, 1.605769216559634005 ) ) ;
#7972 = CARTESIAN_POINT ( 'NONE',  ( -57.52287095715006160, -24.33832256527049154, 0.1851278514138604558 ) ) ;
#7973 = CARTESIAN_POINT ( 'NONE',  ( 22.28251467978060063, -2.329348454117679879, 11.49999999999999645 ) ) ;
#7974 = ORIENTED_EDGE ( 'NONE', *, *, #87345, .T. ) ;
#7975 = AXIS2_PLACEMENT_3D ( 'NONE', #7103, #70004, #93331 ) ;
#7976 = CARTESIAN_POINT ( 'NONE',  ( -69.52287095715006160, -24.65952944569304606, 1.056160979905697239 ) ) ;
#7977 = DIRECTION ( 'NONE',  ( 1.000000000000000000, 0.000000000000000000, 0.000000000000000000 ) ) ;
#7978 = CARTESIAN_POINT ( 'NONE',  ( -9.563806973793814947, 19.74097577964120376, -1.500000000000002220 ) ) ;
#7979 = EDGE_CURVE ( 'NONE', #28755, #59566, #29174, .T. ) ;
#7980 = CARTESIAN_POINT ( 'NONE',  ( -54.55620429048339304, -23.48783264082478084, -1.443836473390070596 ) ) ;
#7981 = CARTESIAN_POINT ( 'NONE',  ( -87.64317292477575450, -23.48786465467240703, 11.44779295918254647 ) ) ;
#7982 = CARTESIAN_POINT ( 'NONE',  ( -121.5228709571500332, -24.50321055353803246, 9.387540953477520489 ) ) ;
#7983 = B_SPLINE_CURVE_WITH_KNOTS ( 'NONE', 3,
 ( #2080, #93396, #25397, #95413, #80189, #55870 ),
 .UNSPECIFIED., .F., .F.,
 ( 4, 2, 4 ),
 ( 0.000000000000000000, 0.001380764517854766484, 0.002761529035709532967 ),
 .UNSPECIFIED. ) ;
#7984 = CARTESIAN_POINT ( 'NONE',  ( -78.50859902716933902, -24.15543982623907127, -0.2315651400026641771 ) ) ;
#7985 = LINE ( 'NONE', #24209, #12827 ) ;
#7986 = ORIENTED_EDGE ( 'NONE', *, *, #39138, .T. ) ;
#7987 = CARTESIAN_POINT ( 'NONE',  ( -18.14515864413662172, 9.488524743509296755, -1.500000000000002220 ) ) ;
#7988 = ORIENTED_EDGE ( 'NONE', *, *, #5593, .F. ) ;
#7989 = ORIENTED_EDGE ( 'NONE', *, *, #17995, .F. ) ;
#7990 = ORIENTED_EDGE ( 'NONE', *, *, #49574, .F. ) ;
#7991 = VERTEX_POINT ( 'NONE', #77399 ) ;
#7992 = CARTESIAN_POINT ( 'NONE',  ( 16.10802587768190008, -16.50329280669357246, -1.500000000000002220 ) ) ;
#7994 = EDGE_CURVE ( 'NONE', #41799, #76858, #7899, .T. ) ;
#7993 = CARTESIAN_POINT ( 'NONE',  ( -5.366453405989236813, 0.000000000000000000, 0.000000000000000000 ) ) ;
#7995 = CARTESIAN_POINT ( 'NONE',  ( 11.01437679584920026, 17.03896688766576517, -1.500000000000002220 ) ) ;
#7996 = ORIENTED_EDGE ( 'NONE', *, *, #62015, .F. ) ;
#7997 = FACE_OUTER_BOUND ( 'NONE', #53383, .T. ) ;
#7998 = CARTESIAN_POINT ( 'NONE',  ( -72.52287095715007581, -23.94994826722564696, -0.6494450866342730277 ) ) ;
#7999 = EDGE_CURVE ( 'NONE', #88644, #90885, #9961, .T. ) ;
#8000 = DIRECTION ( 'NONE',  ( 0.000000000000000000, -0.9967269304714136968, -0.08084198211964954695 ) ) ;
#8001 = CARTESIAN_POINT ( 'NONE',  ( -70.65050961511018102, -23.85016227208580730, -0.8807180028928335291 ) ) ;
#8003 = EDGE_LOOP ( 'NONE', ( #98106, #47085, #32484, #80010, #85909, #68219, #65466, #15153 ) ) ;
#8002 = CARTESIAN_POINT ( 'NONE',  ( -17.55493245422511350, -12.44833567967518029, 11.49999999999999645 ) ) ;
#8004 = CARTESIAN_POINT ( 'NONE',  ( -80.62287095715005592, -29.50248789122583659, 2.256150453626215580 ) ) ;
#8005 = CARTESIAN_POINT ( 'NONE',  ( -61.64838989061559005, -23.73791477778911840, 11.05961554403170943 ) ) ;
#8006 = ORIENTED_EDGE ( 'NONE', *, *, #59194, .F. ) ;
#8007 = CARTESIAN_POINT ( 'NONE',  ( 17.22178217532253086, -11.58000449095910867, -1.500000000000002220 ) ) ;
#8008 = ORIENTED_EDGE ( 'NONE', *, *, #74075, .F. ) ;
#8011 = ORIENTED_EDGE ( 'NONE', *, *, #25631, .T. ) ;
#8010 = VECTOR ( 'NONE', #98162, 1000.000000000000000 ) ;
#8009 = DIRECTION ( 'NONE',  ( -1.334402673828313093E-16, -0.000000000000000000, -1.000000000000000000 ) ) ;
#8012 = CARTESIAN_POINT ( 'NONE',  ( -1.714505518806294145E-16, -4.056774720514426669, 1.399999999999999911 ) ) ;
#8013 = FACE_OUTER_BOUND ( 'NONE', #21134, .T. ) ;
#8014 = ORIENTED_EDGE ( 'NONE', *, *, #4247, .T. ) ;
#8015 = ORIENTED_EDGE ( 'NONE', *, *, #17334, .T. ) ;
#8016 = CARTESIAN_POINT ( 'NONE',  ( 4.886128916861816052, -6.376774720514411854, 19.14085035285361514 ) ) ;
#8017 = CARTESIAN_POINT ( 'NONE',  ( -42.50578598728685620, -23.96169478059712787, 10.65365249895718947 ) ) ;
#8018 = CARTESIAN_POINT ( 'NONE',  ( -65.48565870665615307, -24.92564183028979130, 1.928384488918254869 ) ) ;
#8019 = CARTESIAN_POINT ( 'NONE',  ( 17.26801960494244881, -13.64313956103151071, 11.49999999999999645 ) ) ;
#8020 = FACE_BOUND ( 'NONE', #23826, .T. ) ;
#8021 = CARTESIAN_POINT ( 'NONE',  ( 1.861690257272737847, 22.46465895387273903, -1.500000000000002220 ) ) ;
#8022 = CARTESIAN_POINT ( 'NONE',  ( 8.398332666215036824, -19.25654272332048578, 11.49999999999998934 ) ) ;
#8023 = CARTESIAN_POINT ( 'NONE',  ( 0.3000000000000007661, 0.000000000000000000, 18.50000000000000000 ) ) ;
#8024 = ORIENTED_EDGE ( 'NONE', *, *, #31197, .T. ) ;
#8025 = ORIENTED_EDGE ( 'NONE', *, *, #18839, .F. ) ;
#8026 = CARTESIAN_POINT ( 'NONE',  ( -36.62287095715006302, -24.65952944569303895, 1.056160979905693909 ) ) ;
#8027 = AXIS2_PLACEMENT_3D ( 'NONE', #42198, #18824, #95957 ) ;
#8028 = CARTESIAN_POINT ( 'NONE',  ( -17.63906703526961550, 12.34593017946836291, -1.500000000000002220 ) ) ;
#8029 = EDGE_CURVE ( 'NONE', #40387, #89148, #40360, .T. ) ;
#8030 = CARTESIAN_POINT ( 'NONE',  ( -73.52287095715007581, -29.50248528299804818, 1.056150453629036701 ) ) ;
#8031 = ORIENTED_EDGE ( 'NONE', *, *, #43351, .F. ) ;
#8032 = CARTESIAN_POINT ( 'NONE',  ( 14.48694714638828884, 15.39972936300609341, 11.49999999999998934 ) ) ;
#8033 = CARTESIAN_POINT ( 'NONE',  ( -83.52287095715006160, -24.64898659630367916, 1.056161002820826145 ) ) ;
#8034 = CARTESIAN_POINT ( 'NONE',  ( -51.20402663469029392, -25.03148705966398069, 7.397224223744971461 ) ) ;
#8036 = CARTESIAN_POINT ( 'NONE',  ( -121.6275741054623722, -23.48783264082477018, -1.443836473390087694 ) ) ;
#8035 = AXIS2_PLACEMENT_3D ( 'NONE', #50072, #42468, #28217 ) ;
#8037 = DIRECTION ( 'NONE',  ( -3.773278334453079618E-23, 0.9999999999976377785, 2.173523156925979975E-06 ) ) ;
#8038 = DIRECTION ( 'NONE',  ( -0.000000000000000000, -0.000000000000000000, -1.000000000000000000 ) ) ;
#8039 = CARTESIAN_POINT ( 'NONE',  ( -15.97456084408017674, 15.39233244482803009, -1.500000000000002220 ) ) ;
#8040 = CARTESIAN_POINT ( 'NONE',  ( -81.64116179052845723, -23.73791477778912196, 11.05961554403170943 ) ) ;
#8041 = EDGE_LOOP ( 'NONE', ( #16342, #79500, #45109, #4477 ) ) ;
#8042 = CARTESIAN_POINT ( 'NONE',  ( -51.26059310326842677, -25.31633111157479021, 5.062965957937453965 ) ) ;
#8043 = DIRECTION ( 'NONE',  ( -4.522247983293619802E-39, -2.173523156893721996E-06, 0.9999999999976377785 ) ) ;
#8044 = DIRECTION ( 'NONE',  ( 0.7071067811865513475, -0.7071067811865437980, 0.000000000000000000 ) ) ;
#8045 = VECTOR ( 'NONE', #82900, 1000.000000000000114 ) ;
#8046 = B_SPLINE_CURVE_WITH_KNOTS ( 'NONE', 3,
 ( #31452, #37568, #68520, #99451, #49205, #1518 ),
 .UNSPECIFIED., .F., .F.,
 ( 4, 2, 4 ),
 ( 0.000000000000000000, 0.001380764517853252937, 0.002761529035706505875 ),
 .UNSPECIFIED. ) ;
#8047 = CARTESIAN_POINT ( 'NONE',  ( 5.250998264632098511, 5.356774720514425603, -25.47015671074453280 ) ) ;
#8048 = CARTESIAN_POINT ( 'NONE',  ( 12.29742213896087932, -2.682774720514425670, -27.09288434420517433 ) ) ;
#8049 = VECTOR ( 'NONE', #25464, 1000.000000000000114 ) ;
#8050 = CARTESIAN_POINT ( 'NONE',  ( 18.36381783059253081, 6.383776564742674964, 11.49999999999998934 ) ) ;
#8051 = VECTOR ( 'NONE', #98572, 1000.000000000000114 ) ;
#8052 = CARTESIAN_POINT ( 'NONE',  ( -8.434714792116727367, -19.68496499552307455, 11.49999999999998934 ) ) ;
#8053 = CYLINDRICAL_SURFACE ( 'NONE', #19072, 2.000000000000001776 ) ;
#8054 = CARTESIAN_POINT ( 'NONE',  ( -60.55976160235340444, -23.85049219812968957, 10.88485053497088728 ) ) ;
#8055 = CYLINDRICAL_SURFACE ( 'NONE', #22737, 6.000000000000000888 ) ;
#8056 = CARTESIAN_POINT ( 'NONE',  ( -101.1965263674405691, -25.18440091922403568, 3.665446597890811731 ) ) ;
#8057 = CARTESIAN_POINT ( 'NONE',  ( 9.518656604726816184, -20.62229310799655124, -1.500000000000002220 ) ) ;
#8058 = EDGE_CURVE ( 'NONE', #28096, #79008, #11409, .T. ) ;
#8059 = VECTOR ( 'NONE', #27749, 1000.000000000000000 ) ;
#8060 = EDGE_CURVE ( 'NONE', #28964, #71576, #3865, .T. ) ;
#8061 = CARTESIAN_POINT ( 'NONE',  ( -41.52287095715006870, -29.50248528299804818, 1.056150453629031594 ) ) ;
#8062 = CARTESIAN_POINT ( 'NONE',  ( -127.6228709571500843, -23.73907113216990794, -1.053371485793217932 ) ) ;
#8063 = CARTESIAN_POINT ( 'NONE',  ( 13.50462702941046977, 14.53317887778067252, 11.49999999999999645 ) ) ;
#8064 = CARTESIAN_POINT ( 'NONE',  ( 6.365284455128204399, -6.376774720514413630, 19.73076923076922640 ) ) ;
#8065 = CARTESIAN_POINT ( 'NONE',  ( 8.567893164715615129, -0.1262136116457340251, 3.707288619710387145 ) ) ;
#8066 = EDGE_LOOP ( 'NONE', ( #52467, #74425, #15345, #80773 ) ) ;
#8067 = CARTESIAN_POINT ( 'NONE',  ( -45.62287095715006302, -24.62226745350437795, 0.9660975649728075210 ) ) ;
#8068 = CARTESIAN_POINT ( 'NONE',  ( -6.602379858799704238, -6.376774720514410077, 19.46575348430202723 ) ) ;
#8069 = CARTESIAN_POINT ( 'NONE',  ( 14.61581670307174008, 2.682774720514426559, -27.35847990810646024 ) ) ;
#8070 = CARTESIAN_POINT ( 'NONE',  ( 5.966611984012316405, 20.80180421262142687, 11.49999999999998934 ) ) ;
#8071 = EDGE_CURVE ( 'NONE', #12577, #74051, #33749, .T. ) ;
#8072 = CARTESIAN_POINT ( 'NONE',  ( -56.53341610917590287, -24.66019654487199375, 8.947790411086122830 ) ) ;
#8073 = CARTESIAN_POINT ( 'NONE',  ( 12.19879910451502703, -15.15100395215988449, -1.500000000000002220 ) ) ;
#8074 = ADVANCED_FACE ( 'NONE', ( #56603 ), #71314, .F. ) ;
#8075 = CARTESIAN_POINT ( 'NONE',  ( -55.48263523968800115, -24.83644354573578283, 8.397322867130096569 ) ) ;
#8076 = CARTESIAN_POINT ( 'NONE',  ( -0.3680779360730609406, 19.82951397037014729, 11.49999999999998934 ) ) ;
#8077 = ORIENTED_EDGE ( 'NONE', *, *, #52665, .T. ) ;
#8078 = ADVANCED_FACE ( 'NONE', ( #96152, #80418 ), #9901, .F. ) ;
#8079 = CARTESIAN_POINT ( 'NONE',  ( -5.191926799570463658, 19.71030214607805675, 11.49999999999999645 ) ) ;
#8080 = CARTESIAN_POINT ( 'NONE',  ( -80.49781194617861502, -24.73486907724918282, 1.287355809206963908 ) ) ;
#8081 = LINE ( 'NONE', #972, #414 ) ;
#8082 = B_SPLINE_CURVE_WITH_KNOTS ( 'NONE', 3,
 ( #13331, #90472, #97581, #90965 ),
 .UNSPECIFIED., .F., .F.,
 ( 4, 4 ),
 ( 0.000000000000000000, 9.999999999997510880E-05 ),
 .UNSPECIFIED. ) ;
#8083 = ORIENTED_EDGE ( 'NONE', *, *, #30278, .F. ) ;
#8084 = B_SPLINE_SURFACE_WITH_KNOTS ( 'NONE', 3, 3, ( 
 ( #86587, #78965, #23170, #24678 ),
 ( #15074, #48039, #84584, #46042 ),
 ( #8964, #39419, #23677, #85085 ),
 ( #24184, #93694, #61770, #93192 ),
 ( #70368, #17074, #76963, #15570 ),
 ( #55160, #16566, #92689, #85584 ),
 ( #855, #37919, #7456, #39913 ),
 ( #38413, #32302, #16067, #68867 ),
 ( #47040, #99787, #69366, #30295 ),
 ( #61274, #92195, #77955, #22672 ) ),
 .UNSPECIFIED., .F., .F., .F.,
 ( 4, 3, 3, 4 ),
 ( 4, 4 ),
 ( 0.7022005934544808259, 0.7765311282028795059, 0.8508616629512780749, 0.9995227324480753239 ),
 ( 0.04949997043182981921, 0.05054219703631999960 ),
 .UNSPECIFIED. ) ;
#8085 = CARTESIAN_POINT ( 'NONE',  ( 29.73860345376319003, 1.477225279485574028, -1.272392034746785860 ) ) ;
#8086 = DIRECTION ( 'NONE',  ( 1.000000000000000000, 3.773278334444166432E-23, 8.201307841325785021E-29 ) ) ;
#8087 = CARTESIAN_POINT ( 'NONE',  ( -49.53270844027763786, -25.31601842583603457, 5.057855796360450462 ) ) ;
#8088 = CARTESIAN_POINT ( 'NONE',  ( -128.6228709571500417, -24.34917612406839993, 0.1852690917426724204 ) ) ;
#8089 = CARTESIAN_POINT ( 'NONE',  ( -15.87499999999997868, 0.000000000000000000, 1.249999999999997558 ) ) ;
#8090 = CARTESIAN_POINT ( 'NONE',  ( 12.55954966114946458, -15.69740789531843461, 11.49999999999998934 ) ) ;
#8091 = B_SPLINE_CURVE_WITH_KNOTS ( 'NONE', 3,
 ( #100038, #99544, #28555, #68622, #45293, #30043 ),
 .UNSPECIFIED., .F., .F.,
 ( 4, 2, 4 ),
 ( 1.570887131794952276E-05, 0.001396322306279765193, 0.002776935741241580609 ),
 .UNSPECIFIED. ) ;
#8092 = EDGE_CURVE ( 'NONE', #59704, #59375, #76429, .T. ) ;
#8093 = DIRECTION ( 'NONE',  ( -3.773278334453079030E-23, 0.9999999999976377785, 2.173523156925979128E-06 ) ) ;
#8094 = ORIENTED_EDGE ( 'NONE', *, *, #12125, .T. ) ;
#8095 = CARTESIAN_POINT ( 'NONE',  ( 0.1334620785917008390, -8.769264156269322541, -9.000000000000000000 ) ) ;
#8096 = CARTESIAN_POINT ( 'NONE',  ( 16.30191990219073972, -16.09819076282585826, 11.49999999999999645 ) ) ;
#8097 = CARTESIAN_POINT ( 'NONE',  ( -17.38503614929206265, -14.63273120789127013, -1.500000000000002220 ) ) ;
#8098 = EDGE_LOOP ( 'NONE', ( #83327, #35208, #41224, #32020 ) ) ;
#8099 = FACE_OUTER_BOUND ( 'NONE', #74777, .T. ) ;
#8100 = DIRECTION ( 'NONE',  ( 0.000000000000000000, -2.173523156925980399E-06, 0.9999999999976378895 ) ) ;
#8101 = CARTESIAN_POINT ( 'NONE',  ( -39.58729228046302495, -25.24755811718921095, 3.712701613397900058 ) ) ;
#8102 = LINE ( 'NONE', #85223, #93441 ) ;
#8103 = AXIS2_PLACEMENT_3D ( 'NONE', #19154, #50123, #81064 ) ;
#8104 = ADVANCED_FACE ( 'NONE', ( #57103 ), #88040, .F. ) ;
#8105 = B_SPLINE_CURVE_WITH_KNOTS ( 'NONE', 3,
 ( #2183, #94510, #78268, #24991, #25502, #9774, #2679, #33618, #35623, #73679, #11276, #58468, #89403, #49360, #26511, #26000, #18390, #89901, #81289 ),
 .UNSPECIFIED., .F., .F.,
 ( 4, 1, 1, 1, 1, 1, 1, 1, 1, 1, 1, 1, 1, 1, 1, 1, 4 ),
 ( 0.000000000000000000, 0.06523080374203017728, 0.1284048960032230235, 0.1900670715964783708, 0.2509433657682806351, 0.3115458328521427123, 0.3728628021568293205, 0.4350236738562381356, 0.4990717247070431406, 0.5630910750496627148, 0.6255101063303755149, 0.6866800359296488798, 0.7472825030135124003, 0.8085634952159584943, 0.8707421035159862432, 0.9343409515059130088, 1.000000000000000000 ),
 .UNSPECIFIED. ) ;
#8106 = DIRECTION ( 'NONE',  ( -0.9994733861282923959, 0.000000000000000000, -0.03244919754393515293 ) ) ;
#8107 = EDGE_CURVE ( 'NONE', #89671, #82714, #94592, .T. ) ;
#8108 = FACE_OUTER_BOUND ( 'NONE', #33456, .T. ) ;
#8109 = ORIENTED_EDGE ( 'NONE', *, *, #52984, .F. ) ;
#8110 = VECTOR ( 'NONE', #4144, 1000.000000000000000 ) ;
#8111 = CARTESIAN_POINT ( 'NONE',  ( 2.554409723529738052, 20.22502395925995700, 11.49999999999998934 ) ) ;
#8112 = ORIENTED_EDGE ( 'NONE', *, *, #22043, .F. ) ;
#8113 = B_SPLINE_CURVE_WITH_KNOTS ( 'NONE', 3,
 ( #22651, #17429, #2223, #25545 ),
 .UNSPECIFIED., .F., .F.,
 ( 4, 4 ),
 ( 0.000000000000000000, 9.999999999998897304E-05 ),
 .UNSPECIFIED. ) ;
#8114 = CARTESIAN_POINT ( 'NONE',  ( -15.63304604236160067, -16.83380969201049382, 11.49999999999998934 ) ) ;
#8115 = EDGE_CURVE ( 'NONE', #86861, #41039, #49991, .T. ) ;
#8116 = CARTESIAN_POINT ( 'NONE',  ( -103.5895376238167245, -23.48783264082478794, -1.443836473390062158 ) ) ;
#8117 = EDGE_LOOP ( 'NONE', ( #70903, #7142, #71057, #50188, #82681, #26718, #75362, #32837, #42674, #43108, #29124, #73513, #62446, #58751, #13255, #60915, #8387, #75511, #73530, #31749 ) ) ;
#8118 = CIRCLE ( 'NONE', #67882, 6.000000000000000888 ) ;
#8119 = CARTESIAN_POINT ( 'NONE',  ( -101.3556973279126368, -25.18955741793521597, 6.678808583419815648 ) ) ;
#8120 = EDGE_CURVE ( 'NONE', #7991, #78336, #79199, .T. ) ;
#8121 = CARTESIAN_POINT ( 'NONE',  ( -80.71993455722410715, -25.13732816275518900, 7.077603319917434632 ) ) ;
#8122 = ADVANCED_FACE ( 'NONE', ( #80918 ), #48484, .F. ) ;
#8123 = VECTOR ( 'NONE', #1944, 1000.000000000000000 ) ;
#8124 = CARTESIAN_POINT ( 'NONE',  ( -111.5228709571500616, -24.33927499327855770, 9.819080762295804732 ) ) ;
#8126 = VERTEX_POINT ( 'NONE', #52471 ) ;
#8125 = CARTESIAN_POINT ( 'NONE',  ( 18.88549913130557556, 9.949676122998861061, 11.49999999999999645 ) ) ;
#8127 = AXIS2_PLACEMENT_3D ( 'NONE', #37183, #66668, #75238 ) ;
#8128 = ORIENTED_EDGE ( 'NONE', *, *, #17465, .T. ) ;
#8129 = CARTESIAN_POINT ( 'NONE',  ( 22.20243239366838850, -0.07139729354238147363, -1.500000000000002220 ) ) ;
#8130 = B_SPLINE_CURVE_WITH_KNOTS ( 'NONE', 3,
 ( #79575, #85185, #20165, #66865, #87694, #80573 ),
 .UNSPECIFIED., .F., .F.,
 ( 4, 2, 4 ),
 ( 6.384118678611318703E-06, 0.001386860460828374551, 0.002767336802978137555 ),
 .UNSPECIFIED. ) ;
#8131 = CARTESIAN_POINT ( 'NONE',  ( 17.37421522561336928, 11.14841987994331696, -1.500000000000002220 ) ) ;
#8133 = ORIENTED_EDGE ( 'NONE', *, *, #79102, .T. ) ;
#8132 = AXIS2_PLACEMENT_3D ( 'NONE', #97877, #90282, #11650 ) ;
#8134 = ORIENTED_EDGE ( 'NONE', *, *, #24360, .F. ) ;
#8135 = CARTESIAN_POINT ( 'NONE',  ( -109.3320997930167806, -25.27682792883151919, 5.169840796200587008 ) ) ;
#8136 = EDGE_CURVE ( 'NONE', #18610, #20866, #86385, .T. ) ;
#8137 = CARTESIAN_POINT ( 'NONE',  ( -71.72827525033231666, -25.11539253604531297, 2.804427796191110378 ) ) ;
#8138 = EDGE_LOOP ( 'NONE', ( #64333, #91377, #20112, #10890, #74499, #98495, #44932, #12136, #87011 ) ) ;
#8139 = CARTESIAN_POINT ( 'NONE',  ( -49.52581182275615390, -25.18689758514837251, 6.769651850996265985 ) ) ;
#8140 = ORIENTED_EDGE ( 'NONE', *, *, #36921, .T. ) ;
#8141 = CARTESIAN_POINT ( 'NONE',  ( -56.58953762381672448, -24.64965694238407323, 8.947790433994656567 ) ) ;
#8142 = PLANE ( 'NONE',  #27689 ) ;
#8143 = CARTESIAN_POINT ( 'NONE',  ( 5.792680761630559338, -19.98616098212858105, -1.500000000000002220 ) ) ;
#8144 = CARTESIAN_POINT ( 'NONE',  ( -3.523925741820590929, 21.50064390955241578, 11.49999999999999645 ) ) ;
#8145 = DIRECTION ( 'NONE',  ( -3.773278334444166432E-23, 1.000000000000000000, 0.000000000000000000 ) ) ;
#8146 = CARTESIAN_POINT ( 'NONE',  ( -100.3501680573226906, -25.03346342031885641, 7.560302575324243435 ) ) ;
#8147 = CARTESIAN_POINT ( 'NONE',  ( -11.43049785330379997, -19.34545768653811493, 11.49999999999998934 ) ) ;
#8148 = CARTESIAN_POINT ( 'NONE',  ( -34.52287095715006160, -24.64898659630366851, 1.056161002820817485 ) ) ;
#8149 = B_SPLINE_CURVE_WITH_KNOTS ( 'NONE', 3,
 ( #33393, #39516, #78555, #94291, #17674, #70468 ),
 .UNSPECIFIED., .F., .F.,
 ( 4, 2, 4 ),
 ( 0.000000000000000000, 0.5000000000000000000, 1.000000000000000000 ),
 .UNSPECIFIED. ) ;
#8150 = CARTESIAN_POINT ( 'NONE',  ( -109.6228709571500559, -29.50250786944525672, 11.44777988621622988 ) ) ;
#8151 = CARTESIAN_POINT ( 'NONE',  ( 4.400426145423703694, -5.876774720514425177, 21.64763382324305852 ) ) ;
#8152 = ORIENTED_EDGE ( 'NONE', *, *, #23929, .F. ) ;
#8153 = EDGE_LOOP ( 'NONE', ( #84540, #69806, #83811, #87875, #7904 ) ) ;
#8154 = EDGE_LOOP ( 'NONE', ( #38792, #57689 ) ) ;
#8155 = CARTESIAN_POINT ( 'NONE',  ( 19.36035776617087123, -9.008237321879198234, -1.500000000000002220 ) ) ;
#8156 = ORIENTED_EDGE ( 'NONE', *, *, #45300, .T. ) ;
#8157 = CARTESIAN_POINT ( 'NONE',  ( -19.04630365209304799, -9.011775662611203330, 11.49999999999998934 ) ) ;
#8158 = CARTESIAN_POINT ( 'NONE',  ( -30.47189565061154326, -23.47430189329197248, -1.443836490256471983 ) ) ;
#8159 = CARTESIAN_POINT ( 'NONE',  ( 16.79105032741591330, -10.77411451815220822, -1.500000000000002220 ) ) ;
#8160 = DIRECTION ( 'NONE',  ( 0.000000000000000000, 0.000000000000000000, -1.000000000000000000 ) ) ;
#8161 = CARTESIAN_POINT ( 'NONE',  ( 2.905029696106983916, -6.376774720514415407, 20.12486936895525957 ) ) ;
#8162 = CARTESIAN_POINT ( 'NONE',  ( -8.471812324360341151, -20.26817064352238162, -1.500000000000002220 ) ) ;
#8163 = FACE_OUTER_BOUND ( 'NONE', #95226, .T. ) ;
#8164 = ORIENTED_EDGE ( 'NONE', *, *, #48385, .T. ) ;
#8165 = CARTESIAN_POINT ( 'NONE',  ( -65.57704458058132957, -25.00182538069147142, 7.747789668545043362 ) ) ;
#8166 = CARTESIAN_POINT ( 'NONE',  ( -10.34999999999997833, 22.00000000000000000, 0.000000000000000000 ) ) ;
#8167 = CARTESIAN_POINT ( 'NONE',  ( -6.911038104174170194, -19.68591361114308214, 11.49999999999999645 ) ) ;
#8168 = CARTESIAN_POINT ( 'NONE',  ( 31.62080439023052492, -4.380055315099236957, 26.73348078282562668 ) ) ;
#8169 = CARTESIAN_POINT ( 'NONE',  ( -125.5228709571500900, -24.91570333825475458, 8.075032458260897883 ) ) ;
#8170 = MANIFOLD_SOLID_BREP ( 'Aynalama1', #37124 ) ;
#8171 = CARTESIAN_POINT ( 'NONE',  ( -30.60531187098371575, -24.66542028447632262, 8.909134979017295564 ) ) ;
#8172 = CARTESIAN_POINT ( 'NONE',  ( 19.49461108348020133, 8.573440864381753457, 11.49999999999998934 ) ) ;
#8173 = DIRECTION ( 'NONE',  ( 0.000000000000000000, 1.000000000000000000, 0.000000000000000000 ) ) ;
#8174 = CARTESIAN_POINT ( 'NONE',  ( -107.6262921065285241, -24.35071581493543746, 9.817618358456021710 ) ) ;
#8175 = AXIS2_PLACEMENT_3D ( 'NONE', #27230, #12493, #60185 ) ;
#8176 = DIRECTION ( 'NONE',  ( 0.000000000000000000, 0.000000000000000000, 1.000000000000000000 ) ) ;
#8177 = CARTESIAN_POINT ( 'NONE',  ( -5.514838905578028694, -5.876774720514410966, 19.81240905262003338 ) ) ;
#8178 = CARTESIAN_POINT ( 'NONE',  ( -15.68175098440391402, -16.16561365185589594, -1.500000000000002220 ) ) ;
#8179 = EDGE_CURVE ( 'NONE', #27420, #54063, #5178, .T. ) ;
#8180 = CARTESIAN_POINT ( 'NONE',  ( -129.5895376238167387, -24.66019654487200086, 8.947790411086117501 ) ) ;
#8181 = ORIENTED_EDGE ( 'NONE', *, *, #91785, .T. ) ;
#8182 = EDGE_CURVE ( 'NONE', #47263, #58944, #89529, .T. ) ;
#8183 = CARTESIAN_POINT ( 'NONE',  ( -104.5228709571500758, -23.48786465467241769, 11.44779295918254114 ) ) ;
#8184 = CARTESIAN_POINT ( 'NONE',  ( 19.16472379399037251, -4.548241762842377689, 11.49999999999999645 ) ) ;
#8185 = CARTESIAN_POINT ( 'NONE',  ( -125.6228709571500559, -24.63287334234178161, 0.9662140553045557301 ) ) ;
#8186 = LINE ( 'NONE', #32523, #41553 ) ;
#8187 = ORIENTED_EDGE ( 'NONE', *, *, #38850, .F. ) ;
#8188 = EDGE_CURVE ( 'NONE', #44155, #96177, #54944, .T. ) ;
#8189 = DIRECTION ( 'NONE',  ( -1.000000000000000000, -0.000000000000000000, -0.000000000000000000 ) ) ;
#8190 = DIRECTION ( 'NONE',  ( 0.000000000000000000, 0.000000000000000000, 1.000000000000000000 ) ) ;
#8191 = CARTESIAN_POINT ( 'NONE',  ( -89.90116859791649517, -25.30572777988223976, 5.920366768842380445 ) ) ;
#8192 = ADVANCED_FACE ( 'NONE', ( #28136 ), #3811, .F. ) ;
#8193 = ADVANCED_FACE ( 'NONE', ( #28628 ), #35253, .T. ) ;
#8194 = FACE_OUTER_BOUND ( 'NONE', #93674, .T. ) ;
#8195 = CARTESIAN_POINT ( 'NONE',  ( 12.09797951242163805, 15.59582292391970704, 11.49999999999998934 ) ) ;
#8196 = ORIENTED_EDGE ( 'NONE', *, *, #55698, .F. ) ;
#8198 = ADVANCED_FACE ( 'NONE', ( #42872 ), #90522, .T. ) ;
#8197 = VECTOR ( 'NONE', #75880, 1000.000000000000000 ) ;
#8199 = CARTESIAN_POINT ( 'NONE',  ( -109.3903331153901206, -25.27100251396372244, 3.960067624998357960 ) ) ;
#8200 = CIRCLE ( 'NONE', #48712, 1.399999999999988143 ) ;
#8201 = PERSON_AND_ORGANIZATION_ROLE ( 'classification_officer' ) ;
#8202 = ORIENTED_EDGE ( 'NONE', *, *, #21124, .T. ) ;
#8203 = CARTESIAN_POINT ( 'NONE',  ( -81.42380231474228935, -29.50249428492551829, 5.197779886230994073 ) ) ;
#8204 = CARTESIAN_POINT ( 'NONE',  ( -89.62287095715004170, -29.50248528299804818, 1.056150453629040253 ) ) ;
#8205 = CARTESIAN_POINT ( 'NONE',  ( -69.56655373305933665, -25.28935879948601695, 5.635482696873745923 ) ) ;
#8206 = CARTESIAN_POINT ( 'NONE',  ( 30.53060340732036337, 1.477225279485574028, -8.442346167188910400 ) ) ;
#8207 = DIRECTION ( 'NONE',  ( 1.000000000000000000, 3.773278334444167608E-23, 8.201307810031787050E-29 ) ) ;
#8208 = B_SPLINE_CURVE_WITH_KNOTS ( 'NONE', 3,
 ( #44174, #7099, #75105, #68013, #98942, #5602, #30436, #36546, #67513, #52283, #60412, #91332, #29933, #99927, #52785, #21809, #83722, #14199, #6603 ),
 .UNSPECIFIED., .F., .F.,
 ( 4, 1, 1, 1, 1, 1, 1, 1, 1, 1, 1, 1, 1, 1, 1, 1, 4 ),
 ( 0.000000000000000000, 0.06796237149445635839, 0.1332834028675231042, 0.1978352977570558280, 0.2608919865309880515, 0.3233765044831760083, 0.3863500754690888384, 0.4496377310517142845, 0.5147953269783583918, 0.5792399132410295248, 0.6418141777582890839, 0.7013585647860598460, 0.7607267659857199771, 0.8192220679243895631, 0.8787161693846299304, 0.9381473540533086242, 1.000000000000000000 ),
 .UNSPECIFIED. ) ;
#8209 = CARTESIAN_POINT ( 'NONE',  ( -94.58953762381672448, -24.65952944569304961, 1.056160979905703678 ) ) ;
#8210 = CARTESIAN_POINT ( 'NONE',  ( -43.62287095715004170, -23.48786465467241058, 11.44779295918255180 ) ) ;
#8211 = CARTESIAN_POINT ( 'NONE',  ( -18.81269933604069067, 6.858547123926768130, -1.500000000000002220 ) ) ;
#8212 = EDGE_CURVE ( 'NONE', #42958, #11783, #50106, .T. ) ;
#8213 = CARTESIAN_POINT ( 'NONE',  ( -100.0924861708260636, -25.10935045777317498, 2.869718873696385675 ) ) ;
#8214 = PLANE ( 'NONE',  #43554 ) ;
#8215 = ORIENTED_EDGE ( 'NONE', *, *, #93039, .F. ) ;
#8216 = EDGE_CURVE ( 'NONE', #6907, #54320, #11904, .T. ) ;
#8217 = CARTESIAN_POINT ( 'NONE',  ( -79.55429133993682456, -23.96169478059713143, 10.65365249895718058 ) ) ;
#8218 = CARTESIAN_POINT ( 'NONE',  ( -110.2348554541972874, -25.18430154389852049, 3.296590759564009154 ) ) ;
#8219 = CARTESIAN_POINT ( 'NONE',  ( -35.54983106724529307, -24.15503026093914940, -0.2815557561904327155 ) ) ;
#8220 = CARTESIAN_POINT ( 'NONE',  ( -39.56136241089613748, -25.30385213834873781, 5.536731319770037629 ) ) ;
#8221 = B_SPLINE_CURVE_WITH_KNOTS ( 'NONE', 3,
 ( #5447, #60749, #36898, #91671 ),
 .UNSPECIFIED., .F., .F.,
 ( 4, 4 ),
 ( 0.1298786676550697794, 0.1388850989271851466 ),
 .UNSPECIFIED. ) ;
#8222 = FACE_OUTER_BOUND ( 'NONE', #71721, .T. ) ;
#8223 = CARTESIAN_POINT ( 'NONE',  ( 14.83405752585509596, 4.881907540129173384, -27.54622755360215791 ) ) ;
#8224 = ADVANCED_FACE ( 'NONE', ( #83402 ), #21000, .T. ) ;
#8225 = CARTESIAN_POINT ( 'NONE',  ( -3.103301570662693187, -5.876774720514418071, 20.14409848895067512 ) ) ;
#8226 = CARTESIAN_POINT ( 'NONE',  ( -40.52287095715006160, -24.62285846331440098, 9.038163153548140372 ) ) ;
#8227 = ORIENTED_EDGE ( 'NONE', *, *, #40647, .T. ) ;
#8228 = CARTESIAN_POINT ( 'NONE',  ( 20.23688964843749005, 1.552196809742036221, -1.500000000000002220 ) ) ;
#8229 = DIRECTION ( 'NONE',  ( -0.8254963646400337307, 1.226752628532750849E-06, -0.5644074343633185276 ) ) ;
#8230 = CARTESIAN_POINT ( 'NONE',  ( -99.62287095715001328, -24.33832256526968862, 0.1851278514119927554 ) ) ;
#8232 = VERTEX_POINT ( 'NONE', #43861 ) ;
#8231 = ADVANCED_FACE ( 'NONE', ( #50980 ), #82902, .F. ) ;
#8233 = DIRECTION ( 'NONE',  ( 0.000000000000000000, 0.000000000000000000, -1.000000000000000000 ) ) ;
#8234 = CARTESIAN_POINT ( 'NONE',  ( 17.77915467781788195, 9.360003092772107181, -1.500000000000002220 ) ) ;
#8235 = CARTESIAN_POINT ( 'NONE',  ( -13.19772682967519195, -16.48504770976277101, 11.49999999999999645 ) ) ;
#8236 = CARTESIAN_POINT ( 'NONE',  ( 21.87352179494074633, -3.179377960941109915, -1.500000000000002220 ) ) ;
#8238 = EDGE_CURVE ( 'NONE', #2872, #95000, #91019, .T. ) ;
#8237 = VECTOR ( 'NONE', #58203, 1000.000000000000114 ) ;
#8239 = CARTESIAN_POINT ( 'NONE',  ( 11.66944253441096002, 16.90307425063352298, -1.500000000000002220 ) ) ;
#8240 = CARTESIAN_POINT ( 'NONE',  ( -60.58607451518173548, -24.63355581998385446, 0.9682620441943891043 ) ) ;
#8241 = ORIENTED_EDGE ( 'NONE', *, *, #31626, .F. ) ;
#8242 = DIRECTION ( 'NONE',  ( -0.4771587602595986910, -0.8788171126619707119, 0.000000000000000000 ) ) ;
#8243 = VERTEX_POINT ( 'NONE', #21492 ) ;
#8244 = CARTESIAN_POINT ( 'NONE',  ( -88.52287095715006160, -24.64965694238407323, 8.947790433994196491 ) ) ;
#8245 = CARTESIAN_POINT ( 'NONE',  ( -70.52287095715009002, -24.82576562948882781, 8.398263436605597931 ) ) ;
#8246 = ORIENTED_EDGE ( 'NONE', *, *, #10282, .F. ) ;
#8247 = ORIENTED_EDGE ( 'NONE', *, *, #6415, .T. ) ;
#8248 = ORIENTED_EDGE ( 'NONE', *, *, #44167, .F. ) ;
#8249 = DIRECTION ( 'NONE',  ( 0.000000000000000000, -0.9999999999976377785, -2.173523156925979128E-06 ) ) ;
#8250 = CARTESIAN_POINT ( 'NONE',  ( -49.41210582477036439, -25.09381984642397612, 7.261948667840803395 ) ) ;
#8251 = CARTESIAN_POINT ( 'NONE',  ( 0.3849403830293018358, -6.376774720514418959, 20.45311193189268906 ) ) ;
#8252 = CARTESIAN_POINT ( 'NONE',  ( -3.087264924507187924, 20.40197043678811539, -1.500000000000002220 ) ) ;
#8253 = EDGE_CURVE ( 'NONE', #55098, #45187, #13887, .T. ) ;
#8254 = CARTESIAN_POINT ( 'NONE',  ( 10.18377579766961283, -19.05927572544859672, 11.49999999999999645 ) ) ;
#8255 = ORIENTED_EDGE ( 'NONE', *, *, #8996, .T. ) ;
#8256 = FACE_OUTER_BOUND ( 'NONE', #4281, .T. ) ;
#8257 = CARTESIAN_POINT ( 'NONE',  ( 3.116263380642223968, -5.876774720514401196, 18.40799819116699609 ) ) ;
#8258 = CARTESIAN_POINT ( 'NONE',  ( 6.497064355747536268, 21.42967291005575348, -1.500000000000002220 ) ) ;
#8259 = CARTESIAN_POINT ( 'NONE',  ( -67.22287095715007865, -23.47596703998600276, 11.44779298504227860 ) ) ;
#8260 = CARTESIAN_POINT ( 'NONE',  ( -5.891025641025637860, -5.876774720514426953, 21.75000000000000711 ) ) ;
#8261 = ORIENTED_EDGE ( 'NONE', *, *, #37521, .T. ) ;
#8262 = CARTESIAN_POINT ( 'NONE',  ( -58.58953762381673158, -24.65952944569304250, 1.056160979905698127 ) ) ;
#8263 = AXIS2_PLACEMENT_3D ( 'NONE', #99627, #46361, #54982 ) ;
#8264 = CARTESIAN_POINT ( 'NONE',  ( -35.49720035677762553, -24.15602025860895452, 10.28564288303536856 ) ) ;
#8265 = CARTESIAN_POINT ( 'NONE',  ( -15.06743543786183714, 14.52697759824333090, 11.49999999999998934 ) ) ;
#8266 = ORIENTED_EDGE ( 'NONE', *, *, #24245, .F. ) ;
#8267 = DIRECTION ( 'NONE',  ( 0.000000000000000000, -0.9999999999976377785, -2.173523156925979128E-06 ) ) ;
#8268 = VERTEX_POINT ( 'NONE', #27641 ) ;
#8269 = DIRECTION ( 'NONE',  ( 0.000000000000000000, -2.173523156925980399E-06, 0.9999999999976378895 ) ) ;
#8270 = CARTESIAN_POINT ( 'NONE',  ( -15.68702345270385834, -14.21367052863537417, -1.500000000000002220 ) ) ;
#8271 = ORIENTED_EDGE ( 'NONE', *, *, #19553, .F. ) ;
#8272 = CARTESIAN_POINT ( 'NONE',  ( -50.58898002243636682, -24.52300882791530157, 0.6510814631126389251 ) ) ;
#8273 = CARTESIAN_POINT ( 'NONE',  ( 19.81658424304261246, 9.080307684375437560, -1.500000000000002220 ) ) ;
#8274 = DIRECTION ( 'NONE',  ( 0.000000000000000000, -2.173523156925979552E-06, 0.9999999999976378895 ) ) ;
#8275 = CARTESIAN_POINT ( 'NONE',  ( -89.52287095715006160, -24.64965694238407323, 8.947790433994196491 ) ) ;
#8276 = CARTESIAN_POINT ( 'NONE',  ( -75.52287095715006160, -25.00158670708909625, 2.256160236439166411 ) ) ;
#8277 = CARTESIAN_POINT ( 'NONE',  ( -16.21501377034323710, -14.60173171477820198, -1.500000000000002220 ) ) ;
#8278 = CARTESIAN_POINT ( 'NONE',  ( -30.57287095715005165, -23.78566233802480312, -0.9545366882134203035 ) ) ;
#8279 = ORIENTED_EDGE ( 'NONE', *, *, #46869, .F. ) ;
#8280 = CARTESIAN_POINT ( 'NONE',  ( -76.62287095715007013, -24.66019654487199730, 8.947790411086128159 ) ) ;
#8281 = CARTESIAN_POINT ( 'NONE',  ( -85.62363014113577719, -25.00182538069147142, 7.747789668545045139 ) ) ;
#8282 = ORIENTED_EDGE ( 'NONE', *, *, #66637, .T. ) ;
#8283 = ORIENTED_EDGE ( 'NONE', *, *, #85738, .F. ) ;
#8284 = ORIENTED_EDGE ( 'NONE', *, *, #42237, .T. ) ;
#8285 = CARTESIAN_POINT ( 'NONE',  ( -89.40841769935764205, -25.12049752546738191, 2.832404795212221327 ) ) ;
#8286 = CARTESIAN_POINT ( 'NONE',  ( -45.52287095715007581, -23.47593901973090169, -1.443836447538997092 ) ) ;
#8287 = CARTESIAN_POINT ( 'NONE',  ( -6.347832186973104029, -20.24257907634199682, 11.49999999999998934 ) ) ;
#8288 = CARTESIAN_POINT ( 'NONE',  ( -125.6228709571500559, -23.47593901973091235, -1.443836447538995760 ) ) ;
#8289 = CARTESIAN_POINT ( 'NONE',  ( -25.92875734969025814, -3.316774720514426456, -0.08597719988137648983 ) ) ;
#8290 = CARTESIAN_POINT ( 'NONE',  ( 30.93860345374796594, -6.475225279485573360, 19.84760796525321780 ) ) ;
#8291 = CARTESIAN_POINT ( 'NONE',  ( -99.52287095715011844, -24.33832256527049154, 0.1851278514138630094 ) ) ;
#8292 = CARTESIAN_POINT ( 'NONE',  ( 4.312616920666290987, -18.91975033782923887, -1.500000000000002220 ) ) ;
#8293 = EDGE_CURVE ( 'NONE', #11381, #34120, #13762, .T. ) ;
#8294 = CARTESIAN_POINT ( 'NONE',  ( -41.88562729343752267, -25.32724636324323342, 4.398074533285874388 ) ) ;
#8295 = ORIENTED_EDGE ( 'NONE', *, *, #19850, .F. ) ;
#8296 = ADVANCED_FACE ( 'NONE', ( #81917 ), #37241, .T. ) ;
#8297 = CARTESIAN_POINT ( 'NONE',  ( -17.86923650574433609, -7.721772263035739492, 11.49999999999999645 ) ) ;
#8298 = CARTESIAN_POINT ( 'NONE',  ( -79.11611000704996854, -29.50249039766296022, 3.409318347773680369 ) ) ;
#8299 = EDGE_CURVE ( 'NONE', #58944, #69140, #8925, .T. ) ;
#8300 = DIRECTION ( 'NONE',  ( 0.000000000000000000, 0.000000000000000000, -1.000000000000000000 ) ) ;
#8301 = ORIENTED_EDGE ( 'NONE', *, *, #26743, .F. ) ;
#8302 = EDGE_CURVE ( 'NONE', #18512, #82889, #44861, .T. ) ;
#8303 = FACE_OUTER_BOUND ( 'NONE', #532, .T. ) ;
#8304 = CARTESIAN_POINT ( 'NONE',  ( -44.62287095715004881, -23.47593901973091235, -1.443836447539011525 ) ) ;
#8305 = EDGE_CURVE ( 'NONE', #20861, #47172, #40109, .T. ) ;
#8306 = CARTESIAN_POINT ( 'NONE',  ( -106.5228709571500758, -24.64898659630368627, 1.056161002820831474 ) ) ;
#8307 = CARTESIAN_POINT ( 'NONE',  ( -93.58413747110309089, -24.66019654487200441, 8.947790411086105067 ) ) ;
#8308 = CARTESIAN_POINT ( 'NONE',  ( 5.239555828037883778, -18.94419173073049478, 11.49999999999998934 ) ) ;
#8309 = LINE ( 'NONE', #39253, #65582 ) ;
#8310 = ORIENTED_EDGE ( 'NONE', *, *, #30413, .T. ) ;
#8311 = CARTESIAN_POINT ( 'NONE',  ( -7.206546067468990735, 20.34698395366585189, 11.49999999999998934 ) ) ;
#8312 = CARTESIAN_POINT ( 'NONE',  ( -40.52054906611086693, -25.00158670708910336, 2.256160236439222366 ) ) ;
#8313 = VECTOR ( 'NONE', #37757, 1000.000000000000000 ) ;
#8314 = CARTESIAN_POINT ( 'NONE',  ( -10.34999999999999254, 12.00000000000002309, 2.100000000000000089 ) ) ;
#8315 = CARTESIAN_POINT ( 'NONE',  ( -20.34888222059871410, 10.79260868881566715, -1.500000000000002220 ) ) ;
#8316 = DATE_TIME_ROLE ( 'classification_date' ) ;
#8317 = DIRECTION ( 'NONE',  ( 0.000000000000000000, 0.000000000000000000, -1.000000000000000000 ) ) ;
#8318 = CARTESIAN_POINT ( 'NONE',  ( 4.595037417369686850, -6.376774720514420736, 20.70846556543617467 ) ) ;
#8319 = CARTESIAN_POINT ( 'NONE',  ( -121.5537543563160625, -24.51419770103157347, 9.386484678747175181 ) ) ;
#8320 = CARTESIAN_POINT ( 'NONE',  ( -90.62287095715004170, -29.50247984919015209, -1.443849546365051806 ) ) ;
#8321 = CARTESIAN_POINT ( 'NONE',  ( -110.3139465455115129, -25.29823811160681046, 2.832404408888942626 ) ) ;
#8322 = CARTESIAN_POINT ( 'NONE',  ( -127.6228709571500559, -29.50248528299804818, 1.056150453629047137 ) ) ;
#8323 = CARTESIAN_POINT ( 'NONE',  ( -49.52287095715007581, -23.47593901973090169, -1.443836447538997092 ) ) ;
#8324 = CARTESIAN_POINT ( 'NONE',  ( -1.646307629438301667, 19.86461321233117872, 11.49999999999998934 ) ) ;
#8325 = CARTESIAN_POINT ( 'NONE',  ( -101.2005726979208617, -25.24249036930439871, 3.670115594759035371 ) ) ;
#8326 = CARTESIAN_POINT ( 'NONE',  ( 17.96171645398845129, 8.431260308876343146, -1.500000000000002220 ) ) ;
#8327 = CARTESIAN_POINT ( 'NONE',  ( 0.2885822020289898759, -5.876774720514416295, 19.94806476610988710 ) ) ;
#8328 = VECTOR ( 'NONE', #59359, 1000.000000000000000 ) ;
#8329 = DIRECTION ( 'NONE',  ( -0.000000000000000000, -1.000000000000000000, -0.000000000000000000 ) ) ;
#8330 = CARTESIAN_POINT ( 'NONE',  ( -94.92287095715005307, -23.47593901973090169, -1.443836447538996870 ) ) ;
#8331 = CARTESIAN_POINT ( 'NONE',  ( -13.51810693421681719, -15.76408947421354156, 11.49999999999999645 ) ) ;
#8332 = MANIFOLD_SOLID_BREP ( 'Radyus2', #12780 ) ;
#8333 = CARTESIAN_POINT ( 'NONE',  ( -7.635352852713973348, -6.376774720514415407, 20.14409848895066091 ) ) ;
#8334 = CARTESIAN_POINT ( 'NONE',  ( -106.5126059859705379, -24.51314013834316441, 0.6176544820404206160 ) ) ;
#8335 = CARTESIAN_POINT ( 'NONE',  ( -22.77908990650604792, -0.06651829912971220227, 11.49999999999999645 ) ) ;
#8336 = ORIENTED_EDGE ( 'NONE', *, *, #74542, .F. ) ;
#8337 = CARTESIAN_POINT ( 'NONE',  ( -69.58051520251109423, -24.65952944569304606, 1.056160979905704567 ) ) ;
#8338 = CARTESIAN_POINT ( 'NONE',  ( -70.01986906652584253, -25.12987166818711060, 7.062085323942192794 ) ) ;
#8339 = VERTEX_POINT ( 'NONE', #61589 ) ;
#8340 = CARTESIAN_POINT ( 'NONE',  ( 7.037473118728134303, -18.94123407977296480, -1.500000000000002220 ) ) ;
#8341 = DIRECTION ( 'NONE',  ( 0.000000000000000000, -1.000000000000000000, 0.000000000000000000 ) ) ;
#8342 = DIRECTION ( 'NONE',  ( -3.773278334453079618E-23, 0.9999999999976377785, 2.173523156925979975E-06 ) ) ;
#8343 = ORIENTED_EDGE ( 'NONE', *, *, #14807, .F. ) ;
#8344 = B_SPLINE_CURVE_WITH_KNOTS ( 'NONE', 3,
 ( #333, #70351, #55137, #78947, #9445, #63764, #2349, #8450 ),
 .UNSPECIFIED., .F., .F.,
 ( 4, 2, 2, 4 ),
 ( 0.000000000000000000, 0.002001098010032679314, 0.003001647015049018971, 0.004002196020065358628 ),
 .UNSPECIFIED. ) ;
#8345 = ORIENTED_EDGE ( 'NONE', *, *, #35271, .F. ) ;
#8346 = CARTESIAN_POINT ( 'NONE',  ( -127.5228709571500900, -23.96127896941632685, -0.6493128931037952523 ) ) ;
#8347 = CARTESIAN_POINT ( 'NONE',  ( -7.509321099650855480, 21.62252279970214985, -1.500000000000002220 ) ) ;
#8348 = CARTESIAN_POINT ( 'NONE',  ( -51.04387771620785941, -25.27420607828345567, 3.499820197422921719 ) ) ;
#8349 = CARTESIAN_POINT ( 'NONE',  ( -8.642975711230413083, 19.83371042614930957, -1.500000000000002220 ) ) ;
#8350 = DIRECTION ( 'NONE',  ( -1.000000000000000000, -3.773278334444166432E-23, -8.201307841325785021E-29 ) ) ;
#8351 = CARTESIAN_POINT ( 'NONE',  ( -5.628781154649386664, 20.11113626451368219, 11.49999999999999645 ) ) ;
#8352 = ORIENTED_EDGE ( 'NONE', *, *, #86480, .F. ) ;
#8353 = CARTESIAN_POINT ( 'NONE',  ( 282.9764569301858046, -5.965225279485572685, 20.79159422840526616 ) ) ;
#8354 = CARTESIAN_POINT ( 'NONE',  ( -124.5202242993295982, -24.34968618360934300, 0.1864209137778899961 ) ) ;
#8355 = CARTESIAN_POINT ( 'NONE',  ( -2.902263480631018577, 21.84654903556016947, 11.49999999999998934 ) ) ;
#8356 = ADVANCED_FACE ( 'NONE', ( #32495 ), #86706, .T. ) ;
#8357 = DIRECTION ( 'NONE',  ( -0.4009304992412300317, 6.845827386180410961E-16, -0.9161084732596779245 ) ) ;
#8358 = CARTESIAN_POINT ( 'NONE',  ( 8.499999999999989342, 18.74999999999999645, 2.100000000000000089 ) ) ;
#8359 = ORIENTED_EDGE ( 'NONE', *, *, #85474, .T. ) ;
#8360 = AXIS2_PLACEMENT_3D ( 'NONE', #89651, #44480, #83020 ) ;
#8361 = DIRECTION ( 'NONE',  ( 0.9161084732596777025, -7.885106708985488048E-16, -0.4009304992412306978 ) ) ;
#8362 = EDGE_CURVE ( 'NONE', #11149, #59077, #41666, .T. ) ;
#8363 = CARTESIAN_POINT ( 'NONE',  ( 14.76093561896379214, 3.316774720514426456, -27.37148769130089931 ) ) ;
#8364 = B_SPLINE_CURVE_WITH_KNOTS ( 'NONE', 3,
 ( #91194, #97808, #21666, #45041 ),
 .UNSPECIFIED., .F., .F.,
 ( 4, 4 ),
 ( 0.000000000000000000, 9.999999999998897304E-05 ),
 .UNSPECIFIED. ) ;
#8365 = VERTEX_POINT ( 'NONE', #92510 ) ;
#8366 = CARTESIAN_POINT ( 'NONE',  ( -112.5228709571500616, -29.50248528299804818, 1.056150453629043584 ) ) ;
#8367 = EDGE_LOOP ( 'NONE', ( #6618, #52808, #62295, #46064 ) ) ;
#8368 = VERTEX_POINT ( 'NONE', #52971 ) ;
#8369 = CARTESIAN_POINT ( 'NONE',  ( -71.63964193945945169, -23.96169478059713498, 10.65365249895718058 ) ) ;
#8370 = CARTESIAN_POINT ( 'NONE',  ( -83.52287095715006160, -23.47596703998600631, 11.44779298504228571 ) ) ;
#8371 = CARTESIAN_POINT ( 'NONE',  ( -4.177535645411178500, -6.376774720514415407, 20.17598923696320767 ) ) ;
#8372 = CARTESIAN_POINT ( 'NONE',  ( -16.05948562299510485, -12.68841425896798469, -1.500000000000002220 ) ) ;
#8373 = EDGE_LOOP ( 'NONE', ( #95649, #92975, #64159, #92148 ) ) ;
#8374 = CARTESIAN_POINT ( 'NONE',  ( -79.11611000704996854, -25.13069340115296058, 2.947789388436138580 ) ) ;
#8375 = DIRECTION ( 'NONE',  ( 0.000000000000000000, 1.000000000000000000, 0.000000000000000000 ) ) ;
#8376 = CARTESIAN_POINT ( 'NONE',  ( 32.98733314340959311, -0.3587747205144265483, 2.074222136288530027 ) ) ;
#8377 = CARTESIAN_POINT ( 'NONE',  ( -3.941980378682776287, 21.93750326593198352, -1.500000000000002220 ) ) ;
#8378 = CARTESIAN_POINT ( 'NONE',  ( -71.09433122556509943, -25.18619088944823758, 6.774128143594245088 ) ) ;
#8379 = DIRECTION ( 'NONE',  ( -0.000000000000000000, 0.000000000000000000, 1.000000000000000000 ) ) ;
#8380 = ORIENTED_EDGE ( 'NONE', *, *, #74911, .T. ) ;
#8381 = LINE ( 'NONE', #46449, #3073 ) ;
#8382 = CARTESIAN_POINT ( 'NONE',  ( -29.70813536620188700, -24.63645634153647990, 6.270928624350932346 ) ) ;
#8383 = CARTESIAN_POINT ( 'NONE',  ( 13.71216040526616098, 15.69570726272272232, -1.500000000000002220 ) ) ;
#8384 = CIRCLE ( 'NONE', #97472, 6.000000000000000888 ) ;
#8385 = ORIENTED_EDGE ( 'NONE', *, *, #91511, .F. ) ;
#8387 = ORIENTED_EDGE ( 'NONE', *, *, #24455, .T. ) ;
#8386 = LINE ( 'NONE', #78383, #19542 ) ;
#8388 = VERTEX_POINT ( 'NONE', #45360 ) ;
#8389 = CARTESIAN_POINT ( 'NONE',  ( -58.52287095715008292, -24.33927499327856125, 9.819080762295811837 ) ) ;
#8390 = CARTESIAN_POINT ( 'NONE',  ( -20.11743356864677423, -6.099313207006018089, -1.500000000000002220 ) ) ;
#8391 = ORIENTED_EDGE ( 'NONE', *, *, #18085, .F. ) ;
#8392 = PLANE ( 'NONE',  #44590 ) ;
#8393 = DIRECTION ( 'NONE',  ( 0.9951627101165076983, -0.09824042138329622254, -3.430045979798646929E-16 ) ) ;
#8394 = DIRECTION ( 'NONE',  ( 1.000000000000000000, 0.000000000000000000, 0.000000000000000000 ) ) ;
#8395 = DIRECTION ( 'NONE',  ( -1.000000000000000000, -3.773278334444167608E-23, -8.201307833595939069E-29 ) ) ;
#8396 = CARTESIAN_POINT ( 'NONE',  ( -36.62287095715006302, -24.65952944569303895, 1.056160979905693909 ) ) ;
#8397 = LINE ( 'NONE', #48480, #43284 ) ;
#8399 = VERTEX_POINT ( 'NONE', #63976 ) ;
#8398 = CARTESIAN_POINT ( 'NONE',  ( 2.577866586777615154, 22.04066829813923789, 11.49999999999999645 ) ) ;
#8400 = CARTESIAN_POINT ( 'NONE',  ( 2.499999999999988454, 22.00000000000000000, 2.100000000000000089 ) ) ;
#8401 = CARTESIAN_POINT ( 'NONE',  ( -23.62875734969026453, -6.143225279485574397, 23.50402280011862288 ) ) ;
#8402 = ORIENTED_EDGE ( 'NONE', *, *, #99124, .T. ) ;
#8403 = CARTESIAN_POINT ( 'NONE',  ( -22.35490716430079061, -3.811827842488555440, 11.49999999999998934 ) ) ;
#8404 = EDGE_CURVE ( 'NONE', #73995, #32487, #19725, .T. ) ;
#8406 = ORIENTED_EDGE ( 'NONE', *, *, #63432, .F. ) ;
#8405 = CARTESIAN_POINT ( 'NONE',  ( -28.54669807489977273, -24.93252285695803749, 7.282279334780318969 ) ) ;
#8407 = AXIS2_PLACEMENT_3D ( 'NONE', #20906, #21894, #52374 ) ;
#8408 = ORIENTED_EDGE ( 'NONE', *, *, #62977, .F. ) ;
#8409 = CC_DESIGN_SECURITY_CLASSIFICATION ( #21292, ( #79677 ) ) ;
#8410 = CARTESIAN_POINT ( 'NONE',  ( -70.52287095715007581, -29.50247984919015209, -1.443849546365055359 ) ) ;
#8411 = B_SPLINE_CURVE_WITH_KNOTS ( 'NONE', 3,
 ( #89270, #96882, #11635, #43600, #42613, #21240 ),
 .UNSPECIFIED., .F., .F.,
 ( 4, 2, 4 ),
 ( 1.571326169170308057E-05, 0.001397068978785498622, 0.002778424695879294117 ),
 .UNSPECIFIED. ) ;
#8412 = B_SPLINE_CURVE_WITH_KNOTS ( 'NONE', 3,
 ( #54090, #85011, #45971, #15495 ),
 .UNSPECIFIED., .F., .F.,
 ( 4, 4 ),
 ( 0.000000000000000000, 0.0001000000000000028644 ),
 .UNSPECIFIED. ) ;
#8413 = CARTESIAN_POINT ( 'NONE',  ( 20.05498121024909253, 1.910150955369836812, 11.49999999999998934 ) ) ;
#8414 = CARTESIAN_POINT ( 'NONE',  ( -101.6228709571500559, -29.50248528299804818, 1.056150453629042030 ) ) ;
#8415 = ORIENTED_EDGE ( 'NONE', *, *, #23300, .F. ) ;
#8416 = ADVANCED_FACE ( 'NONE', ( #17265 ), #86775, .T. ) ;
#8417 = CYLINDRICAL_SURFACE ( 'NONE', #79540, 1.325999999999943446 ) ;
#8418 = CARTESIAN_POINT ( 'NONE',  ( -21.99995728619510516, 3.820703864638951952, -1.500000000000002220 ) ) ;
#8419 = ORIENTED_EDGE ( 'NONE', *, *, #16444, .T. ) ;
#8420 = ORIENTED_EDGE ( 'NONE', *, *, #50567, .T. ) ;
#8421 = CARTESIAN_POINT ( 'NONE',  ( -101.2134684488937069, -25.16257435076780169, 6.841542966572015771 ) ) ;
#8422 = FACE_OUTER_BOUND ( 'NONE', #93995, .T. ) ;
#8423 = ADVANCED_FACE ( 'NONE', ( #79160, #25377 ), #87274, .F. ) ;
#8424 = FACE_BOUND ( 'NONE', #8631, .T. ) ;
#8425 = DIRECTION ( 'NONE',  ( -0.000000000000000000, 1.000000000000000000, -0.000000000000000000 ) ) ;
#8426 = ADVANCED_FACE ( 'NONE', ( #18270 ), #91902, .T. ) ;
#8427 = CARTESIAN_POINT ( 'NONE',  ( -95.52287095715006160, -24.99132157543166954, 2.256160258750667502 ) ) ;
#8428 = CARTESIAN_POINT ( 'NONE',  ( -10.41718274906430786, -16.55731393670301088, -1.500000000000002220 ) ) ;
#8429 = ADVANCED_FACE ( 'NONE', ( #34993 ), #43112, .T. ) ;
#8430 = CARTESIAN_POINT ( 'NONE',  ( -5.293508136514246232, -5.876774720514409189, 19.18727597066021318 ) ) ;
#8431 = CARTESIAN_POINT ( 'NONE',  ( 18.54456287915894563, -10.88813254144886322, 11.49999999999998934 ) ) ;
#8432 = CARTESIAN_POINT ( 'NONE',  ( -128.6235872204422321, -24.51314013834317862, 0.6176544820404316072 ) ) ;
#8433 = EDGE_CURVE ( 'NONE', #83907, #62489, #97358, .T. ) ;
#8434 = LINE ( 'NONE', #820, #67528 ) ;
#8435 = CARTESIAN_POINT ( 'NONE',  ( 8.349999999999972999, 27.69999999999999574, 2.100000000000000089 ) ) ;
#8436 = DIRECTION ( 'NONE',  ( 0.000000000000000000, -1.000000000000000000, 0.000000000000000000 ) ) ;
#8437 = CARTESIAN_POINT ( 'NONE',  ( 4.459850365305920938, 22.40387240153798487, -1.500000000000002220 ) ) ;
#8438 = AXIS2_PLACEMENT_3D ( 'NONE', #69817, #69315, #24133 ) ;
#8439 = PERSON_AND_ORGANIZATION_ROLE ( 'classification_officer' ) ;
#8440 = CARTESIAN_POINT ( 'NONE',  ( -120.5228709571500616, -25.00158670708909625, 2.256160236439166411 ) ) ;
#8441 = CARTESIAN_POINT ( 'NONE',  ( -70.35895856474229504, -25.31161946917133321, 5.313173610579343453 ) ) ;
#8442 = CARTESIAN_POINT ( 'NONE',  ( -1.415466703587968667, 19.98303252902060834, 11.49999999999999645 ) ) ;
#8443 = CARTESIAN_POINT ( 'NONE',  ( -99.92287095715006728, -23.47593901973090169, -1.443836447538996870 ) ) ;
#8444 = DIRECTION ( 'NONE',  ( 0.000000000000000000, 0.000000000000000000, -1.000000000000000000 ) ) ;
#8445 = DIRECTION ( 'NONE',  ( -0.6599726524652352877, 0.000000000000000000, 0.7512896232465892110 ) ) ;
#8446 = LINE ( 'NONE', #46510, #66728 ) ;
#8447 = B_SPLINE_CURVE_WITH_KNOTS ( 'NONE', 3,
 ( #73701, #4196, #97531, #81314, #28029, #74205, #4695, #11796, #49384, #58988, #66120, #19407, #42284, #56995, #73214, #89428, #50376, #42770, #43755, #20392, #34649, #51367 ),
 .UNSPECIFIED., .F., .F.,
 ( 4, 2, 2, 2, 2, 2, 2, 2, 2, 2, 4 ),
 ( 0.000000000000000000, 0.0002789761287897273164, 0.0005579522575794546328, 0.0008369283863691820034, 0.001115904515158909266, 0.001673856772738364874, 0.002231809030317820700, 0.002789761287897275874, 0.003347713545476731917, 0.003905665803056187092, 0.004463618060635643134 ),
 .UNSPECIFIED. ) ;
#8448 = ORIENTED_EDGE ( 'NONE', *, *, #59899, .F. ) ;
#8449 = ADVANCED_FACE ( 'NONE', ( #48739 ), #72564, .F. ) ;
#8450 = CARTESIAN_POINT ( 'NONE',  ( -85.62287095715004170, -24.99132157543083821, 2.256160258750667502 ) ) ;
#8451 = CARTESIAN_POINT ( 'NONE',  ( 18.41774212405765709, -11.57998961627671441, -1.500000000000002220 ) ) ;
#8452 = SPHERICAL_SURFACE ( 'NONE', #56099, 1.000000000000000000 ) ;
#8453 = CARTESIAN_POINT ( 'NONE',  ( -17.62575346185542102, 8.740161020289619387, -1.500000000000002220 ) ) ;
#8454 = DIRECTION ( 'NONE',  ( 0.000000000000000000, 0.9999999999976377785, 2.173523156925979128E-06 ) ) ;
#8455 = FACE_OUTER_BOUND ( 'NONE', #79387, .T. ) ;
#8456 = DATE_TIME_ROLE ( 'classification_date' ) ;
#8457 = VECTOR ( 'NONE', #330, 1000.000000000000000 ) ;
#8458 = LINE ( 'NONE', #92185, #72668 ) ;
#8459 = DIRECTION ( 'NONE',  ( -0.000000000000000000, -1.000000000000000000, 0.000000000000000000 ) ) ;
#8460 = CARTESIAN_POINT ( 'NONE',  ( 4.814550503181614260, -19.98661186389175271, 11.49999999999999645 ) ) ;
#8461 = CARTESIAN_POINT ( 'NONE',  ( 22.81105451610979173, -6.475225279485573360, -20.71691820600746681 ) ) ;
#8462 = CIRCLE ( 'NONE', #71627, 1.325999999999990298 ) ;
#8463 = DIRECTION ( 'NONE',  ( 0.09721092304694051167, 0.000000000000000000, -0.9952638024365005887 ) ) ;
#8464 = CARTESIAN_POINT ( 'NONE',  ( -12.77507031947300042, 18.62636059118606724, 11.49999999999999645 ) ) ;
#8465 = ORIENTED_EDGE ( 'NONE', *, *, #73953, .F. ) ;
#8466 = CARTESIAN_POINT ( 'NONE',  ( -99.55666892486131303, -25.26387334811825269, 4.188639845853757926 ) ) ;
#8467 = CARTESIAN_POINT ( 'NONE',  ( -60.55620429048340014, -24.99132157543166599, 2.256160258750668390 ) ) ;
#8468 = DIRECTION ( 'NONE',  ( 0.000000000000000000, 0.000000000000000000, -1.000000000000000000 ) ) ;
#8469 = CARTESIAN_POINT ( 'NONE',  ( -85.62287095715007013, -25.00158670708909270, 2.256160236439165967 ) ) ;
#8470 = CARTESIAN_POINT ( 'NONE',  ( -26.25023971703978276, -24.61459967487257217, 7.578547068710756562 ) ) ;
#8471 = LINE ( 'NONE', #53160, #82042 ) ;
#8472 = EDGE_CURVE ( 'NONE', #59266, #77504, #5338, .T. ) ;
#8473 = EDGE_LOOP ( 'NONE', ( #59285, #51682, #15693, #51065 ) ) ;
#8474 = AXIS2_PLACEMENT_3D ( 'NONE', #55, #15269, #79174 ) ;
#8475 = CARTESIAN_POINT ( 'NONE',  ( 20.16173082093541424, 11.17373015621797627, 11.49999999999999645 ) ) ;
#8476 = CARTESIAN_POINT ( 'NONE',  ( 9.312063170398973355, -20.82641193498425025, -1.500000000000002220 ) ) ;
#8477 = CARTESIAN_POINT ( 'NONE',  ( -33.62287095715005592, -23.47596703998600276, 11.44779298504227505 ) ) ;
#8478 = CARTESIAN_POINT ( 'NONE',  ( -105.6228709571500275, -23.84047902841604127, -0.8780736468305382347 ) ) ;
#8479 = DIRECTION ( 'NONE',  ( -0.000000000000000000, -1.000000000000000000, -0.000000000000000000 ) ) ;
#8480 = CC_DESIGN_SECURITY_CLASSIFICATION ( #97564, ( #11661 ) ) ;
#8481 = CARTESIAN_POINT ( 'NONE',  ( 22.29217321540274099, 2.676729263222305644, 11.49999999999999645 ) ) ;
#8482 = VERTEX_POINT ( 'NONE', #74058 ) ;
#8483 = CARTESIAN_POINT ( 'NONE',  ( -84.52287095715006160, -23.47593901973090524, -1.443836447538996648 ) ) ;
#8484 = CARTESIAN_POINT ( 'NONE',  ( -38.62287095715005592, -24.64965695001467694, 8.947790433994187609 ) ) ;
#8485 = CARTESIAN_POINT ( 'NONE',  ( -9.563806973793814947, 19.74097577964120376, 11.49999999999998934 ) ) ;
#8486 = EDGE_CURVE ( 'NONE', #87540, #93259, #42436, .T. ) ;
#8487 = CARTESIAN_POINT ( 'NONE',  ( -5.023036858974360364, -6.376774720514410077, 19.14743589743590491 ) ) ;
#8488 = CARTESIAN_POINT ( 'NONE',  ( -71.52287095715007581, -23.48786465467241058, 11.44779295918254647 ) ) ;
#8489 = CARTESIAN_POINT ( 'NONE',  ( -126.6228709571500559, -23.47593901973091235, -1.443836447538995760 ) ) ;
#8490 = ORIENTED_EDGE ( 'NONE', *, *, #34263, .F. ) ;
#8491 = CARTESIAN_POINT ( 'NONE',  ( -78.54639593351097915, -24.34968618360933945, 0.1864209137778830849 ) ) ;
#8492 = CARTESIAN_POINT ( 'NONE',  ( 6.150000000000003908, 1.999999999999998224, 18.24068255301868291 ) ) ;
#8493 = ORIENTED_EDGE ( 'NONE', *, *, #93110, .T. ) ;
#8494 = CARTESIAN_POINT ( 'NONE',  ( -20.44062828730913139, -1.133067592104922694, -1.500000000000002220 ) ) ;
#8495 = VERTEX_POINT ( 'NONE', #19748 ) ;
#8496 = ORIENTED_EDGE ( 'NONE', *, *, #66338, .T. ) ;
#8498 = ORIENTED_EDGE ( 'NONE', *, *, #66219, .F. ) ;
#8497 = AXIS2_PLACEMENT_3D ( 'NONE', #24104, #2792, #48962 ) ;
#8499 = VERTEX_POINT ( 'NONE', #34000 ) ;
#8500 = CARTESIAN_POINT ( 'NONE',  ( -17.29220519630379016, 15.29500218549028645, 11.49999999999998934 ) ) ;
#8501 = CARTESIAN_POINT ( 'NONE',  ( -40.79740563987936497, -25.26871255744267231, 3.880430150159563496 ) ) ;
#8502 = CARTESIAN_POINT ( 'NONE',  ( 16.58868386459195676, 11.68684615565071283, -1.500000000000002220 ) ) ;
#8503 = ORIENTED_EDGE ( 'NONE', *, *, #15491, .T. ) ;
#8504 = CARTESIAN_POINT ( 'NONE',  ( 14.52511747680497933, -5.965225279485572685, -27.86035006098926559 ) ) ;
#8505 = CARTESIAN_POINT ( 'NONE',  ( -92.54897924172895785, -24.34968618360935011, 0.1864209137778966296 ) ) ;
#8506 = PLANE ( 'NONE',  #33531 ) ;
#8507 = CARTESIAN_POINT ( 'NONE',  ( 4.486687842132109694, -6.376774720514410077, 18.98221446873611029 ) ) ;
#8509 = EDGE_LOOP ( 'NONE', ( #20117, #33294, #68422, #52588 ) ) ;
#8508 = CARTESIAN_POINT ( 'NONE',  ( -13.16228656746626591, 16.97819584282690286, 11.49999999999999645 ) ) ;
#8510 = CARTESIAN_POINT ( 'NONE',  ( -75.65600191686841924, -23.48783264082477018, -1.443836473390089914 ) ) ;
#8511 = CARTESIAN_POINT ( 'NONE',  ( -61.59803781195726913, -23.96169478059713143, 10.65365249895718591 ) ) ;
#8512 = ORIENTED_EDGE ( 'NONE', *, *, #98582, .T. ) ;
#8513 = CARTESIAN_POINT ( 'NONE',  ( -18.06733440434376092, 10.15830956056102963, 11.49999999999998934 ) ) ;
#8514 = ORIENTED_EDGE ( 'NONE', *, *, #33342, .F. ) ;
#8515 = CC_DESIGN_DATE_AND_TIME_ASSIGNMENT ( #55631, #68843, ( #21292 ) ) ;
#8517 = ORIENTED_EDGE ( 'NONE', *, *, #40410, .F. ) ;
#8516 = CARTESIAN_POINT ( 'NONE',  ( 29.73860345376319003, -1.477225279485574028, 19.84760796525321780 ) ) ;
#8518 = CIRCLE ( 'NONE', #94411, 6.119803529381341534 ) ;
#8519 = CARTESIAN_POINT ( 'NONE',  ( -41.49211046241916989, -24.35071581493542681, 9.817618358456032368 ) ) ;
#8520 = DIRECTION ( 'NONE',  ( -3.773278334453079030E-23, 0.9999999999976377785, 2.173523156925979128E-06 ) ) ;
#8521 = ORIENTED_EDGE ( 'NONE', *, *, #43858, .F. ) ;
#8522 = ORIENTED_EDGE ( 'NONE', *, *, #19539, .F. ) ;
#8523 = CARTESIAN_POINT ( 'NONE',  ( -40.52287095715007581, -24.15431212366391023, -0.2830839119429403028 ) ) ;
#8524 = CARTESIAN_POINT ( 'NONE',  ( -77.62287095715004170, -23.72773821059535848, 11.05748984161097503 ) ) ;
#8525 = CARTESIAN_POINT ( 'NONE',  ( -64.62287095715005592, -29.50248528299804818, 1.056150453629034924 ) ) ;
#8526 = CARTESIAN_POINT ( 'NONE',  ( -21.99024891984110752, 1.279939690139831665, 11.49999999999999645 ) ) ;
#8527 = FACE_OUTER_BOUND ( 'NONE', #11812, .T. ) ;
#8528 = CARTESIAN_POINT ( 'NONE',  ( -8.190886813464794969, 21.05079722441571732, 11.49999999999998934 ) ) ;
#8529 = CARTESIAN_POINT ( 'NONE',  ( 2.184583272949580213, -20.89682302726931340, -1.500000000000002220 ) ) ;
#8530 = LINE ( 'NONE', #69926, #7068 ) ;
#8532 = ORIENTED_EDGE ( 'NONE', *, *, #61268, .T. ) ;
#8531 = CARTESIAN_POINT ( 'NONE',  ( -46.66198039096105532, -23.48786465467240703, 11.44779295918255180 ) ) ;
#8533 = B_SPLINE_CURVE_WITH_KNOTS ( 'NONE', 3,
 ( #75433, #98773, #68343, #20156 ),
 .UNSPECIFIED., .F., .F.,
 ( 4, 4 ),
 ( 0.000000000000000000, 0.0001000000000000028644 ),
 .UNSPECIFIED. ) ;
#8534 = VECTOR ( 'NONE', #32149, 1000.000000000000114 ) ;
#8535 = ORIENTED_EDGE ( 'NONE', *, *, #14481, .T. ) ;
#8536 = CARTESIAN_POINT ( 'NONE',  ( -88.52287095715006160, -24.64965694238407323, 8.947790433994196491 ) ) ;
#8537 = LINE ( 'NONE', #16639, #49016 ) ;
#8538 = ORIENTED_EDGE ( 'NONE', *, *, #43491, .F. ) ;
#8539 = CARTESIAN_POINT ( 'NONE',  ( 10.59196434753715010, 18.29633683537252509, 11.49999999999998934 ) ) ;
#8540 = DIRECTION ( 'NONE',  ( -3.445208383210904213E-15, 0.9940716917543755970, -0.1087265912856350408 ) ) ;
#8541 = CARTESIAN_POINT ( 'NONE',  ( -50.46940435010577630, -25.03148741713950187, 7.561692462087905575 ) ) ;
#8542 = CARTESIAN_POINT ( 'NONE',  ( -88.62287095715004170, -24.64965695001469115, 8.947790433994180503 ) ) ;
#8543 = PLANE ( 'NONE',  #71882 ) ;
#8544 = PLANE ( 'NONE',  #82715 ) ;
#8545 = CARTESIAN_POINT ( 'NONE',  ( -22.11311035156252558, 1.696007508605793301, -1.500000000000002220 ) ) ;
#8546 = DIRECTION ( 'NONE',  ( 2.501730345825856573E-15, 0.000000000000000000, 1.000000000000000000 ) ) ;
#8547 = EDGE_CURVE ( 'NONE', #46190, #41589, #56228, .T. ) ;
#8548 = ORIENTED_EDGE ( 'NONE', *, *, #23556, .T. ) ;
#8549 = CARTESIAN_POINT ( 'NONE',  ( -82.58953762381671027, -23.47596703998600276, 11.44779298504227683 ) ) ;
#8550 = CARTESIAN_POINT ( 'NONE',  ( -37.64896086412395704, -23.96119346886880663, -0.6495511937831990323 ) ) ;
#8551 = CARTESIAN_POINT ( 'NONE',  ( -40.33334756173746172, -25.30373406279863957, 5.539412886275527192 ) ) ;
#8553 = B_SPLINE_CURVE_WITH_KNOTS ( 'NONE', 3,
 ( #67553, #90872, #74644, #13238, #98471, #52818, #29463, #6633, #45704, #51826, #38081, #58935, #76630, #27981 ),
 .UNSPECIFIED., .F., .F.,
 ( 4, 2, 2, 2, 2, 2, 4 ),
 ( 8.673617379884035472E-19, 0.0001871047122523776312, 0.0003742094245047543951, 0.0007484188490095090070, 0.001122628273514263836, 0.001309732985766650900, 0.001496837698019038180 ),
 .UNSPECIFIED. ) ;
#8552 = CARTESIAN_POINT ( 'NONE',  ( -100.5847598729784380, -24.92564183028979130, 1.928384488918251760 ) ) ;
#8554 = DIRECTION ( 'NONE',  ( 1.000000000000000000, 3.773278334444167608E-23, 8.201307833595939069E-29 ) ) ;
#8555 = VECTOR ( 'NONE', #29401, 1000.000000000000114 ) ;
#8556 = CARTESIAN_POINT ( 'NONE',  ( -0.2416374764669896869, -19.45557994585427508, 11.49999999999998934 ) ) ;
#8557 = CC_DESIGN_APPROVAL ( #22686, ( #19830 ) ) ;
#8558 = EDGE_CURVE ( 'NONE', #53441, #90740, #6594, .T. ) ;
#8559 = CARTESIAN_POINT ( 'NONE',  ( -21.12015818079280649, -3.594773940630530795, 11.49999999999998934 ) ) ;
#8560 = CARTESIAN_POINT ( 'NONE',  ( -64.55620429048339304, -24.65952944569304606, 1.056160979905695685 ) ) ;
#8561 = CARTESIAN_POINT ( 'NONE',  ( -60.58056880734444860, -24.83644354574317603, 8.397322867105112110 ) ) ;
#8562 = EDGE_CURVE ( 'NONE', #74181, #48376, #99102, .T. ) ;
#8563 = CARTESIAN_POINT ( 'NONE',  ( -51.54141383909072971, -24.34968618360933590, 0.1864209137778788938 ) ) ;
#8564 = CARTESIAN_POINT ( 'NONE',  ( -44.52287095715006160, -24.64965694238575011, 8.947790433994205372 ) ) ;
#8565 = CARTESIAN_POINT ( 'NONE',  ( -1.179572987637725889, 22.66035800735570049, -1.500000000000002220 ) ) ;
#8566 = VECTOR ( 'NONE', #60261, 1000.000000000000114 ) ;
#8567 = PLANE ( 'NONE',  #85462 ) ;
#8568 = CARTESIAN_POINT ( 'NONE',  ( 11.98973536156539943, 2.682774720514426559, -26.26140391504922178 ) ) ;
#8569 = CARTESIAN_POINT ( 'NONE',  ( 17.96171645398845129, 8.431260308876343146, 11.49999999999999645 ) ) ;
#8570 = CARTESIAN_POINT ( 'NONE',  ( 6.156881756163101294, -6.376774720514413630, 19.74809127057764968 ) ) ;
#8571 = CIRCLE ( 'NONE', #2134, 2.500000000000000444 ) ;
#8572 = CARTESIAN_POINT ( 'NONE',  ( -73.62287095715008434, -24.33832256526968862, 0.1851278514119885088 ) ) ;
#8573 = LINE ( 'NONE', #10068, #35848 ) ;
#8574 = ORIENTED_EDGE ( 'NONE', *, *, #20459, .T. ) ;
#8575 = ADVANCED_FACE ( 'NONE', ( #88793 ), #4050, .T. ) ;
#8576 = DIRECTION ( 'NONE',  ( -1.000000000000000000, -3.773278334444167608E-23, -8.201307833595939069E-29 ) ) ;
#8577 = CARTESIAN_POINT ( 'NONE',  ( -5.926585084595196840, -5.876774720514415407, 20.19722303762275573 ) ) ;
#8578 = CARTESIAN_POINT ( 'NONE',  ( -51.32120688873476411, -25.27412302063908101, 3.174475563666860012 ) ) ;
#8579 = CARTESIAN_POINT ( 'NONE',  ( -20.21959982808627032, -7.803091810188320210, 11.49999999999998934 ) ) ;
#8580 = CARTESIAN_POINT ( 'NONE',  ( -32.58953762381672448, -24.66019654487198665, 8.947790411086138818 ) ) ;
#8581 = CARTESIAN_POINT ( 'NONE',  ( -10.96721834449554933, 16.09610527815933168, -1.500000000000002220 ) ) ;
#8582 = CARTESIAN_POINT ( 'NONE',  ( -61.62287095715008434, -23.95044443724992433, 10.65354141964650125 ) ) ;
#8583 = VERTEX_POINT ( 'NONE', #75036 ) ;
#8584 = CARTESIAN_POINT ( 'NONE',  ( 19.80222353126469415, -4.898785079568316547, 11.49999999999999645 ) ) ;
#8585 = CARTESIAN_POINT ( 'NONE',  ( -80.58515248380662399, -24.73486907724918282, 1.287355809206963908 ) ) ;
#8587 = AXIS2_PLACEMENT_3D ( 'NONE', #26661, #41901, #10426 ) ;
#8586 = CARTESIAN_POINT ( 'NONE',  ( -69.62287095715005592, -29.50250243563736774, 8.947779886222143375 ) ) ;
#8588 = ORIENTED_EDGE ( 'NONE', *, *, #34312, .F. ) ;
#8589 = CARTESIAN_POINT ( 'NONE',  ( -79.23479724101613897, -25.14774951949591042, 6.961175731640159015 ) ) ;
#8590 = CARTESIAN_POINT ( 'NONE',  ( -29.62287095715004881, -24.58390616985635546, 1.056161279468100123 ) ) ;
#8591 = DIRECTION ( 'NONE',  ( -3.773278334453079030E-23, 0.9999999999976377785, 2.173523156925979128E-06 ) ) ;
#8592 = CARTESIAN_POINT ( 'NONE',  ( -40.62957167911499567, -24.83644354573577928, 8.397322867130096569 ) ) ;
#8593 = CARTESIAN_POINT ( 'NONE',  ( -1.012926118674504883, -6.376774720514415407, 19.92818918856637822 ) ) ;
#8594 = CARTESIAN_POINT ( 'NONE',  ( -3.374260732160392795, -19.82512954709321562, -1.500000000000002220 ) ) ;
#8595 = EDGE_CURVE ( 'NONE', #52090, #88744, #59838, .T. ) ;
#8596 = DIRECTION ( 'NONE',  ( -0.3133898629642186684, 0.000000000000000000, 0.9496245541219267006 ) ) ;
#8597 = AXIS2_PLACEMENT_3D ( 'NONE', #47214, #16747, #20244 ) ;
#8598 = ORIENTED_EDGE ( 'NONE', *, *, #56365, .T. ) ;
#8599 = CARTESIAN_POINT ( 'NONE',  ( -95.62287095715005592, -24.99156045073393173, 7.747789690856161648 ) ) ;
#8600 = ADVANCED_FACE ( 'NONE', ( #83653 ), #20251, .F. ) ;
#8601 = CARTESIAN_POINT ( 'NONE',  ( 2.319610639010541764, -22.79860127089448696, 11.49999999999999645 ) ) ;
#8602 = B_SPLINE_CURVE_WITH_KNOTS ( 'NONE', 3,
 ( #41017, #10552, #41511, #95789, #62682, #30208 ),
 .UNSPECIFIED., .F., .F.,
 ( 4, 2, 4 ),
 ( 0.000000000000000000, 0.001380764517854762364, 0.002761529035709524727 ),
 .UNSPECIFIED. ) ;
#8603 = CARTESIAN_POINT ( 'NONE',  ( -22.07869367785253090, -5.390224856484156390, -1.500000000000002220 ) ) ;
#8604 = VERTEX_POINT ( 'NONE', #20749 ) ;
#8605 = CARTESIAN_POINT ( 'NONE',  ( -71.70487185728066493, -25.24836947220651595, 6.282845680122700394 ) ) ;
#8606 = VECTOR ( 'NONE', #69359, 1000.000000000000114 ) ;
#8607 = LINE ( 'NONE', #93835, #65609 ) ;
#8608 = CARTESIAN_POINT ( 'NONE',  ( -39.44867388513146977, -25.28405637431412956, 4.124821700262499391 ) ) ;
#8609 = CARTESIAN_POINT ( 'NONE',  ( -30.57287095715005876, -24.68108607773119090, 1.119903471769779335 ) ) ;
#8610 = CARTESIAN_POINT ( 'NONE',  ( -128.5561025708502143, -23.73791477778912551, 11.05961554403169522 ) ) ;
#8611 = EDGE_CURVE ( 'NONE', #22611, #149, #63406, .T. ) ;
#8612 = CARTESIAN_POINT ( 'NONE',  ( -40.52287095715006870, -23.47593901973090169, -1.443836447538997092 ) ) ;
#8613 = ORIENTED_EDGE ( 'NONE', *, *, #16315, .T. ) ;
#8614 = CARTESIAN_POINT ( 'NONE',  ( -2.125485521908593078, 20.27274140177646444, 11.49999999999998934 ) ) ;
#8615 = ORIENTED_EDGE ( 'NONE', *, *, #39342, .T. ) ;
#8616 = CARTESIAN_POINT ( 'NONE',  ( 18.09022303007301247, 14.20294132079179938, 11.49999999999998934 ) ) ;
#8617 = CARTESIAN_POINT ( 'NONE',  ( -1.390986686320385468, -5.876774720514412742, 19.62288733224860948 ) ) ;
#8618 = DIRECTION ( 'NONE',  ( -2.860369681942282691E-39, -2.173523156925979128E-06, 0.9999999999976378895 ) ) ;
#8619 = EDGE_LOOP ( 'NONE', ( #60818, #37687, #21358, #81138 ) ) ;
#8620 = DIRECTION ( 'NONE',  ( 1.000000000000000000, 3.773278334444166432E-23, 8.201307841325785021E-29 ) ) ;
#8621 = AXIS2_PLACEMENT_3D ( 'NONE', #85825, #86822, #62495 ) ;
#8622 = CARTESIAN_POINT ( 'NONE',  ( -118.7289294252545488, -25.23516544469813283, 6.311314093648517698 ) ) ;
#8624 = ORIENTED_EDGE ( 'NONE', *, *, #33867, .F. ) ;
#8623 = CARTESIAN_POINT ( 'NONE',  ( 20.65877813657638740, 5.380652674160894655, 11.49999999999999645 ) ) ;
#8625 = CC_DESIGN_APPROVAL ( #36350, ( #96129 ) ) ;
#8626 = ORIENTED_EDGE ( 'NONE', *, *, #88602, .T. ) ;
#8627 = CARTESIAN_POINT ( 'NONE',  ( -5.994446910899359438, -21.39327697068355505, -1.500000000000002220 ) ) ;
#8628 = CARTESIAN_POINT ( 'NONE',  ( 19.46067915675286386, 6.892634557253153105, -1.500000000000002220 ) ) ;
#8629 = ADVANCED_FACE ( 'NONE', ( #6540 ), #30368, .F. ) ;
#8631 = EDGE_LOOP ( 'NONE', ( #4269, #72139 ) ) ;
#8630 = CIRCLE ( 'NONE', #44270, 1.149999999999999911 ) ;
#8632 = DIRECTION ( 'NONE',  ( -3.773278334444166432E-23, 1.000000000000000000, 0.000000000000000000 ) ) ;
#8633 = CARTESIAN_POINT ( 'NONE',  ( -95.54869878359860991, -24.52399227489127398, 9.353111116836524630 ) ) ;
#8634 = ORIENTED_EDGE ( 'NONE', *, *, #60014, .F. ) ;
#8635 = DIRECTION ( 'NONE',  ( 0.000000000000000000, 0.000000000000000000, -1.000000000000000000 ) ) ;
#8636 = EDGE_CURVE ( 'NONE', #81022, #17829, #75531, .T. ) ;
#8637 = ORIENTED_EDGE ( 'NONE', *, *, #35762, .F. ) ;
#8638 = VECTOR ( 'NONE', #99622, 1000.000000000000114 ) ;
#8639 = DIRECTION ( 'NONE',  ( -0.000000000000000000, 0.000000000000000000, 1.000000000000000000 ) ) ;
#8640 = CARTESIAN_POINT ( 'NONE',  ( -116.2228709571500644, -23.47596703998600631, 11.44779298504227860 ) ) ;
#8641 = CARTESIAN_POINT ( 'NONE',  ( -19.94048968823238255, 6.179419890754223488, -1.500000000000002220 ) ) ;
#8642 = CARTESIAN_POINT ( 'NONE',  ( 16.32745387341675780, -14.53119815553504068, 11.49999999999999645 ) ) ;
#8643 = CARTESIAN_POINT ( 'NONE',  ( -27.27372260060660736, -24.89279990012216359, 7.541612528384861847 ) ) ;
#8644 = CARTESIAN_POINT ( 'NONE',  ( -98.97737064162744502, -25.20109320840395739, 6.595599656366546881 ) ) ;
#8645 = CARTESIAN_POINT ( 'NONE',  ( 6.846561153812083411, -21.39451737393737574, 11.49999999999998934 ) ) ;
#8646 = EDGE_CURVE ( 'NONE', #71422, #52694, #15031, .T. ) ;
#8647 = EDGE_CURVE ( 'NONE', #52813, #12728, #23457, .T. ) ;
#8648 = CARTESIAN_POINT ( 'NONE',  ( -50.41800648699645393, -25.26334751556140290, 4.735576037500227820 ) ) ;
#8649 = CARTESIAN_POINT ( 'NONE',  ( -50.52287095715006160, -23.48786465467241058, 11.44779295918255002 ) ) ;
#8650 = CARTESIAN_POINT ( 'NONE',  ( 4.189750619059152470, -5.876774720514427841, 21.76591699724029283 ) ) ;
#8651 = B_SPLINE_SURFACE_WITH_KNOTS ( 'NONE', 3, 3, ( 
 ( #73474, #19172, #57760, #27299 ),
 ( #89200, #72985, #2468, #43029 ),
 ( #80083, #35420, #73972, #96309 ),
 ( #71986, #34412, #41033, #80580 ),
 ( #81085, #33402, #64394, #4470 ),
 ( #11561, #50634, #18674, #25797 ),
 ( #42539, #66379, #64894, #95309 ) ),
 .UNSPECIFIED., .F., .F., .F.,
 ( 4, 3, 4 ),
 ( 4, 4 ),
 ( 0.2590395444657082047, 0.4996700994841927201, 0.7403006545026772356 ),
 ( 0.9757605720749513711, 0.9935688618463752730 ),
 .UNSPECIFIED. ) ;
#8652 = B_SPLINE_CURVE_WITH_KNOTS ( 'NONE', 3,
 ( #36503, #4070, #50746, #89800 ),
 .UNSPECIFIED., .F., .F.,
 ( 4, 4 ),
 ( 2.775557561562891351E-17, 0.0001000000000000028644 ),
 .UNSPECIFIED. ) ;
#8653 = EDGE_LOOP ( 'NONE', ( #1874, #64471, #30139, #33485 ) ) ;
#8654 = VERTEX_POINT ( 'NONE', #83151 ) ;
#8655 = EDGE_LOOP ( 'NONE', ( #80781, #60055, #52556, #65517 ) ) ;
#8656 = CARTESIAN_POINT ( 'NONE',  ( -17.20161093224466953, -12.68000408521323408, -1.500000000000002220 ) ) ;
#8657 = CARTESIAN_POINT ( 'NONE',  ( 12.67250375155129127, 18.46511205475877304, 11.49999999999999645 ) ) ;
#8658 = ORIENTED_EDGE ( 'NONE', *, *, #48663, .T. ) ;
#8659 = CARTESIAN_POINT ( 'NONE',  ( -21.07084664159375009, 0.3847054351051909515, 11.49999999999998934 ) ) ;
#8660 = CARTESIAN_POINT ( 'NONE',  ( -67.62287095715005592, -29.50250243563736774, 8.947779886222143375 ) ) ;
#8661 = CARTESIAN_POINT ( 'NONE',  ( -16.62890364678930410, -10.96057169749504645, -1.500000000000002220 ) ) ;
#8662 = CARTESIAN_POINT ( 'NONE',  ( -50.52684220265726367, -24.92592662359561473, 8.075495903018000021 ) ) ;
#8663 = CARTESIAN_POINT ( 'NONE',  ( -49.25197268407241324, -25.13168855254613021, 7.110315888415422947 ) ) ;
#8664 = CARTESIAN_POINT ( 'NONE',  ( -13.73438224071023761, 17.16576579689093762, -1.500000000000002220 ) ) ;
#8665 = CARTESIAN_POINT ( 'NONE',  ( -84.52287095715006160, -24.64965694238406613, 8.947790433994198267 ) ) ;
#8666 = ORIENTED_EDGE ( 'NONE', *, *, #35312, .F. ) ;
#8667 = CARTESIAN_POINT ( 'NONE',  ( -74.55620429048335041, -24.64965694238574301, 8.947790433994201820 ) ) ;
#8668 = EDGE_CURVE ( 'NONE', #26207, #98742, #68438, .T. ) ;
#8669 = VECTOR ( 'NONE', #52970, 1000.000000000000000 ) ;
#8670 = CARTESIAN_POINT ( 'NONE',  ( -81.62287095715005592, -29.50248528299804818, 1.056150453629038477 ) ) ;
#8671 = CARTESIAN_POINT ( 'NONE',  ( 13.71216040526616098, 15.69570726272272232, 11.49999999999999645 ) ) ;
#8672 = CARTESIAN_POINT ( 'NONE',  ( 31.68607835968417064, -4.403148666511627951, 29.28367637967570758 ) ) ;
#8673 = VECTOR ( 'NONE', #76047, 1000.000000000000000 ) ;
#8674 = FACE_OUTER_BOUND ( 'NONE', #21224, .T. ) ;
#8675 = CARTESIAN_POINT ( 'NONE',  ( -117.5228709571500758, -24.65952944569305316, 1.056160979905705899 ) ) ;
#8676 = CARTESIAN_POINT ( 'NONE',  ( -1.376967878889499897, 21.29249089469206524, -1.500000000000002220 ) ) ;
#8677 = DIRECTION ( 'NONE',  ( -0.000000000000000000, 1.000000000000000000, -0.000000000000000000 ) ) ;
#8678 = CARTESIAN_POINT ( 'NONE',  ( -48.62287095715004881, -29.50250786944525672, 11.44777988621624054 ) ) ;
#8679 = ADVANCED_FACE ( 'NONE', ( #44107 ), #6034, .F. ) ;
#8680 = CARTESIAN_POINT ( 'NONE',  ( -64.49195876600683164, -24.66019654487199730, 8.947790411086113949 ) ) ;
#8681 = CARTESIAN_POINT ( 'NONE',  ( -69.99588697226764111, -25.12112739299269037, 7.112216829152949948 ) ) ;
#8682 = CARTESIAN_POINT ( 'NONE',  ( -6.869692127560369066, -21.44495933931894527, -1.500000000000002220 ) ) ;
#8683 = EDGE_CURVE ( 'NONE', #80402, #73900, #61061, .T. ) ;
#8684 = DIRECTION ( 'NONE',  ( -0.000000000000000000, -0.000000000000000000, -1.000000000000000000 ) ) ;
#8685 = EDGE_LOOP ( 'NONE', ( #92222, #23945, #57445, #56071 ) ) ;
#8687 = CARTESIAN_POINT ( 'NONE',  ( -99.22287095715007865, -23.47593901973090524, -1.443836447538996870 ) ) ;
#8686 = B_SPLINE_CURVE_WITH_KNOTS ( 'NONE', 3,
 ( #36793, #67755, #35306, #60148 ),
 .UNSPECIFIED., .F., .F.,
 ( 4, 4 ),
 ( 0.5709076711935395787, 0.5799141024656551124 ),
 .UNSPECIFIED. ) ;
#8688 = CARTESIAN_POINT ( 'NONE',  ( -31.62374207134597270, -24.66019654487199020, 8.947790411086133489 ) ) ;
#8689 = CARTESIAN_POINT ( 'NONE',  ( -19.15281226579456231, 4.489446101945751444, 11.49999999999999645 ) ) ;
#8690 = DIRECTION ( 'NONE',  ( -1.000000000000000000, -1.655121434032222977E-15, 0.000000000000000000 ) ) ;
#8691 = CARTESIAN_POINT ( 'NONE',  ( 14.56700794487395534, -4.079493581517788847, -28.22524715676654594 ) ) ;
#8692 = ORIENTED_EDGE ( 'NONE', *, *, #98529, .T. ) ;
#8693 = EDGE_CURVE ( 'NONE', #70837, #76528, #90776, .T. ) ;
#8694 = LINE ( 'NONE', #93409, #32813 ) ;
#8695 = CARTESIAN_POINT ( 'NONE',  ( -75.62287095715005592, -29.50250786944525672, 11.44777988621623521 ) ) ;
#8696 = LINE ( 'NONE', #93918, #53105 ) ;
#8697 = EDGE_CURVE ( 'NONE', #18133, #12639, #60841, .T. ) ;
#8698 = CARTESIAN_POINT ( 'NONE',  ( -40.52287095715006870, -29.50248528299804818, 1.056150453629031594 ) ) ;
#8699 = AXIS2_PLACEMENT_3D ( 'NONE', #34550, #11207, #73118 ) ;
#8700 = CARTESIAN_POINT ( 'NONE',  ( 14.33573519231038063, 13.56928687979844561, -1.500000000000002220 ) ) ;
#8701 = EDGE_CURVE ( 'NONE', #61677, #13991, #84554, .T. ) ;
#8702 = ORIENTED_EDGE ( 'NONE', *, *, #53860, .T. ) ;
#8703 = CARTESIAN_POINT ( 'NONE',  ( 9.818046095181445665, 6.376774720513751937, -28.04791983960493695 ) ) ;
#8704 = AXIS2_PLACEMENT_3D ( 'NONE', #23781, #64385, #31903 ) ;
#8705 = CALENDAR_DATE ( 2026, 9, 10 ) ;
#8706 = EDGE_LOOP ( 'NONE', ( #29697, #46836, #21403, #4783 ) ) ;
#8707 = CARTESIAN_POINT ( 'NONE',  ( -70.27422298781921484, -25.30465073045868252, 4.851635164186505200 ) ) ;
#8708 = CARTESIAN_POINT ( 'NONE',  ( 16.30000000000000071, 0.000000000000000000, 18.35000000000000142 ) ) ;
#8709 = CARTESIAN_POINT ( 'NONE',  ( -80.77170908772370694, -25.30559281118826220, 4.999461766569205601 ) ) ;
#8710 = FACE_OUTER_BOUND ( 'NONE', #78899, .T. ) ;
#8711 = CARTESIAN_POINT ( 'NONE',  ( -1.318699232124953324, -5.876774720514411854, 19.74039977944280722 ) ) ;
#8712 = DIRECTION ( 'NONE',  ( -0.9888510809027408754, 0.000000000000000000, -0.1489078231574183231 ) ) ;
#8713 = VECTOR ( 'NONE', #85666, 1000.000000000000114 ) ;
#8714 = CARTESIAN_POINT ( 'NONE',  ( -11.16000000000000014, -10.65233964170348635, -1.621096496867198589 ) ) ;
#8715 = CARTESIAN_POINT ( 'NONE',  ( 11.47056939498152950, -16.38825109899074661, 11.49999999999998934 ) ) ;
#8716 = CARTESIAN_POINT ( 'NONE',  ( -34.58953762381672448, -24.64898659630367206, 1.056161002820377393 ) ) ;
#8717 = PLANE ( 'NONE',  #28981 ) ;
#8718 = VERTEX_POINT ( 'NONE', #53223 ) ;
#8719 = B_SPLINE_CURVE_WITH_KNOTS ( 'NONE', 3,
 ( #62985, #77668, #31507, #56376, #86296, #25401, #54862, #62469, #46745, #8177, #54360, #9679, #87297, #85292, #24397, #46237, #93398, #7673, #15779 ),
 .UNSPECIFIED., .F., .F.,
 ( 4, 1, 1, 1, 1, 1, 1, 1, 1, 1, 1, 1, 1, 1, 1, 1, 4 ),
 ( 0.000000000000000000, 0.08252970382206502309, 0.1587788549175692676, 0.2277380621151786910, 0.2899456527966748909, 0.3454988386981381332, 0.3938963373401223600, 0.4363737851900878484, 0.4721222744615228284, 0.5363836155048271603, 0.5990779017254961314, 0.6619482340244576823, 0.7263105423531555083, 0.7917711030502102565, 0.8586473037978576972, 0.9273053338076845398, 1.000000000000000000 ),
 .UNSPECIFIED. ) ;
#8720 = CARTESIAN_POINT ( 'NONE',  ( -79.58202135401835164, -24.66019654487199375, 8.947790411086119278 ) ) ;
#8721 = CARTESIAN_POINT ( 'NONE',  ( -109.3584176993576591, -25.29012923716278749, 4.206202503440089835 ) ) ;
#8722 = CARTESIAN_POINT ( 'NONE',  ( -35.64597012725812419, -24.40034930558991277, 0.3402023900116170063 ) ) ;
#8723 = CARTESIAN_POINT ( 'NONE',  ( -108.5228709571500900, -24.33832256527048798, 0.1851278514138625098 ) ) ;
#8724 = B_SPLINE_CURVE_WITH_KNOTS ( 'NONE', 3,
 ( #85192, #47149, #46649, #77568 ),
 .UNSPECIFIED., .F., .F.,
 ( 4, 4 ),
 ( 1.387778780781445676E-17, 9.999999999997510880E-05 ),
 .UNSPECIFIED. ) ;
#8725 = CARTESIAN_POINT ( 'NONE',  ( -119.4728709570019589, -25.40556189117671693, 4.803963375099986166 ) ) ;
#8726 = FACE_OUTER_BOUND ( 'NONE', #10506, .T. ) ;
#8727 = CARTESIAN_POINT ( 'NONE',  ( -2.889365861140832159, -5.876774720514410966, 19.43823095447973870 ) ) ;
#8728 = DIRECTION ( 'NONE',  ( -0.000000000000000000, 1.000000000000000000, -0.000000000000000000 ) ) ;
#8729 = VERTEX_POINT ( 'NONE', #84151 ) ;
#8730 = CARTESIAN_POINT ( 'NONE',  ( 20.05935882324986963, -3.104462954613115500, 11.49999999999998934 ) ) ;
#8731 = FACE_OUTER_BOUND ( 'NONE', #39071, .T. ) ;
#8732 = CIRCLE ( 'NONE', #11995, 251.4258649670780699 ) ;
#8733 = CARTESIAN_POINT ( 'NONE',  ( -59.53433122793244081, -24.66019654487199730, 8.947790411086124607 ) ) ;
#8734 = ORIENTED_EDGE ( 'NONE', *, *, #51282, .F. ) ;
#8735 = PLANE ( 'NONE',  #4787 ) ;
#8736 = CARTESIAN_POINT ( 'NONE',  ( -18.21026628907936029, 8.684577975296603469, -1.500000000000002220 ) ) ;
#8737 = AXIS2_PLACEMENT_3D ( 'NONE', #9230, #48821, #78232 ) ;
#8738 = CARTESIAN_POINT ( 'NONE',  ( 1.363997202867437863, 21.09336101032836908, 11.49999999999999645 ) ) ;
#8739 = CARTESIAN_POINT ( 'NONE',  ( -15.83042281971428977, -15.45127431894796466, 11.49999999999998934 ) ) ;
#8740 = CARTESIAN_POINT ( 'NONE',  ( -20.42507745660439156, -2.452541965221147535, 11.49999999999998934 ) ) ;
#8741 = EDGE_CURVE ( 'NONE', #79654, #71653, #42919, .T. ) ;
#8742 = CARTESIAN_POINT ( 'NONE',  ( -60.58057154149170032, -24.83618233451449697, 1.606449574219536380 ) ) ;
#8743 = ORIENTED_EDGE ( 'NONE', *, *, #13912, .F. ) ;
#8744 = CARTESIAN_POINT ( 'NONE',  ( -32.62287095715004881, -23.72747288104469732, -1.053458166803227902 ) ) ;
#8745 = ORIENTED_EDGE ( 'NONE', *, *, #21123, .F. ) ;
#8746 = CARTESIAN_POINT ( 'NONE',  ( -57.62287095715004881, -23.48786465467241058, 11.44779295918254824 ) ) ;
#8747 = CARTESIAN_POINT ( 'NONE',  ( 22.81105451610979173, 6.475225279485573360, -20.71691820600746681 ) ) ;
#8748 = VERTEX_POINT ( 'NONE', #40493 ) ;
#8749 = EDGE_LOOP ( 'NONE', ( #24867, #52643, #28795 ) ) ;
#8750 = VERTEX_POINT ( 'NONE', #70440 ) ;
#8751 = CARTESIAN_POINT ( 'NONE',  ( -110.3139465455115271, -25.12049752546738191, 2.832404795212222659 ) ) ;
#8752 = CARTESIAN_POINT ( 'NONE',  ( 6.792576760808763936, -6.376774720514415407, 20.16775508794004779 ) ) ;
#8753 = CARTESIAN_POINT ( 'NONE',  ( 0.2428503871269292180, -6.376774720514413630, 19.85590024959437017 ) ) ;
#8754 = CARTESIAN_POINT ( 'NONE',  ( -19.50335911044312098, -6.847048061534898977, -1.500000000000002220 ) ) ;
#8755 = CARTESIAN_POINT ( 'NONE',  ( 9.217229664113554932, 19.63635308506117383, 11.49999999999999645 ) ) ;
#8756 = ORIENTED_EDGE ( 'NONE', *, *, #27309, .T. ) ;
#8757 = EDGE_CURVE ( 'NONE', #29214, #76528, #36792, .T. ) ;
#8758 = CARTESIAN_POINT ( 'NONE',  ( -46.55620429048337883, -24.64965694238575011, 8.947790433994201820 ) ) ;
#8759 = CARTESIAN_POINT ( 'NONE',  ( 3.052815417670126319, -5.876774720514407413, 18.46676085997033923 ) ) ;
#8760 = CARTESIAN_POINT ( 'NONE',  ( -11.14805103425725719, -19.39388463112642214, 11.49999999999998934 ) ) ;
#8761 = EDGE_CURVE ( 'NONE', #16980, #23842, #36035, .T. ) ;
#8762 = ADVANCED_FACE ( 'NONE', ( #69931 ), #1434, .T. ) ;
#8763 = CARTESIAN_POINT ( 'NONE',  ( -79.39179774623507058, -25.12205638436979882, 6.303984304149410356 ) ) ;
#8764 = CARTESIAN_POINT ( 'NONE',  ( -101.5228709571500474, -24.33927499327855415, 9.819080762295810061 ) ) ;
#8765 = EDGE_LOOP ( 'NONE', ( #17119, #26129, #90646, #35347 ) ) ;
#8766 = CARTESIAN_POINT ( 'NONE',  ( -118.3652930134189774, -25.31861658550455374, 6.462000913474522434 ) ) ;
#8767 = CARTESIAN_POINT ( 'NONE',  ( -35.65499668529189137, -24.15602025860895452, 10.28564288303536856 ) ) ;
#8768 = EDGE_CURVE ( 'NONE', #70766, #17712, #15142, .T. ) ;
#8769 = VERTEX_POINT ( 'NONE', #31877 ) ;
#8770 = CARTESIAN_POINT ( 'NONE',  ( -45.52287095715006870, -24.62285846331438677, 9.038163153548225637 ) ) ;
#8771 = ORIENTED_EDGE ( 'NONE', *, *, #53566, .F. ) ;
#8772 = CARTESIAN_POINT ( 'NONE',  ( -109.5151415522008023, -24.35071581493543391, 9.817618358456025263 ) ) ;
#8773 = CARTESIAN_POINT ( 'NONE',  ( -16.93204426113827310, 12.72334981527875186, -1.500000000000002220 ) ) ;
#8774 = ORIENTED_EDGE ( 'NONE', *, *, #17458, .F. ) ;
#8775 = CARTESIAN_POINT ( 'NONE',  ( 8.160000000000000142, -9.652339641703484574, -1.203735189656879756 ) ) ;
#8776 = CARTESIAN_POINT ( 'NONE',  ( -3.204121956075930200, -21.57847171274271858, 11.49999999999998934 ) ) ;
#8777 = CARTESIAN_POINT ( 'NONE',  ( -113.6228709571500417, -23.47596703998600631, 11.44779298504227860 ) ) ;
#8778 = FACE_OUTER_BOUND ( 'NONE', #16752, .T. ) ;
#8779 = CARTESIAN_POINT ( 'NONE',  ( -116.6228709571500417, -24.51283580621365843, 0.6167428607019838083 ) ) ;
#8780 = CARTESIAN_POINT ( 'NONE',  ( 6.711561834375728175, -20.75310922853297058, -1.500000000000002220 ) ) ;
#8781 = CARTESIAN_POINT ( 'NONE',  ( 6.403846153846157740, -6.376774720514426065, 21.48076923076922995 ) ) ;
#8782 = ORIENTED_EDGE ( 'NONE', *, *, #5333, .F. ) ;
#8783 = FACE_OUTER_BOUND ( 'NONE', #45727, .T. ) ;
#8784 = CARTESIAN_POINT ( 'NONE',  ( -85.55841537188921109, -23.85049219812685450, 10.88485053497527133 ) ) ;
#8785 = EDGE_CURVE ( 'NONE', #6907, #31632, #63348, .T. ) ;
#8786 = EDGE_LOOP ( 'NONE', ( #35320, #70752, #31595, #62069 ) ) ;
#8787 = ORIENTED_EDGE ( 'NONE', *, *, #81249, .F. ) ;
#8788 = EDGE_CURVE ( 'NONE', #43715, #34477, #14941, .T. ) ;
#8789 = ORIENTED_EDGE ( 'NONE', *, *, #68744, .T. ) ;
#8790 = CARTESIAN_POINT ( 'NONE',  ( -4.993225604111835914, -5.965225279485592225, -29.11654937215278593 ) ) ;
#8791 = CARTESIAN_POINT ( 'NONE',  ( -120.2228709571500644, -23.47593901973090524, -1.443836447538996426 ) ) ;
#8792 = CARTESIAN_POINT ( 'NONE',  ( -20.47598858559898716, 5.595549388561865456, 11.49999999999998934 ) ) ;
#8793 = CARTESIAN_POINT ( 'NONE',  ( -121.6228709571500843, -23.94994826722515668, -0.6494450866351686447 ) ) ;
#8794 = DIRECTION ( 'NONE',  ( -0.000000000000000000, 1.000000000000000000, -0.000000000000000000 ) ) ;
#8795 = AXIS2_PLACEMENT_3D ( 'NONE', #11087, #81601, #3489 ) ;
#8796 = EDGE_CURVE ( 'NONE', #23800, #37700, #58710, .T. ) ;
#8797 = CARTESIAN_POINT ( 'NONE',  ( -42.52287095715005449, -29.50247984919015209, -1.443849546365060466 ) ) ;
#8798 = DIRECTION ( 'NONE',  ( 3.773278334444166432E-23, -1.000000000000000000, 0.000000000000000000 ) ) ;
#8799 = CARTESIAN_POINT ( 'NONE',  ( 2.844571010020486845, -19.19604305453586690, -1.500000000000002220 ) ) ;
#8800 = CARTESIAN_POINT ( 'NONE',  ( -40.93937950312512442, -25.11539320593059443, 2.804431443241629740 ) ) ;
#8801 = ORIENTED_EDGE ( 'NONE', *, *, #87931, .T. ) ;
#8802 = CARTESIAN_POINT ( 'NONE',  ( 4.731349760756693890, 18.90081699332259646, 11.49999999999999645 ) ) ;
#8803 = FACE_OUTER_BOUND ( 'NONE', #19951, .T. ) ;
#8804 = LINE ( 'NONE', #39243, #25312 ) ;
#8805 = ORIENTED_EDGE ( 'NONE', *, *, #36622, .F. ) ;
#8806 = ADVANCED_FACE ( 'NONE', ( #93767 ), #24257, .T. ) ;
#8807 = VECTOR ( 'NONE', #79511, 1000.000000000000000 ) ;
#8808 = CARTESIAN_POINT ( 'NONE',  ( -58.62287095715005592, -24.33927499327854704, 9.819080762295822495 ) ) ;
#8809 = DIRECTION ( 'NONE',  ( -3.773278334453079618E-23, 0.9999999999976377785, 2.173523156925979975E-06 ) ) ;
#8811 = EDGE_CURVE ( 'NONE', #86043, #63083, #8537, .T. ) ;
#8810 = CARTESIAN_POINT ( 'NONE',  ( -106.5228709571500900, -23.72747288104470442, -1.053458166803224794 ) ) ;
#8812 = CARTESIAN_POINT ( 'NONE',  ( -93.55195563180954821, -24.15620529776628800, 10.23563542870659582 ) ) ;
#8813 = CARTESIAN_POINT ( 'NONE',  ( 16.09843989366402539, -11.26760994518913428, 11.49999999999998934 ) ) ;
#8814 = CARTESIAN_POINT ( 'NONE',  ( -117.6228709571500559, -24.51387760970724372, 9.387446482453409402 ) ) ;
#8815 = ORIENTED_EDGE ( 'NONE', *, *, #41531, .T. ) ;
#8816 = CARTESIAN_POINT ( 'NONE',  ( -18.50814150397365410, 11.09706937414969374, -1.500000000000002220 ) ) ;
#8817 = LINE ( 'NONE', #61623, #83071 ) ;
#8818 = DIRECTION ( 'NONE',  ( -0.6599726524652352877, 0.000000000000000000, 0.7512896232465891000 ) ) ;
#8819 = CARTESIAN_POINT ( 'NONE',  ( 23.08992502549420323, -0.8469403905869224980, -1.500000000000002220 ) ) ;
#8820 = PERSON_AND_ORGANIZATION_ROLE ( 'design_owner' ) ;
#8821 = CARTESIAN_POINT ( 'NONE',  ( -93.63360391309790032, -23.96119346886880663, -0.6495511937832079141 ) ) ;
#8822 = CARTESIAN_POINT ( 'NONE',  ( -90.52287095715006160, -23.84081130425357387, 10.88220057483158243 ) ) ;
#8823 = PLANE ( 'NONE',  #10456 ) ;
#8824 = DIRECTION ( 'NONE',  ( 0.000000000000000000, 0.000000000000000000, 1.000000000000000000 ) ) ;
#8825 = CARTESIAN_POINT ( 'NONE',  ( -111.7148472136480990, -25.10921600246400587, 3.873546110135351217 ) ) ;
#8826 = CARTESIAN_POINT ( 'NONE',  ( -124.6228709571500559, -23.48786465467241769, 11.44779295918253759 ) ) ;
#8827 = CARTESIAN_POINT ( 'NONE',  ( -114.5530339053627813, -24.35071581493544457, 9.817618358456016381 ) ) ;
#8828 = CARTESIAN_POINT ( 'NONE',  ( -19.91179686852411734, 0.6080443046932394457, -1.500000000000002220 ) ) ;
#8829 = CARTESIAN_POINT ( 'NONE',  ( -75.54218285077926964, -24.63419186844611275, 9.035850630976923981 ) ) ;
#8830 = CARTESIAN_POINT ( 'NONE',  ( -19.81728208556213389, 0.3677575464312098363, -1.500000000000002220 ) ) ;
#8831 = CARTESIAN_POINT ( 'NONE',  ( -0.1037292527911751056, -5.876774720514413630, 19.53657742262743824 ) ) ;
#8832 = CARTESIAN_POINT ( 'NONE',  ( -39.32379795506943054, -25.10925708289683911, 3.365606678701691834 ) ) ;
#8833 = VECTOR ( 'NONE', #39522, 1000.000000000000000 ) ;
#8834 = DIRECTION ( 'NONE',  ( 0.9975640502598247528, -0.06975647374411753088, 0.000000000000000000 ) ) ;
#8835 = CARTESIAN_POINT ( 'NONE',  ( -16.75865769207039335, -12.26659692683164593, 11.49999999999999645 ) ) ;
#8836 = PLANE ( 'NONE',  #41925 ) ;
#8837 = CARTESIAN_POINT ( 'NONE',  ( -106.5874661333381397, -24.51314013834316796, 0.6176544820404221703 ) ) ;
#8838 = CARTESIAN_POINT ( 'NONE',  ( -21.15473383059569557, 8.456223909384457116, 11.49999999999999645 ) ) ;
#8839 = ORIENTED_EDGE ( 'NONE', *, *, #1310, .F. ) ;
#8840 = CARTESIAN_POINT ( 'NONE',  ( -91.62287095715004170, -24.64898659630368627, 1.056161002820827921 ) ) ;
#8841 = CARTESIAN_POINT ( 'NONE',  ( -69.34303308397305443, -25.24554880456021522, 6.209207408033732278 ) ) ;
#8842 = ORIENTED_EDGE ( 'NONE', *, *, #50341, .F. ) ;
#8843 = CARTESIAN_POINT ( 'NONE',  ( -19.21899500656021331, -6.280627263257740900, 11.49999999999998934 ) ) ;
#8844 = PLANE ( 'NONE',  #79191 ) ;
#8845 = FACE_OUTER_BOUND ( 'NONE', #54105, .T. ) ;
#8846 = ORIENTED_EDGE ( 'NONE', *, *, #27384, .F. ) ;
#8847 = DIRECTION ( 'NONE',  ( 0.000000000000000000, -0.9999999999976377785, -2.173523156925979128E-06 ) ) ;
#8848 = CARTESIAN_POINT ( 'NONE',  ( 0.5590224530292132732, -22.91010021869659852, 11.49999999999998934 ) ) ;
#8849 = CARTESIAN_POINT ( 'NONE',  ( -50.43601667505130592, -25.27420563262489139, 3.294780489091903686 ) ) ;
#8850 = CARTESIAN_POINT ( 'NONE',  ( 18.80801646011137507, -6.797914457553222434, -1.500000000000002220 ) ) ;
#8851 = CARTESIAN_POINT ( 'NONE',  ( -41.26959558397305727, -25.07899898050004950, 7.338714981574760543 ) ) ;
#8852 = CARTESIAN_POINT ( 'NONE',  ( -20.44905293368100985, -4.654758753755802836, 11.49999999999999645 ) ) ;
#8853 = EDGE_LOOP ( 'NONE', ( #18878, #79136, #3344, #37036 ) ) ;
#8854 = CARTESIAN_POINT ( 'NONE',  ( -86.62287095715001328, -23.47596703998600631, 11.44779298504227683 ) ) ;
#8855 = CARTESIAN_POINT ( 'NONE',  ( -124.5888236901737969, -24.65952944569305316, 1.056160979905708563 ) ) ;
#8856 = CARTESIAN_POINT ( 'NONE',  ( -7.037580251249667462, -20.86201633182841420, -1.500000000000002220 ) ) ;
#8857 = VECTOR ( 'NONE', #68010, 1000.000000000000000 ) ;
#8858 = LINE ( 'NONE', #78853, #85200 ) ;
#8859 = ORIENTED_EDGE ( 'NONE', *, *, #26757, .T. ) ;
#8860 = B_SPLINE_CURVE_WITH_KNOTS ( 'NONE', 3,
 ( #38470, #8524, #62322, #23736, #47096, #73923 ),
 .UNSPECIFIED., .F., .F.,
 ( 4, 2, 4 ),
 ( 0.000000000000000000, 0.001380901958385384641, 0.002761803916770769283 ),
 .UNSPECIFIED. ) ;
#8861 = CARTESIAN_POINT ( 'NONE',  ( -49.86550021440504565, -25.18440128170155035, 3.414711424454316191 ) ) ;
#8862 = CARTESIAN_POINT ( 'NONE',  ( -126.6228709571500559, -29.50247984919015209, -1.443849546365044922 ) ) ;
#8863 = ORIENTED_EDGE ( 'NONE', *, *, #65199, .F. ) ;
#8864 = CARTESIAN_POINT ( 'NONE',  ( 3.183477995988301945, -6.376774720514404748, 18.35601591497023577 ) ) ;
#8865 = EDGE_CURVE ( 'NONE', #95482, #3899, #33186, .T. ) ;
#8866 = ORIENTED_EDGE ( 'NONE', *, *, #44279, .F. ) ;
#8867 = EDGE_CURVE ( 'NONE', #58528, #88521, #92484, .T. ) ;
#8868 = ORIENTED_EDGE ( 'NONE', *, *, #89096, .F. ) ;
#8869 = CARTESIAN_POINT ( 'NONE',  ( -25.92875734969025814, -3.316774720514426456, 23.50402280011861933 ) ) ;
#8870 = CARTESIAN_POINT ( 'NONE',  ( -101.0021142486707646, -25.27404655521463184, 2.948027157395776587 ) ) ;
#8871 = CARTESIAN_POINT ( 'NONE',  ( -36.53267038383642529, -24.51314013834317151, 0.6176544820404150649 ) ) ;
#8872 = CARTESIAN_POINT ( 'NONE',  ( -18.14515864413662172, 9.488524743509296755, -1.500000000000002220 ) ) ;
#8873 = B_SPLINE_CURVE_WITH_KNOTS ( 'NONE', 3,
 ( #7172, #7680, #18789, #93913 ),
 .UNSPECIFIED., .F., .F.,
 ( 4, 4 ),
 ( 0.000000000000000000, 9.999999999998897304E-05 ),
 .UNSPECIFIED. ) ;
#8874 = AXIS2_PLACEMENT_3D ( 'NONE', #33718, #4270, #11870 ) ;
#8875 = EDGE_CURVE ( 'NONE', #57442, #78612, #82957, .T. ) ;
#8876 = ORIENTED_EDGE ( 'NONE', *, *, #58380, .T. ) ;
#8877 = PLANE ( 'NONE',  #88270 ) ;
#8878 = CARTESIAN_POINT ( 'NONE',  ( -44.52977088278382922, -24.65952944569304606, 1.056160979905693909 ) ) ;
#8879 = CARTESIAN_POINT ( 'NONE',  ( -40.45829750704998418, -25.18492896333868103, 3.293943116708551777 ) ) ;
#8880 = CARTESIAN_POINT ( 'NONE',  ( 22.30035941410032763, -0.3387204123245128873, 11.49999999999998934 ) ) ;
#8881 = EDGE_CURVE ( 'NONE', #36540, #54139, #61340, .T. ) ;
#8882 = CARTESIAN_POINT ( 'NONE',  ( -70.62782063829519075, -25.14001972948981134, 7.062078543324224356 ) ) ;
#8883 = CARTESIAN_POINT ( 'NONE',  ( -27.51755584304929414, -24.62734232575839144, 8.245802515575128666 ) ) ;
#8884 = EDGE_LOOP ( 'NONE', ( #92043, #16100, #98962, #74650 ) ) ;
#8885 = CARTESIAN_POINT ( 'NONE',  ( -28.07868692527382493, -24.64332086767980101, 1.662177252415085293 ) ) ;
#8886 = CARTESIAN_POINT ( 'NONE',  ( -73.52287095715007581, -24.65952944569304606, 1.056160979905697239 ) ) ;
#8887 = CARTESIAN_POINT ( 'NONE',  ( -12.81329989551134751, 16.42372500408851366, -1.500000000000002220 ) ) ;
#8888 = ORIENTED_EDGE ( 'NONE', *, *, #33182, .F. ) ;
#8890 = ORIENTED_EDGE ( 'NONE', *, *, #93486, .F. ) ;
#8889 = CARTESIAN_POINT ( 'NONE',  ( 0.03625801282051022839, -6.376774720514410077, 19.27714342948718240 ) ) ;
#8891 = ORIENTED_EDGE ( 'NONE', *, *, #62740, .T. ) ;
#8892 = CARTESIAN_POINT ( 'NONE',  ( -31.52287095715006160, -24.65952944569304606, 1.056160979905690134 ) ) ;
#8893 = CARTESIAN_POINT ( 'NONE',  ( 0.9685562702117149758, 20.96446713366763248, -1.500000000000002220 ) ) ;
#8894 = VERTEX_POINT ( 'NONE', #54227 ) ;
#8895 = CARTESIAN_POINT ( 'NONE',  ( 5.717391271363888805, -6.376774720514426953, -25.39218285751184467 ) ) ;
#8896 = CARTESIAN_POINT ( 'NONE',  ( -53.52287095715007581, -24.33927499327856125, 9.819080762295815390 ) ) ;
#8897 = DIRECTION ( 'NONE',  ( 0.000000000000000000, 0.000000000000000000, 1.000000000000000000 ) ) ;
#8898 = CARTESIAN_POINT ( 'NONE',  ( -101.6175123368144142, -25.03152335046257448, 7.038108615052007799 ) ) ;
#8899 = CARTESIAN_POINT ( 'NONE',  ( -60.62287095715004881, -24.14406661707768365, 10.28769366152059739 ) ) ;
#8900 = CARTESIAN_POINT ( 'NONE',  ( -64.52287095715006160, -23.47596703998600631, 11.44779298504228926 ) ) ;
#8902 = VERTEX_POINT ( 'NONE', #85152 ) ;
#8901 = CARTESIAN_POINT ( 'NONE',  ( -18.13406196532287140, 12.77545654309102474, 11.49999999999999645 ) ) ;
#8903 = LINE ( 'NONE', #39849, #33982 ) ;
#8904 = DIRECTION ( 'NONE',  ( 0.000000000000000000, 0.000000000000000000, 1.000000000000000000 ) ) ;
#8905 = ORIENTED_EDGE ( 'NONE', *, *, #59755, .T. ) ;
#8906 = CARTESIAN_POINT ( 'NONE',  ( 12.64511023617726160, -18.80563239904246231, -1.500000000000002220 ) ) ;
#8908 = ORIENTED_EDGE ( 'NONE', *, *, #99060, .T. ) ;
#8907 = LINE ( 'NONE', #25122, #36085 ) ;
#8909 = VERTEX_POINT ( 'NONE', #15642 ) ;
#8910 = CIRCLE ( 'NONE', #34852, 2.499999999999996891 ) ;
#8911 = LINE ( 'NONE', #301, #58024 ) ;
#8912 = CARTESIAN_POINT ( 'NONE',  ( -14.30055291515510518, -14.21740073472259525, -1.500000000000002220 ) ) ;
#8913 = FACE_OUTER_BOUND ( 'NONE', #20132, .T. ) ;
#8914 = ORIENTED_EDGE ( 'NONE', *, *, #78625, .T. ) ;
#8915 = CARTESIAN_POINT ( 'NONE',  ( -92.55620429048340725, -23.48786465467241413, 11.44779295918254292 ) ) ;
#8916 = CARTESIAN_POINT ( 'NONE',  ( 0.2029947971921062799, -22.41465419638480228, -1.500000000000002220 ) ) ;
#8917 = ORIENTED_EDGE ( 'NONE', *, *, #653, .F. ) ;
#8918 = ORIENTED_EDGE ( 'NONE', *, *, #6415, .F. ) ;
#8919 = LINE ( 'NONE', #3336, #69248 ) ;
#8920 = CARTESIAN_POINT ( 'NONE',  ( -94.58861374093797281, -24.35071581493543036, 9.817618358456030592 ) ) ;
#8921 = CARTESIAN_POINT ( 'NONE',  ( -35.52287095715006870, -29.50249982740957577, 7.747779886224967605 ) ) ;
#8922 = CARTESIAN_POINT ( 'NONE',  ( -89.40841769935767047, -29.50248914370730091, 2.832395270851967073 ) ) ;
#8924 = EDGE_CURVE ( 'NONE', #91672, #71483, #31371, .T. ) ;
#8923 = CARTESIAN_POINT ( 'NONE',  ( -97.25938467801201170, -23.78062553189672812, -0.9709657327914289482 ) ) ;
#8925 = B_SPLINE_CURVE_WITH_KNOTS ( 'NONE', 3,
 ( #38225, #46345, #21990, #30114, #14884, #1554 ),
 .UNSPECIFIED., .F., .F.,
 ( 4, 2, 4 ),
 ( 0.000000000000000000, 0.001380764517853247083, 0.002761529035706494165 ),
 .UNSPECIFIED. ) ;
#8926 = CARTESIAN_POINT ( 'NONE',  ( 2.510080532074158377, -19.39449211012750496, 11.49999999999998934 ) ) ;
#8927 = DIRECTION ( 'NONE',  ( 1.000000000000000000, -0.000000000000000000, -0.000000000000000000 ) ) ;
#8928 = ORIENTED_EDGE ( 'NONE', *, *, #76342, .T. ) ;
#8929 = CARTESIAN_POINT ( 'NONE',  ( 21.49998558720804809, 0.1351929536555107336, 11.49999999999998934 ) ) ;
#8930 = CARTESIAN_POINT ( 'NONE',  ( -62.52287095715009002, -24.51387760970724372, 9.387446482453405849 ) ) ;
#8931 = DIRECTION ( 'NONE',  ( 0.000000000000000000, 1.000000000000000000, 0.000000000000000000 ) ) ;
#8932 = CARTESIAN_POINT ( 'NONE',  ( 0.000000000000000000, -4.056774720514426669, 3.500000000000000000 ) ) ;
#8933 = EDGE_CURVE ( 'NONE', #15581, #29598, #18639, .T. ) ;
#8934 = CARTESIAN_POINT ( 'NONE',  ( 31.84105487026623393, -5.152774720514427642, -11.95870468328481806 ) ) ;
#8936 = VECTOR ( 'NONE', #29815, 1000.000000000000114 ) ;
#8935 = CARTESIAN_POINT ( 'NONE',  ( 17.95915693031428262, 14.28781372813260120, -1.500000000000002220 ) ) ;
#8937 = APPLICATION_PROTOCOL_DEFINITION ( 'international standard', 'config_control_design', 1994, #34267 ) ;
#8938 = CARTESIAN_POINT ( 'NONE',  ( -120.6228709571500701, -25.00158670708909625, 2.256160236439166411 ) ) ;
#8939 = CARTESIAN_POINT ( 'NONE',  ( -92.62287095715005592, -23.47593901973091235, -1.443836447539002865 ) ) ;
#8940 = CARTESIAN_POINT ( 'NONE',  ( 14.85562765054232059, -13.46834898924134372, 11.49999999999999645 ) ) ;
#8941 = CARTESIAN_POINT ( 'NONE',  ( -79.04068788000392942, -25.31594508206281802, 5.390100702044224867 ) ) ;
#8942 = CARTESIAN_POINT ( 'NONE',  ( 30.53060340732036693, 4.740362442169048229, -2.970849955429423872 ) ) ;
#8943 = FACE_OUTER_BOUND ( 'NONE', #88476, .T. ) ;
#8944 = CARTESIAN_POINT ( 'NONE',  ( 26.73860345374794178, 1.477225279485574028, -1.272392034746785860 ) ) ;
#8945 = ORIENTED_EDGE ( 'NONE', *, *, #31472, .F. ) ;
#8946 = CARTESIAN_POINT ( 'NONE',  ( -65.62287095715005592, -23.47593901973091235, -1.443836447539006196 ) ) ;
#8947 = AXIS2_PLACEMENT_3D ( 'NONE', #58463, #48852, #10274 ) ;
#8948 = CARTESIAN_POINT ( 'NONE',  ( -19.00758693998263738, -10.61793046214600089, -1.500000000000002220 ) ) ;
#8949 = CARTESIAN_POINT ( 'NONE',  ( -22.05275734969026047, -5.965225279485572685, 31.02402280011862246 ) ) ;
#8950 = CARTESIAN_POINT ( 'NONE',  ( -11.91260469445801995, 15.66180005371307260, -1.500000000000002220 ) ) ;
#8951 = VECTOR ( 'NONE', #72778, 1000.000000000000000 ) ;
#8952 = PLANE ( 'NONE',  #71875 ) ;
#8953 = B_SPLINE_CURVE_WITH_KNOTS ( 'NONE', 3,
 ( #45382, #58599, #66736, #74806, #37260, #60610, #12409, #28151 ),
 .UNSPECIFIED., .F., .F.,
 ( 4, 2, 2, 4 ),
 ( 6.391158118972243699E-06, 0.002007136338672931355, 0.003007508928949908632, 0.004007881519226886777 ),
 .UNSPECIFIED. ) ;
#8954 = DIRECTION ( 'NONE',  ( 0.000000000000000000, -2.173523156925979552E-06, 0.9999999999976378895 ) ) ;
#8955 = CARTESIAN_POINT ( 'NONE',  ( 9.278253834636473130, -5.876774720514426953, 21.78128695274316229 ) ) ;
#8956 = CARTESIAN_POINT ( 'NONE',  ( -6.499999999999992895, 0.000000000000000000, -2.500000000000001332 ) ) ;
#8957 = CARTESIAN_POINT ( 'NONE',  ( -6.092534927433182368, -19.63929903328317295, 11.49999999999999645 ) ) ;
#8958 = CARTESIAN_POINT ( 'NONE',  ( 4.487249349319938574, -5.876774720514419847, 21.01618089687719504 ) ) ;
#8959 = DIRECTION ( 'NONE',  ( -3.773278334453079618E-23, 0.9999999999976377785, 2.173523156925978705E-06 ) ) ;
#8960 = CARTESIAN_POINT ( 'NONE',  ( 19.70651319644445465, -11.07993823016455792, 11.49999999999999645 ) ) ;
#8961 = ORIENTED_EDGE ( 'NONE', *, *, #55002, .F. ) ;
#8962 = FACE_OUTER_BOUND ( 'NONE', #51305, .T. ) ;
#8963 = FACE_OUTER_BOUND ( 'NONE', #12111, .T. ) ;
#8964 = CARTESIAN_POINT ( 'NONE',  ( -125.6238069808063642, -24.83644354573579349, 8.397322867130096569 ) ) ;
#8965 = FACE_OUTER_BOUND ( 'NONE', #30901, .T. ) ;
#8966 = B_SPLINE_CURVE_WITH_KNOTS ( 'NONE', 3,
 ( #40156, #32541, #87837, #17821 ),
 .UNSPECIFIED., .F., .F.,
 ( 4, 4 ),
 ( 2.791380378375079153E-06, 0.0004665020696472202692 ),
 .UNSPECIFIED. ) ;
#8967 = CARTESIAN_POINT ( 'NONE',  ( -25.74405688418818272, -24.93063286172094450, 6.647229298724505853 ) ) ;
#8968 = LINE ( 'NONE', #78972, #96580 ) ;
#8969 = ORIENTED_EDGE ( 'NONE', *, *, #94638, .T. ) ;
#8970 = CARTESIAN_POINT ( 'NONE',  ( 22.95697726795019378, -2.620641032420567118, 11.49999999999999645 ) ) ;
#8971 = CARTESIAN_POINT ( 'NONE',  ( 21.82588152991271713, 6.770963248321698380, -1.500000000000002220 ) ) ;
#8972 = CARTESIAN_POINT ( 'NONE',  ( 4.593956459244529889, -5.876774720514410077, 19.29001220640957115 ) ) ;
#8973 = CARTESIAN_POINT ( 'NONE',  ( -96.58868282968654739, -24.34968618360933945, 0.1864209137778869152 ) ) ;
#8974 = CARTESIAN_POINT ( 'NONE',  ( -82.56324868667182670, -23.48786465467241413, 11.44779295918254824 ) ) ;
#8975 = VECTOR ( 'NONE', #97695, 1000.000000000000000 ) ;
#8976 = CARTESIAN_POINT ( 'NONE',  ( 3.503984654965784706, -22.18958196551723816, 11.49999999999999645 ) ) ;
#8977 = VERTEX_POINT ( 'NONE', #42507 ) ;
#8978 = FACE_OUTER_BOUND ( 'NONE', #3453, .T. ) ;
#8979 = CARTESIAN_POINT ( 'NONE',  ( -21.09739860443290382, 5.981408608369527258, 11.49999999999998934 ) ) ;
#8980 = CARTESIAN_POINT ( 'NONE',  ( 11.62916340711181284, 5.965225279485572685, 28.75961759920349792 ) ) ;
#8981 = CARTESIAN_POINT ( 'NONE',  ( -34.64979159594478375, -23.96169478059712077, 10.65365249895718769 ) ) ;
#8982 = CARTESIAN_POINT ( 'NONE',  ( -121.5228709571500758, -24.33927499327855770, 9.819080762295813614 ) ) ;
#8983 = ORIENTED_EDGE ( 'NONE', *, *, #1858, .F. ) ;
#8984 = CARTESIAN_POINT ( 'NONE',  ( -48.65308815567226475, -23.73791477778911840, 11.05961554403170766 ) ) ;
#8985 = CYLINDRICAL_SURFACE ( 'NONE', #100309, 1.325999999999990298 ) ;
#8986 = ORIENTED_EDGE ( 'NONE', *, *, #20791, .F. ) ;
#8987 = EDGE_CURVE ( 'NONE', #18949, #56586, #65358, .T. ) ;
#8988 = CARTESIAN_POINT ( 'NONE',  ( -20.02755620033356010, -4.236777897013602079, 11.49999999999998934 ) ) ;
#8989 = VERTEX_POINT ( 'NONE', #17649 ) ;
#8990 = ORIENTED_EDGE ( 'NONE', *, *, #4337, .F. ) ;
#8991 = ORIENTED_EDGE ( 'NONE', *, *, #56789, .F. ) ;
#8992 = EDGE_LOOP ( 'NONE', ( #67059, #85478, #48107, #23002, #79787 ) ) ;
#8993 = CARTESIAN_POINT ( 'NONE',  ( 10.36671515591691950, -20.60271000134967068, 11.49999999999998934 ) ) ;
#8994 = CYLINDRICAL_SURFACE ( 'NONE', #74677, 24.00000000000000000 ) ;
#8995 = CARTESIAN_POINT ( 'NONE',  ( -19.79944955726156763, -4.570829099900970860, -1.500000000000002220 ) ) ;
#8996 = EDGE_CURVE ( 'NONE', #97579, #48183, #83849, .T. ) ;
#8997 = ORIENTED_EDGE ( 'NONE', *, *, #75443, .F. ) ;
#8998 = CARTESIAN_POINT ( 'NONE',  ( -97.52287095715006160, -24.64965694238575011, 8.947790433994194714 ) ) ;
#8999 = CARTESIAN_POINT ( 'NONE',  ( -73.52287095715007581, -23.48786465467241058, 11.44779295918254647 ) ) ;
#9000 = EDGE_CURVE ( 'NONE', #67804, #26531, #16534, .T. ) ;
#9001 = DIRECTION ( 'NONE',  ( 3.773278334444167608E-23, -1.000000000000000000, 0.000000000000000000 ) ) ;
#9002 = CARTESIAN_POINT ( 'NONE',  ( -70.53236091209835479, -25.00158670708910691, 2.256160236439221034 ) ) ;
#9004 = EDGE_LOOP ( 'NONE', ( #27987, #90613, #13601, #33123 ) ) ;
#9003 = CARTESIAN_POINT ( 'NONE',  ( 16.66814584454133907, -13.58961022886752978, 11.49999999999999645 ) ) ;
#9005 = CARTESIAN_POINT ( 'NONE',  ( -79.55620429048339304, -24.66019654487199375, 8.947790411086131712 ) ) ;
#9006 = CARTESIAN_POINT ( 'NONE',  ( -104.6228709571500559, -23.47593901973091235, -1.443836447539001089 ) ) ;
#9007 = EDGE_CURVE ( 'NONE', #31838, #96235, #92308, .T. ) ;
#9008 = ORIENTED_EDGE ( 'NONE', *, *, #99589, .F. ) ;
#9009 = EDGE_CURVE ( 'NONE', #52065, #67869, #49617, .T. ) ;
#9010 = CARTESIAN_POINT ( 'NONE',  ( 18.38559056850662543, 9.607341378227904016, 11.49999999999998934 ) ) ;
#9011 = ORIENTED_EDGE ( 'NONE', *, *, #61711, .T. ) ;
#9013 = VERTEX_POINT ( 'NONE', #42998 ) ;
#9012 = CARTESIAN_POINT ( 'NONE',  ( -125.5543386547933977, -24.83618233451450763, 1.606449574219537046 ) ) ;
#9014 = CIRCLE ( 'NONE', #88401, 84.48086791635432746 ) ;
#9015 = CARTESIAN_POINT ( 'NONE',  ( -111.5936678842673331, -23.73791477778912551, 11.05961554403170055 ) ) ;
#9016 = DIRECTION ( 'NONE',  ( 0.000000000000000000, -1.000000000000000000, 0.000000000000000000 ) ) ;
#9017 = ORIENTED_EDGE ( 'NONE', *, *, #90910, .T. ) ;
#9018 = ORIENTED_EDGE ( 'NONE', *, *, #91792, .F. ) ;
#9019 = CARTESIAN_POINT ( 'NONE',  ( -58.87764846858842560, -29.50248939449842922, 2.947779886236309377 ) ) ;
#9020 = CARTESIAN_POINT ( 'NONE',  ( -42.62869147627655053, -24.51419770103158413, 9.386484678747191168 ) ) ;
#9021 = AXIS2_PLACEMENT_3D ( 'NONE', #58483, #36130, #49878 ) ;
#9022 = ADVANCED_FACE ( 'NONE', ( #12031 ), #95774, .F. ) ;
#9023 = CARTESIAN_POINT ( 'NONE',  ( -29.36337478090402797, -24.98585162628100420, 2.615322239748779420 ) ) ;
#9024 = CARTESIAN_POINT ( 'NONE',  ( 16.65356921002588919, 14.36988287374134821, 11.49999999999999645 ) ) ;
#9025 = AXIS2_PLACEMENT_3D ( 'NONE', #36497, #28890, #58849 ) ;
#9026 = FACE_BOUND ( 'NONE', #64000, .T. ) ;
#9027 = CARTESIAN_POINT ( 'NONE',  ( -17.80605238980536953, 13.89162706601689479, -1.500000000000002220 ) ) ;
#9028 = CARTESIAN_POINT ( 'NONE',  ( 6.892386425805808514, -19.84609432511738447, 11.49999999999998934 ) ) ;
#9030 = ORIENTED_EDGE ( 'NONE', *, *, #94900, .T. ) ;
#9029 = FACE_OUTER_BOUND ( 'NONE', #75515, .T. ) ;
#9031 = ORIENTED_EDGE ( 'NONE', *, *, #40405, .F. ) ;
#9032 = DIRECTION ( 'NONE',  ( 0.000000000000000000, -2.173523156925979552E-06, 0.9999999999976378895 ) ) ;
#9033 = CARTESIAN_POINT ( 'NONE',  ( -90.62287095715005592, -24.62285846362216546, 9.038163152653526211 ) ) ;
#9034 = ORIENTED_EDGE ( 'NONE', *, *, #74757, .T. ) ;
#9035 = CARTESIAN_POINT ( 'NONE',  ( 20.98173926746349238, 2.650078317256617577, -1.500000000000002220 ) ) ;
#9036 = CARTESIAN_POINT ( 'NONE',  ( -0.4362980769230789257, -6.376774720514411854, 19.46153846153846345 ) ) ;
#9037 = CARTESIAN_POINT ( 'NONE',  ( -51.32936205048392964, -25.26041064547814941, 7.321355772070240242 ) ) ;
#9038 = CARTESIAN_POINT ( 'NONE',  ( -121.5192093918902572, -24.34968618360933945, 0.1864209137778886083 ) ) ;
#9039 = LINE ( 'NONE', #84661, #2208 ) ;
#9040 = CARTESIAN_POINT ( 'NONE',  ( -101.5228709571501327, -23.96127896941632329, -0.6493128931038008034 ) ) ;
#9041 = CARTESIAN_POINT ( 'NONE',  ( -4.073883676365832152, 21.86232641878667593, -1.500000000000002220 ) ) ;
#9042 = FACE_OUTER_BOUND ( 'NONE', #21629, .T. ) ;
#9043 = ADVANCED_FACE ( 'NONE', ( #57729 ), #25255, .F. ) ;
#9044 = EDGE_LOOP ( 'NONE', ( #3421, #68783 ) ) ;
#9045 = CARTESIAN_POINT ( 'NONE',  ( -51.26059310326842677, -25.24860019069869210, 5.062966105152178820 ) ) ;
#9046 = DIRECTION ( 'NONE',  ( -0.000000000000000000, 1.000000000000000000, -0.000000000000000000 ) ) ;
#9047 = FACE_OUTER_BOUND ( 'NONE', #11042, .T. ) ;
#9048 = EDGE_CURVE ( 'NONE', #73282, #75171, #93551, .T. ) ;
#9049 = DIRECTION ( 'NONE',  ( 0.000000000000000000, 0.000000000000000000, -1.000000000000000000 ) ) ;
#9050 = CARTESIAN_POINT ( 'NONE',  ( 26.73860345374794534, -1.682774720514426114, -7.113848178280766099 ) ) ;
#9051 = CARTESIAN_POINT ( 'NONE',  ( 18.45204572605500104, 6.281640480902235701, -1.500000000000002220 ) ) ;
#9052 = VECTOR ( 'NONE', #62013, 1000.000000000000000 ) ;
#9053 = CARTESIAN_POINT ( 'NONE',  ( -20.52298544035203776, 6.160189734329080125, -1.500000000000002220 ) ) ;
#9054 = CARTESIAN_POINT ( 'NONE',  ( -85.52287095715004739, -24.62285846331436190, 9.038163153548291362 ) ) ;
#9055 = CYLINDRICAL_SURFACE ( 'NONE', #20369, 3.979149600822063704 ) ;
#9056 = PLANE ( 'NONE',  #34147 ) ;
#9057 = FACE_OUTER_BOUND ( 'NONE', #51176, .T. ) ;
#9058 = CARTESIAN_POINT ( 'NONE',  ( 17.68435195917723490, -14.24712819257710095, -1.500000000000002220 ) ) ;
#9059 = B_SPLINE_CURVE_WITH_KNOTS ( 'NONE', 3,
 ( #28657, #59121, #92045, #44392 ),
 .UNSPECIFIED., .F., .F.,
 ( 4, 4 ),
 ( 0.4408147750407612198, 0.4498212063128765870 ),
 .UNSPECIFIED. ) ;
#9060 = EDGE_CURVE ( 'NONE', #94938, #43985, #41494, .T. ) ;
#9061 = CARTESIAN_POINT ( 'NONE',  ( -103.6228709571500417, -24.65952944569304606, 1.056160979905701680 ) ) ;
#9062 = CARTESIAN_POINT ( 'NONE',  ( -80.52287095715004739, -24.62226745350437440, 0.9660975649728149595 ) ) ;
#9063 = CARTESIAN_POINT ( 'NONE',  ( 19.75055111929153639, -1.948201398878238066, 11.49999999999999645 ) ) ;
#9064 = CARTESIAN_POINT ( 'NONE',  ( -61.64687923781919210, -25.21083105912962452, 3.409327675794633361 ) ) ;
#9065 = CARTESIAN_POINT ( 'NONE',  ( -112.5562042904833788, -23.47596703998600631, 11.44779298504227683 ) ) ;
#9066 = LINE ( 'NONE', #25287, #26138 ) ;
#9067 = ORIENTED_EDGE ( 'NONE', *, *, #26020, .F. ) ;
#9068 = DIRECTION ( 'NONE',  ( -3.773278334453079618E-23, 0.9999999999976377785, 2.173523156925979975E-06 ) ) ;
#9069 = ADVANCED_FACE ( 'NONE', ( #34877 ), #6835, .F. ) ;
#9070 = CARTESIAN_POINT ( 'NONE',  ( -5.912814555383966386, -6.376774720514418959, 20.28973052848695602 ) ) ;
#9071 = CARTESIAN_POINT ( 'NONE',  ( -51.69439593370608321, -25.10935976765677324, 3.842802501644153157 ) ) ;
#9072 = CARTESIAN_POINT ( 'NONE',  ( -1.126084586642228436, -21.63456646517454729, 11.49999999999998934 ) ) ;
#9073 = CARTESIAN_POINT ( 'NONE',  ( -19.80875734969026425, -5.965225279485572685, 31.02402280011862246 ) ) ;
#9074 = CARTESIAN_POINT ( 'NONE',  ( 18.70946937610417038, -5.484834493922766896, -1.500000000000002220 ) ) ;
#9075 = PLANE ( 'NONE',  #86348 ) ;
#9076 = ORIENTED_EDGE ( 'NONE', *, *, #29037, .F. ) ;
#9077 = CARTESIAN_POINT ( 'NONE',  ( 4.102729645046709450, 19.96921287702725323, 11.49999999999999645 ) ) ;
#9078 = DIRECTION ( 'NONE',  ( 0.000000000000000000, -0.9999999999976377785, -2.173523156925979975E-06 ) ) ;
#9079 = APPROVAL ( #11454, 'UNKNOWN' ) ;
#9080 = AXIS2_PLACEMENT_3D ( 'NONE', #83719, #45175, #53284 ) ;
#9081 = CARTESIAN_POINT ( 'NONE',  ( -104.5895376238167245, -23.48783264082478794, -1.443836473390062158 ) ) ;
#9082 = ORIENTED_EDGE ( 'NONE', *, *, #14418, .T. ) ;
#9083 = DIRECTION ( 'NONE',  ( 0.000000000000000000, 0.000000000000000000, 1.000000000000000000 ) ) ;
#9084 = CARTESIAN_POINT ( 'NONE',  ( -29.62287095715006302, -24.43673626876299920, 0.6166258652147375008 ) ) ;
#9085 = CARTESIAN_POINT ( 'NONE',  ( -39.49170631829002787, -25.31628713280249698, 5.433214320636030159 ) ) ;
#9086 = CARTESIAN_POINT ( 'NONE',  ( -40.48563153939314674, -24.52399227489126687, 9.353111116836521077 ) ) ;
#9087 = VECTOR ( 'NONE', #97290, 1000.000000000000000 ) ;
#9088 = LINE ( 'NONE', #92319, #96470 ) ;
#9089 = CARTESIAN_POINT ( 'NONE',  ( 20.09017895974002599, 0.4902201509063087159, 11.49999999999998934 ) ) ;
#9090 = AXIS2_PLACEMENT_3D ( 'NONE', #83299, #13779, #14281 ) ;
#9091 = FACE_OUTER_BOUND ( 'NONE', #6919, .T. ) ;
#9092 = ORIENTED_EDGE ( 'NONE', *, *, #67213, .T. ) ;
#9093 = CARTESIAN_POINT ( 'NONE',  ( -66.58367953917903037, -24.51419770103157347, 9.386484678747176957 ) ) ;
#9094 = AXIS2_PLACEMENT_3D ( 'NONE', #61157, #91083, #76834 ) ;
#9095 = CARTESIAN_POINT ( 'NONE',  ( 2.177599385301639323, -22.86303409451243596, 11.49999999999999645 ) ) ;
#9096 = CARTESIAN_POINT ( 'NONE',  ( 13.97002500213282516, -17.90638934399130733, -1.500000000000002220 ) ) ;
#9097 = ORIENTED_EDGE ( 'NONE', *, *, #35807, .F. ) ;
#9098 = CARTESIAN_POINT ( 'NONE',  ( -30.47287095715006089, -25.28806803508177836, 5.559097854862454113 ) ) ;
#9099 = PLANE ( 'NONE',  #85263 ) ;
#9100 = CARTESIAN_POINT ( 'NONE',  ( -38.54595511171842759, -24.15620529776627379, 10.23563542870660825 ) ) ;
#9101 = CARTESIAN_POINT ( 'NONE',  ( -30.57287095715008007, -24.05861711713197337, -0.4619017001958101165 ) ) ;
#9102 = CARTESIAN_POINT ( 'NONE',  ( -128.5222656221514228, -23.48786465467242124, 11.44779295918253403 ) ) ;
#9103 = CARTESIAN_POINT ( 'NONE',  ( -49.51489430277374026, -25.31544969143762458, 5.069408439402988797 ) ) ;
#9104 = CARTESIAN_POINT ( 'NONE',  ( -61.52287095715006160, -24.64898659630367916, 1.056161002820822592 ) ) ;
#9105 = CARTESIAN_POINT ( 'NONE',  ( -58.65645660196261701, -23.48783264082476663, -1.443836473390093689 ) ) ;
#9106 = VERTEX_POINT ( 'NONE', #26264 ) ;
#9107 = CARTESIAN_POINT ( 'NONE',  ( -14.54385459823299875, 14.27422344363935025, -1.500000000000002220 ) ) ;
#9108 = ORIENTED_EDGE ( 'NONE', *, *, #90095, .T. ) ;
#9109 = EDGE_CURVE ( 'NONE', #13730, #96161, #40995, .T. ) ;
#9110 = CARTESIAN_POINT ( 'NONE',  ( -0.3492834940180428727, 22.98956000712751546, 11.49999999999998934 ) ) ;
#9111 = CARTESIAN_POINT ( 'NONE',  ( -7.264088518202086675, -5.876774720514411854, 19.78976258633487717 ) ) ;
#9112 = ORIENTED_EDGE ( 'NONE', *, *, #12545, .F. ) ;
#9113 = VECTOR ( 'NONE', #31410, 1000.000000000000000 ) ;
#9114 = PLANE ( 'NONE',  #81741 ) ;
#9115 = CARTESIAN_POINT ( 'NONE',  ( -81.62287095715004170, -24.66019654487199020, 8.947790411086131712 ) ) ;
#9116 = CARTESIAN_POINT ( 'NONE',  ( -116.4728709571500360, -25.30558663486635140, 5.000950659935019971 ) ) ;
#9118 = ORIENTED_EDGE ( 'NONE', *, *, #33925, .T. ) ;
#9117 = CARTESIAN_POINT ( 'NONE',  ( -20.14006130340733236, -7.001243683211865410, 11.49999999999999645 ) ) ;
#9119 = EDGE_CURVE ( 'NONE', #36250, #94475, #36589, .T. ) ;
#9120 = ORIENTED_EDGE ( 'NONE', *, *, #20552, .F. ) ;
#9121 = CARTESIAN_POINT ( 'NONE',  ( -13.56020932195406203, -17.60290058955388659, -1.500000000000002220 ) ) ;
#9122 = ADVANCED_FACE ( 'NONE', ( #65854 ), #28687, .T. ) ;
#9123 = CARTESIAN_POINT ( 'NONE',  ( 1.453578435135240321, -20.60874541997745268, -1.500000000000002220 ) ) ;
#9124 = VERTEX_POINT ( 'NONE', #90653 ) ;
#9125 = DIRECTION ( 'NONE',  ( 0.000000000000000000, 0.9999999999976377785, 2.173523156925979128E-06 ) ) ;
#9126 = CARTESIAN_POINT ( 'NONE',  ( -95.58938763694557395, -24.52399227489127398, 9.353111116836521077 ) ) ;
#9127 = EDGE_LOOP ( 'NONE', ( #2825, #46985 ) ) ;
#9128 = CARTESIAN_POINT ( 'NONE',  ( -79.52287095715006160, -23.48786465467241058, 11.44779295918254469 ) ) ;
#9129 = ORIENTED_EDGE ( 'NONE', *, *, #49574, .T. ) ;
#9130 = DIRECTION ( 'NONE',  ( -3.773278334453079618E-23, 0.9999999999976377785, 2.173523156925979975E-06 ) ) ;
#9131 = CARTESIAN_POINT ( 'NONE',  ( 6.973883220674568229, 19.69035807221911938, -1.500000000000002220 ) ) ;
#9132 = ADVANCED_FACE ( 'NONE', ( #97766 ), #43984, .T. ) ;
#9133 = CARTESIAN_POINT ( 'NONE',  ( 4.919149715316761373, 21.27959583485438344, 11.49999999999999645 ) ) ;
#9134 = FACE_OUTER_BOUND ( 'NONE', #36227, .T. ) ;
#9135 = DIRECTION ( 'NONE',  ( 0.000000000000000000, -0.9999999999976377785, -2.173523156925979128E-06 ) ) ;
#9136 = CARTESIAN_POINT ( 'NONE',  ( 16.76845895467136671, -15.01613412638008782, -1.500000000000002220 ) ) ;
#9137 = AXIS2_PLACEMENT_3D ( 'NONE', #94302, #46143, #38521 ) ;
#9138 = CARTESIAN_POINT ( 'NONE',  ( -50.47686723370601669, -25.26334751266341883, 4.734242724451897644 ) ) ;
#9139 = CARTESIAN_POINT ( 'NONE',  ( -108.8968792378192063, -25.15277794460069316, 6.986250878905963191 ) ) ;
#9140 = CARTESIAN_POINT ( 'NONE',  ( 4.261846905714947731, -5.876774720514426953, 21.73176331363731251 ) ) ;
#9141 = EDGE_LOOP ( 'NONE', ( #24212, #4614, #18758, #2939, #15469, #53947, #10299, #73177, #98853, #14794, #41463 ) ) ;
#9142 = VERTEX_POINT ( 'NONE', #20636 ) ;
#9143 = ORIENTED_EDGE ( 'NONE', *, *, #28431, .T. ) ;
#9144 = EDGE_LOOP ( 'NONE', ( #33586, #62177, #85307, #15851 ) ) ;
#9145 = CIRCLE ( 'NONE', #65898, 3.500000000000000000 ) ;
#9146 = CARTESIAN_POINT ( 'NONE',  ( -0.4629837013611828866, -21.40787533109759977, -1.500000000000002220 ) ) ;
#9147 = CARTESIAN_POINT ( 'NONE',  ( -22.37156870845955225, 0.5457896250522937809, 11.49999999999999645 ) ) ;
#9148 = EDGE_LOOP ( 'NONE', ( #82745, #22395, #30961, #9840 ) ) ;
#9149 = CARTESIAN_POINT ( 'NONE',  ( 18.71565868802652588, -9.641079743366450572, 11.49999999999998934 ) ) ;
#9150 = CARTESIAN_POINT ( 'NONE',  ( -30.40154523107553075, -25.30205729935985559, 3.857144010898052588 ) ) ;
#9151 = CARTESIAN_POINT ( 'NONE',  ( 19.59856454566043382, -3.714209461170434157, -1.500000000000002220 ) ) ;
#9152 = CARTESIAN_POINT ( 'NONE',  ( -50.53590823224938333, -24.63419186844610209, 9.035850630976920428 ) ) ;
#9153 = CIRCLE ( 'NONE', #39943, 0.3000000000000016542 ) ;
#9154 = CARTESIAN_POINT ( 'NONE',  ( 2.922108196329484375, -5.876774720514417183, 20.36383711510645256 ) ) ;
#9155 = CARTESIAN_POINT ( 'NONE',  ( -11.61111146657235871, -18.70866699758865792, -1.500000000000002220 ) ) ;
#9156 = CARTESIAN_POINT ( 'NONE',  ( -83.52287095715007581, -23.72747288104470087, -1.053458166803226348 ) ) ;
#9157 = EDGE_LOOP ( 'NONE', ( #69653, #42715, #67109, #46719, #23121 ) ) ;
#9158 = B_SPLINE_CURVE_WITH_KNOTS ( 'NONE', 3,
 ( #85600, #22188, #7980, #14586 ),
 .UNSPECIFIED., .F., .F.,
 ( 4, 4 ),
 ( 0.000000000000000000, 9.999999999998897304E-05 ),
 .UNSPECIFIED. ) ;
#9159 = DIRECTION ( 'NONE',  ( -7.994117400814786717E-16, -0.000000000000000000, 1.000000000000000000 ) ) ;
#9160 = CARTESIAN_POINT ( 'NONE',  ( -9.278253834636469577, -5.876774720514426953, 21.48128695274316158 ) ) ;
#9161 = CARTESIAN_POINT ( 'NONE',  ( 18.76864855846692492, -9.085702381504452418, 11.49999999999999645 ) ) ;
#9162 = AXIS2_PLACEMENT_3D ( 'NONE', #87205, #48158, #47157 ) ;
#9163 = EDGE_CURVE ( 'NONE', #98076, #7900, #68055, .T. ) ;
#9164 = DIRECTION ( 'NONE',  ( 4.625929269271486900E-15, -1.000000000000000000, 0.000000000000000000 ) ) ;
#9165 = DIRECTION ( 'NONE',  ( 0.1489078231574183508, 6.454799914155188842E-16, -0.9888510809027409865 ) ) ;
#9166 = CARTESIAN_POINT ( 'NONE',  ( -38.62287095715005592, -24.51387760970723662, 9.387446482453427166 ) ) ;
#9167 = CARTESIAN_POINT ( 'NONE',  ( -17.77299844720193533, 11.79293508692305537, -1.500000000000002220 ) ) ;
#9168 = CARTESIAN_POINT ( 'NONE',  ( -55.62287095715006302, -23.48786465467240703, 11.44779295918255180 ) ) ;
#9169 = CARTESIAN_POINT ( 'NONE',  ( -51.08434323850904235, -25.22609634996768690, 3.528234306468502446 ) ) ;
#9170 = EDGE_CURVE ( 'NONE', #51347, #45568, #91644, .T. ) ;
#9171 = CARTESIAN_POINT ( 'NONE',  ( -108.8968792378191921, -25.06732983082694943, 7.447789526168955732 ) ) ;
#9172 = PLANE ( 'NONE',  #5445 ) ;
#9173 = CARTESIAN_POINT ( 'NONE',  ( 16.76845895467136671, -15.01613412638008782, -1.500000000000002220 ) ) ;
#9174 = CARTESIAN_POINT ( 'NONE',  ( -89.23534077628075067, -25.23397913219355004, 6.409327625488847602 ) ) ;
#9175 = ORIENTED_EDGE ( 'NONE', *, *, #4848, .T. ) ;
#9176 = CARTESIAN_POINT ( 'NONE',  ( -98.62287095715005592, -23.47593901973091235, -1.443836447539001089 ) ) ;
#9177 = CARTESIAN_POINT ( 'NONE',  ( -31.61027363099887921, -23.73791477778911130, 11.05961554403171299 ) ) ;
#9178 = CARTESIAN_POINT ( 'NONE',  ( -14.15603575923578283, -13.64839490926926580, 11.49999999999999645 ) ) ;
#9179 = CARTESIAN_POINT ( 'NONE',  ( 27.53860345374784657, 1.682774720514426114, -8.321925749325748356 ) ) ;
#9180 = CARTESIAN_POINT ( 'NONE',  ( -119.5228709571501184, -24.33927499327856125, 9.819080762295806508 ) ) ;
#9181 = ORIENTED_EDGE ( 'NONE', *, *, #13025, .T. ) ;
#9182 = CARTESIAN_POINT ( 'NONE',  ( -99.58680609741216472, -24.51314013834316796, 0.6176544820404258340 ) ) ;
#9183 = LINE ( 'NONE', #8695, #77208 ) ;
#9184 = CARTESIAN_POINT ( 'NONE',  ( -124.6251032423319032, -23.96169478059714564, 10.65365249895717170 ) ) ;
#9185 = AXIS2_PLACEMENT_3D ( 'NONE', #41219, #95997, #11751 ) ;
#9186 = FACE_BOUND ( 'NONE', #4044, .T. ) ;
#9187 = CARTESIAN_POINT ( 'NONE',  ( 7.891737972721761807, -18.10977644326358771, 11.49999999999998934 ) ) ;
#9188 = VERTEX_POINT ( 'NONE', #14521 ) ;
#9189 = CIRCLE ( 'NONE', #41669, 252.4458649670781085 ) ;
#9190 = CARTESIAN_POINT ( 'NONE',  ( 19.32837167043147986, -5.866312143582237404, 11.49999999999999645 ) ) ;
#9191 = CARTESIAN_POINT ( 'NONE',  ( 11.40529837384167777, 3.316774720514342967, -28.07356074712937044 ) ) ;
#9192 = EDGE_CURVE ( 'NONE', #5846, #27769, #59612, .T. ) ;
#9193 = VERTEX_POINT ( 'NONE', #5420 ) ;
#9194 = FACE_OUTER_BOUND ( 'NONE', #49472, .T. ) ;
#9195 = CARTESIAN_POINT ( 'NONE',  ( 13.60020833695035947, 1.530808498934190338E-16, -1.249999999999998890 ) ) ;
#9196 = CARTESIAN_POINT ( 'NONE',  ( 21.57151214508649772, 3.625915217019311583E-15, 0.000000000000000000 ) ) ;
#9197 = CARTESIAN_POINT ( 'NONE',  ( 9.749999999999985789, 18.74999999999999645, 0.000000000000000000 ) ) ;
#9198 = DIRECTION ( 'NONE',  ( 0.000000000000000000, -7.805083003223303470E-15, 1.000000000000000000 ) ) ;
#9199 = CARTESIAN_POINT ( 'NONE',  ( -107.5862556121689835, -24.65952944569304606, 1.056160979905704789 ) ) ;
#9200 = CARTESIAN_POINT ( 'NONE',  ( 13.83478396660306942, -14.44641118834825910, -1.500000000000002220 ) ) ;
#9201 = CARTESIAN_POINT ( 'NONE',  ( 3.252401863874210264, 5.965225279485592225, -29.35688408629928858 ) ) ;
#9202 = CARTESIAN_POINT ( 'NONE',  ( -116.5517184843068890, -24.66019654487199730, 8.947790411086115725 ) ) ;
#9203 = ORIENTED_EDGE ( 'NONE', *, *, #35701, .T. ) ;
#9204 = ADVANCED_FACE ( 'NONE', ( #98253 ), #21133, .F. ) ;
#9205 = CARTESIAN_POINT ( 'NONE',  ( -79.63744741913833991, -23.96169478059713143, 10.65365249895718058 ) ) ;
#9206 = DIRECTION ( 'NONE',  ( 0.000000000000000000, -2.173523156925980399E-06, 0.9999999999976378895 ) ) ;
#9207 = CARTESIAN_POINT ( 'NONE',  ( -70.34543693012690824, -25.03284467579916495, 7.563174216508125269 ) ) ;
#9208 = LINE ( 'NONE', #79219, #88920 ) ;
#9209 = CYLINDRICAL_SURFACE ( 'NONE', #4312, 130.7884398600581335 ) ;
#9210 = CARTESIAN_POINT ( 'NONE',  ( -83.58529744386720495, -24.51314013834315020, 0.6176544820404096248 ) ) ;
#9211 = CARTESIAN_POINT ( 'NONE',  ( -49.62287095715005592, -29.50250243563736774, 8.947779886222146928 ) ) ;
#9213 = VECTOR ( 'NONE', #25984, 1000.000000000000000 ) ;
#9212 = CARTESIAN_POINT ( 'NONE',  ( -73.62287095715009855, -24.51283580621364067, 0.6167428607019832532 ) ) ;
#9214 = ORIENTED_EDGE ( 'NONE', *, *, #69830, .F. ) ;
#9215 = AXIS2_PLACEMENT_3D ( 'NONE', #33862, #10020, #3927 ) ;
#9216 = CARTESIAN_POINT ( 'NONE',  ( 17.43904876784772284, 10.37648870149486413, 11.49999999999998934 ) ) ;
#9217 = EDGE_CURVE ( 'NONE', #35380, #56311, #44491, .T. ) ;
#9218 = CARTESIAN_POINT ( 'NONE',  ( 0.7051282051282083962, -6.376774720514427841, 21.75000000000000000 ) ) ;
#9219 = CARTESIAN_POINT ( 'NONE',  ( -34.61897583861063765, -23.48783264082478084, -1.443836473390076591 ) ) ;
#9220 = CARTESIAN_POINT ( 'NONE',  ( -105.6228709571500559, -24.83602698348160942, 1.605859176311272618 ) ) ;
#9221 = ORIENTED_EDGE ( 'NONE', *, *, #46047, .T. ) ;
#9222 = CARTESIAN_POINT ( 'NONE',  ( -50.40445135320379677, -25.12215419635199964, 7.101635560852263218 ) ) ;
#9223 = CARTESIAN_POINT ( 'NONE',  ( 19.91930514195032487, 3.327535025408205893, -1.500000000000002220 ) ) ;
#9224 = CARTESIAN_POINT ( 'NONE',  ( 20.45381123341165619, -5.387677532796200097, 11.49999999999999645 ) ) ;
#9225 = CARTESIAN_POINT ( 'NONE',  ( -4.315754209668272168, 21.71352930684897942, -1.500000000000002220 ) ) ;
#9226 = EDGE_CURVE ( 'NONE', #75580, #79185, #98758, .T. ) ;
#9227 = CARTESIAN_POINT ( 'NONE',  ( -15.41819309731374510, 13.62919173607049927, 11.49999999999998934 ) ) ;
#9228 = CARTESIAN_POINT ( 'NONE',  ( 7.081057417352553784, -5.876774720514423400, 21.11453472826393352 ) ) ;
#9229 = VERTEX_POINT ( 'NONE', #91150 ) ;
#9230 = CARTESIAN_POINT ( 'NONE',  ( -88.62287095715004170, -29.50248528299804818, 1.056150453629040253 ) ) ;
#9231 = ORIENTED_EDGE ( 'NONE', *, *, #22296, .F. ) ;
#9232 = EDGE_CURVE ( 'NONE', #9229, #2928, #22125, .T. ) ;
#9233 = CARTESIAN_POINT ( 'NONE',  ( 5.271800844963591359, -3.316774720514426456, -28.56638892015329034 ) ) ;
#9234 = CARTESIAN_POINT ( 'NONE',  ( -109.5228709571500616, -24.64965694238408034, 8.947790433994192938 ) ) ;
#9235 = ORIENTED_EDGE ( 'NONE', *, *, #90540, .F. ) ;
#9236 = ORIENTED_EDGE ( 'NONE', *, *, #96779, .T. ) ;
#9237 = VERTEX_POINT ( 'NONE', #52598 ) ;
#9238 = CARTESIAN_POINT ( 'NONE',  ( -8.160000000000000142, -9.652339641703484574, -1.621096496867199033 ) ) ;
#9239 = CARTESIAN_POINT ( 'NONE',  ( -127.6228709571500843, -23.96177878511309345, 10.65340807706328974 ) ) ;
#9240 = CARTESIAN_POINT ( 'NONE',  ( 6.259688558337090036, -5.876774720514413630, 19.73360741988579292 ) ) ;
#9241 = CARTESIAN_POINT ( 'NONE',  ( 20.01179378540625819, 5.277757631783551950, -1.500000000000002220 ) ) ;
#9242 = EDGE_CURVE ( 'NONE', #47768, #48919, #83534, .T. ) ;
#9243 = CARTESIAN_POINT ( 'NONE',  ( 18.84366469573077296, 10.75509914293975555, 11.49999999999999645 ) ) ;
#9244 = ORIENTED_EDGE ( 'NONE', *, *, #12994, .T. ) ;
#9245 = CARTESIAN_POINT ( 'NONE',  ( -41.92287095715005307, -23.47596703998600276, 11.44779298504227683 ) ) ;
#9246 = VECTOR ( 'NONE', #66214, 1000.000000000000114 ) ;
#9247 = CARTESIAN_POINT ( 'NONE',  ( -111.0639896554701949, -25.14418962453571638, 3.027308487689960970 ) ) ;
#9248 = CARTESIAN_POINT ( 'NONE',  ( 22.37589550080693712, 1.095942408959037273, -1.500000000000002220 ) ) ;
#9249 = EDGE_CURVE ( 'NONE', #20729, #87025, #19800, .T. ) ;
#9250 = CARTESIAN_POINT ( 'NONE',  ( -79.34796103478946350, -25.27874851471385753, 6.000419794089626002 ) ) ;
#9251 = CARTESIAN_POINT ( 'NONE',  ( -120.6228709571500275, -23.84081130438200802, 10.88220057463248658 ) ) ;
#9252 = ORIENTED_EDGE ( 'NONE', *, *, #13634, .F. ) ;
#9253 = DIRECTION ( 'NONE',  ( -5.551115123125793746E-15, 0.000000000000000000, -1.000000000000000000 ) ) ;
#9254 = CARTESIAN_POINT ( 'NONE',  ( -76.62287095715007013, -24.50321055353805377, 9.387540953477529371 ) ) ;
#9255 = ORIENTED_EDGE ( 'NONE', *, *, #6562, .T. ) ;
#9256 = AXIS2_PLACEMENT_3D ( 'NONE', #59610, #97655, #51992 ) ;
#9257 = ORIENTED_EDGE ( 'NONE', *, *, #89257, .T. ) ;
#9258 = CARTESIAN_POINT ( 'NONE',  ( -110.2228709571500502, -23.47596703998600631, 11.44779298504227860 ) ) ;
#9259 = ORIENTED_EDGE ( 'NONE', *, *, #84505, .F. ) ;
#9260 = DIRECTION ( 'NONE',  ( 0.000000000000000000, -0.9999999999976377785, -2.173523156925979975E-06 ) ) ;
#9261 = CARTESIAN_POINT ( 'NONE',  ( -4.771770383141621608, -20.67029057396967318, -1.500000000000002220 ) ) ;
#9262 = VERTEX_POINT ( 'NONE', #37377 ) ;
#9263 = CARTESIAN_POINT ( 'NONE',  ( -117.5520258364394692, -24.65952944569305316, 1.056160979905706343 ) ) ;
#9264 = CARTESIAN_POINT ( 'NONE',  ( -21.80608713477256089, -0.9339522974687717305, 11.49999999999998934 ) ) ;
#9265 = CARTESIAN_POINT ( 'NONE',  ( -52.52205769399885327, -23.48786465467241058, 11.44779295918255357 ) ) ;
#9266 = PLANE ( 'NONE',  #66395 ) ;
#9267 = CARTESIAN_POINT ( 'NONE',  ( -50.52287095715006160, -23.47593901973090169, -1.443836447538997092 ) ) ;
#9268 = CARTESIAN_POINT ( 'NONE',  ( 1.801620404824296084, -21.73869551012647605, -1.500000000000002220 ) ) ;
#9269 = CARTESIAN_POINT ( 'NONE',  ( -1.222978892338334012, -6.376774720514411854, 19.56655654527324373 ) ) ;
#9270 = ORIENTED_EDGE ( 'NONE', *, *, #13657, .T. ) ;
#9271 = CARTESIAN_POINT ( 'NONE',  ( 10.95759398273795249, -4.132774720514426292, -26.86884997114579932 ) ) ;
#9272 = CARTESIAN_POINT ( 'NONE',  ( -48.95684766248727726, -25.26337410439581177, 6.634936722238220952 ) ) ;
#9273 = ORIENTED_EDGE ( 'NONE', *, *, #28984, .F. ) ;
#9274 = AXIS2_PLACEMENT_3D ( 'NONE', #41006, #87676, #40508 ) ;
#9275 = ORIENTED_EDGE ( 'NONE', *, *, #88865, .T. ) ;
#9276 = ORIENTED_EDGE ( 'NONE', *, *, #36706, .F. ) ;
#9277 = DIRECTION ( 'NONE',  ( 0.1311553622875919756, 0.000000000000000000, 0.9913618264504692190 ) ) ;
#9278 = CARTESIAN_POINT ( 'NONE',  ( -82.60434911312748341, -23.48783264082478084, -1.443836473390069264 ) ) ;
#9279 = CARTESIAN_POINT ( 'NONE',  ( -20.47598858559898716, 5.595549388561865456, -1.500000000000002220 ) ) ;
#9280 = CARTESIAN_POINT ( 'NONE',  ( -94.62287095715009855, -24.34917612406837861, 0.1852690917426660921 ) ) ;
#9281 = CARTESIAN_POINT ( 'NONE',  ( -30.59755354180557418, -24.77158516743337913, 8.907023374642852431 ) ) ;
#9282 = CARTESIAN_POINT ( 'NONE',  ( -28.98875734969026396, 5.965225279485572685, -0.08597719988137648983 ) ) ;
#9283 = VECTOR ( 'NONE', #76229, 1000.000000000000000 ) ;
#9284 = DIRECTION ( 'NONE',  ( -0.9976052577199500115, 0.000000000000000000, -0.06916465693916190594 ) ) ;
#9285 = CARTESIAN_POINT ( 'NONE',  ( 12.26431755764203047, -15.03328313062362298, -1.500000000000002220 ) ) ;
#9286 = ADVANCED_FACE ( 'NONE', ( #68322 ), #60723, .T. ) ;
#9287 = CARTESIAN_POINT ( 'NONE',  ( -45.63257255548561631, -24.73486907724917572, 1.287355809206967017 ) ) ;
#9288 = ORIENTED_EDGE ( 'NONE', *, *, #21399, .F. ) ;
#9289 = CARTESIAN_POINT ( 'NONE',  ( 0.4223197742854877812, 19.52780805513575402, 11.49999999999999645 ) ) ;
#9290 = CARTESIAN_POINT ( 'NONE',  ( -5.563047341353722253, -6.376774720514413630, 20.06599527532950589 ) ) ;
#9291 = CIRCLE ( 'NONE', #91934, 18.35000000000000142 ) ;
#9292 = CARTESIAN_POINT ( 'NONE',  ( -108.6228709571500701, -23.73907113216991860, -1.053371485793227702 ) ) ;
#9293 = VERTEX_POINT ( 'NONE', #15515 ) ;
#9294 = CARTESIAN_POINT ( 'NONE',  ( 4.854822496258163866, -6.376774720514422512, 20.96950945262037891 ) ) ;
#9295 = DIRECTION ( 'NONE',  ( -0.000000000000000000, -1.000000000000000000, -0.000000000000000000 ) ) ;
#9296 = CARTESIAN_POINT ( 'NONE',  ( 22.02124265030973760, -4.776774720514394446, 14.80402280011863425 ) ) ;
#9297 = CARTESIAN_POINT ( 'NONE',  ( -101.3313258111971749, -25.25498697735767095, 3.890283171256392780 ) ) ;
#9298 = CARTESIAN_POINT ( 'NONE',  ( 10.71975780190685690, -16.47196428025586812, -1.500000000000002220 ) ) ;
#9299 = ORIENTED_EDGE ( 'NONE', *, *, #42290, .F. ) ;
#9300 = CARTESIAN_POINT ( 'NONE',  ( 19.98343133220876666, -8.209121646405339590, -1.500000000000002220 ) ) ;
#9301 = DIRECTION ( 'NONE',  ( -0.09824042138329623641, -0.9951627101165078093, -3.504396110891626425E-15 ) ) ;
#9302 = CARTESIAN_POINT ( 'NONE',  ( 22.28998074345494729, -6.091270044117925053, -1.500000000000002220 ) ) ;
#9303 = EDGE_CURVE ( 'NONE', #11321, #46989, #49917, .T. ) ;
#9304 = DATE_AND_TIME ( #86440, #18193 ) ;
#9305 = CARTESIAN_POINT ( 'NONE',  ( -91.62287095715004170, -23.47593901973091235, -1.443836447539002865 ) ) ;
#9306 = FACE_OUTER_BOUND ( 'NONE', #23477, .T. ) ;
#9307 = CARTESIAN_POINT ( 'NONE',  ( -76.52287095715009002, -23.73907113216989728, -1.053371485793248574 ) ) ;
#9308 = CARTESIAN_POINT ( 'NONE',  ( -29.49875734969026198, -0.3587747205144262708, 7.870022800118625206 ) ) ;
#9309 = CARTESIAN_POINT ( 'NONE',  ( -43.62287095715006302, -24.51387760970723662, 9.387446482453421837 ) ) ;
#9310 = EDGE_CURVE ( 'NONE', #61298, #48580, #77408, .T. ) ;
#9311 = CARTESIAN_POINT ( 'NONE',  ( -129.5895790072340219, -24.65952944569305316, 1.056160979905705677 ) ) ;
#9312 = CARTESIAN_POINT ( 'NONE',  ( -114.5554595735986680, -23.96169478059714564, 10.65365249895717170 ) ) ;
#9313 = CARTESIAN_POINT ( 'NONE',  ( 7.348632388941331861, 18.53259892055224611, -1.500000000000002220 ) ) ;
#9315 = ADVANCED_FACE ( 'NONE', ( #70321 ), #47483, .F. ) ;
#9314 = CARTESIAN_POINT ( 'NONE',  ( -75.51430423139920833, -23.85049219812685806, 10.88485053497527488 ) ) ;
#9316 = CARTESIAN_POINT ( 'NONE',  ( 17.59243620335545799, -9.192777620008959261, -1.500000000000002220 ) ) ;
#9317 = ORIENTED_EDGE ( 'NONE', *, *, #84311, .T. ) ;
#9318 = AXIS2_PLACEMENT_3D ( 'NONE', #78392, #10393, #49478 ) ;
#9319 = ADVANCED_FACE ( 'NONE', ( #68822 ), #92641, .F. ) ;
#9320 = CARTESIAN_POINT ( 'NONE',  ( -122.5228709571500616, -24.64965694238408034, 8.947790433994191162 ) ) ;
#9321 = ADVANCED_FACE ( 'NONE', ( #8913 ), #38861, .T. ) ;
#9322 = EDGE_CURVE ( 'NONE', #22334, #3335, #23120, .T. ) ;
#9323 = CARTESIAN_POINT ( 'NONE',  ( -104.6228709571500559, -23.95044443724992078, 10.65354141964649592 ) ) ;
#9324 = LINE ( 'NONE', #24047, #24815 ) ;
#9325 = CARTESIAN_POINT ( 'NONE',  ( 12.91705851660734972, -16.24616318834520001, 11.49999999999999645 ) ) ;
#9326 = VECTOR ( 'NONE', #6571, 1000.000000000000000 ) ;
#9327 = FACE_OUTER_BOUND ( 'NONE', #37322, .T. ) ;
#9328 = CARTESIAN_POINT ( 'NONE',  ( -106.5533786925027329, -24.15543982623907482, -0.2315651400026576268 ) ) ;
#9329 = CARTESIAN_POINT ( 'NONE',  ( -2.506051680461856890, -22.62920675306992280, 11.49999999999999645 ) ) ;
#9330 = ORIENTED_EDGE ( 'NONE', *, *, #5221, .T. ) ;
#9331 = B_SPLINE_SURFACE_WITH_KNOTS ( 'NONE', 3, 3, ( 
 ( #76976, #71392, #69381, #100301 ),
 ( #30818, #61783, #92703, #78477 ),
 ( #1384, #54177, #49061, #42947 ),
 ( #3391, #87102, #33819, #27214 ),
 ( #19585, #64298, #2889, #57670 ),
 ( #79492, #34825, #26710, #80996 ),
 ( #73883, #72394, #79989, #9979 ) ),
 .UNSPECIFIED., .F., .F., .F.,
 ( 4, 3, 4 ),
 ( 4, 4 ),
 ( 0.0004766839783834061822, 0.1029713700210900529, 0.2054660560637966982 ),
 ( 0.8697152379461190463, 0.8711292475148973979 ),
 .UNSPECIFIED. ) ;
#9332 = CARTESIAN_POINT ( 'NONE',  ( 30.45304879119406394, 1.682774720514426114, -10.07140455160086567 ) ) ;
#9333 = CARTESIAN_POINT ( 'NONE',  ( -38.52287095715008292, -24.51283580621460345, 0.6167428607048118794 ) ) ;
#9334 = ORIENTED_EDGE ( 'NONE', *, *, #46057, .F. ) ;
#9335 = CARTESIAN_POINT ( 'NONE',  ( -17.47620107869530770, 10.18187089365592612, 11.49999999999998934 ) ) ;
#9336 = EDGE_CURVE ( 'NONE', #12272, #63916, #77907, .T. ) ;
#9337 = EDGE_CURVE ( 'NONE', #44058, #87201, #76412, .T. ) ;
#9338 = DIRECTION ( 'NONE',  ( 0.000000000000000000, 0.000000000000000000, 1.000000000000000000 ) ) ;
#9339 = DIRECTION ( 'NONE',  ( 0.000000000000000000, 0.000000000000000000, -1.000000000000000000 ) ) ;
#9340 = AXIS2_PLACEMENT_3D ( 'NONE', #54604, #70327, #24141 ) ;
#9341 = ORIENTED_EDGE ( 'NONE', *, *, #13400, .T. ) ;
#9342 = CARTESIAN_POINT ( 'NONE',  ( -127.5228709571500616, -24.65952944569304606, 1.056160979905707675 ) ) ;
#9343 = CARTESIAN_POINT ( 'NONE',  ( -13.60431050971674694, 18.46711184989817411, 11.49999999999998934 ) ) ;
#9344 = CARTESIAN_POINT ( 'NONE',  ( -51.62287095715005592, -24.65952944569304250, 1.056160979905695019 ) ) ;
#9345 = CARTESIAN_POINT ( 'NONE',  ( -0.003041637939312698616, 19.98351707251910980, -1.500000000000002220 ) ) ;
#9346 = CARTESIAN_POINT ( 'NONE',  ( -104.6228709571500985, -23.73907113216990794, -1.053371485793226814 ) ) ;
#9347 = CARTESIAN_POINT ( 'NONE',  ( 8.737904895026865404, 19.08465823478955414, 11.49999999999999645 ) ) ;
#9348 = DIRECTION ( 'NONE',  ( -3.773278334453079030E-23, 0.9999999999976377785, 2.173523156925979128E-06 ) ) ;
#9349 = DIRECTION ( 'NONE',  ( -0.000000000000000000, 0.000000000000000000, -1.000000000000000000 ) ) ;
#9350 = CARTESIAN_POINT ( 'NONE',  ( 1.153593019990587942, -22.03401787307112869, 11.49999999999998934 ) ) ;
#9351 = EDGE_CURVE ( 'NONE', #76612, #35157, #295, .T. ) ;
#9352 = AXIS2_PLACEMENT_3D ( 'NONE', #48328, #40207, #72665 ) ;
#9353 = CARTESIAN_POINT ( 'NONE',  ( -34.52287095715006160, -23.48783264083359867, -1.443836473376372442 ) ) ;
#9354 = EDGE_LOOP ( 'NONE', ( #48961, #55318, #66099, #96426 ) ) ;
#9355 = FACE_OUTER_BOUND ( 'NONE', #45570, .T. ) ;
#9356 = CARTESIAN_POINT ( 'NONE',  ( -49.68454138742491466, -25.27344818403857474, 3.564592451155844000 ) ) ;
#9357 = CARTESIAN_POINT ( 'NONE',  ( 6.547257265821404104, -6.376774720514411854, 19.73960610265399396 ) ) ;
#9358 = ORIENTED_EDGE ( 'NONE', *, *, #22237, .T. ) ;
#9359 = CARTESIAN_POINT ( 'NONE',  ( -47.52287095715006160, -24.64898659630528854, 1.056161002820821038 ) ) ;
#9360 = EDGE_LOOP ( 'NONE', ( #14522, #6287, #5754, #27565 ) ) ;
#9361 = VECTOR ( 'NONE', #56254, 1000.000000000000000 ) ;
#9362 = ORIENTED_EDGE ( 'NONE', *, *, #29834, .F. ) ;
#9363 = LINE ( 'NONE', #71780, #97200 ) ;
#9364 = CARTESIAN_POINT ( 'NONE',  ( -100.8972602205940063, -25.10935818312838919, 2.905315788652750086 ) ) ;
#9365 = FACE_OUTER_BOUND ( 'NONE', #89757, .T. ) ;
#9366 = CARTESIAN_POINT ( 'NONE',  ( -6.383830130275963910, 19.51498944528526991, -1.500000000000002220 ) ) ;
#9367 = EDGE_CURVE ( 'NONE', #82473, #46259, #15019, .T. ) ;
#9368 = ORIENTED_EDGE ( 'NONE', *, *, #49146, .F. ) ;
#9369 = CARTESIAN_POINT ( 'NONE',  ( -61.55620429048339304, -23.47596703998600276, 11.44779298504227505 ) ) ;
#9370 = CARTESIAN_POINT ( 'NONE',  ( -44.49316010094732832, -24.34968618360933590, 0.1864209137778786995 ) ) ;
#9371 = DIRECTION ( 'NONE',  ( -0.000000000000000000, 1.000000000000000000, -0.000000000000000000 ) ) ;
#9372 = CARTESIAN_POINT ( 'NONE',  ( -21.31523168734759466, -6.469442287714795015, 11.49999999999998934 ) ) ;
#9373 = EDGE_CURVE ( 'NONE', #42816, #46766, #85030, .T. ) ;
#9374 = CARTESIAN_POINT ( 'NONE',  ( -0.1255922731526210312, -21.42410932854646433, 10.97511746239722363 ) ) ;
#9375 = LINE ( 'NONE', #40334, #28557 ) ;
#9376 = ORIENTED_EDGE ( 'NONE', *, *, #76019, .T. ) ;
#9377 = EDGE_CURVE ( 'NONE', #90387, #9703, #75409, .T. ) ;
#9378 = LINE ( 'NONE', #771, #85702 ) ;
#9379 = CARTESIAN_POINT ( 'NONE',  ( -124.6228709571500559, -23.47593901973091235, -1.443836447538997536 ) ) ;
#9380 = CARTESIAN_POINT ( 'NONE',  ( 18.58881047053902691, 9.431966241625852732, -1.500000000000002220 ) ) ;
#9381 = EDGE_LOOP ( 'NONE', ( #99577, #98081, #93812, #94130 ) ) ;
#9383 = ORIENTED_EDGE ( 'NONE', *, *, #73823, .F. ) ;
#9382 = CARTESIAN_POINT ( 'NONE',  ( 4.712727796232550226, -3.316774720514426456, -25.55789472434992859 ) ) ;
#9384 = ORIENTED_EDGE ( 'NONE', *, *, #22098, .T. ) ;
#9386 = EDGE_CURVE ( 'NONE', #20637, #89121, #95904, .T. ) ;
#9385 = DIRECTION ( 'NONE',  ( -3.773278334453080206E-23, 0.9999999999976377785, 2.173523156925979975E-06 ) ) ;
#9387 = CARTESIAN_POINT ( 'NONE',  ( 17.94697546605861760, -10.91086909363634838, -1.500000000000002220 ) ) ;
#9388 = VERTEX_POINT ( 'NONE', #54597 ) ;
#9389 = CARTESIAN_POINT ( 'NONE',  ( -36.62287095715005592, -23.47593901973091235, -1.443836447539011525 ) ) ;
#9390 = DIRECTION ( 'NONE',  ( 0.000000000000000000, 0.000000000000000000, 1.000000000000000000 ) ) ;
#9391 = CARTESIAN_POINT ( 'NONE',  ( 7.491841679052118508, -5.356774720514426491, -25.13395656343690021 ) ) ;
#9392 = CARTESIAN_POINT ( 'NONE',  ( 9.150000000000000355, -5.876774720514426953, -15.70000000000000284 ) ) ;
#9393 = CARTESIAN_POINT ( 'NONE',  ( -59.50898190215452388, -23.96119346886879597, -0.6495511937832131322 ) ) ;
#9394 = LINE ( 'NONE', #92256, #85271 ) ;
#9395 = CARTESIAN_POINT ( 'NONE',  ( -57.52287095715003318, -24.34917612406836440, 0.1852690917426539075 ) ) ;
#9397 = ORIENTED_EDGE ( 'NONE', *, *, #84248, .T. ) ;
#9396 = CARTESIAN_POINT ( 'NONE',  ( 19.92104321119709098, 9.795001720801039369, 11.49999999999999645 ) ) ;
#9398 = LINE ( 'NONE', #790, #66460 ) ;
#9399 = CARTESIAN_POINT ( 'NONE',  ( -87.52287095715001897, -24.34917612407029353, 0.1852690917476594312 ) ) ;
#9400 = VERTEX_POINT ( 'NONE', #85532 ) ;
#9401 = CARTESIAN_POINT ( 'NONE',  ( -19.30582015231555104, -11.89196067722419237, 11.49999999999998934 ) ) ;
#9402 = VECTOR ( 'NONE', #96275, 1000.000000000000000 ) ;
#9404 = ORIENTED_EDGE ( 'NONE', *, *, #81843, .T. ) ;
#9403 = CARTESIAN_POINT ( 'NONE',  ( -5.926585084595196840, -6.376774720514415407, 20.19722303762275573 ) ) ;
#9405 = ORIENTED_EDGE ( 'NONE', *, *, #43023, .F. ) ;
#9406 = DIRECTION ( 'NONE',  ( -1.000000000000000000, 0.000000000000000000, 0.000000000000000000 ) ) ;
#9407 = CARTESIAN_POINT ( 'NONE',  ( 18.53703574427524359, 7.882278514257341051, -1.500000000000002220 ) ) ;
#9408 = DIRECTION ( 'NONE',  ( -0.000000000000000000, 1.000000000000000000, -0.000000000000000000 ) ) ;
#9409 = ORIENTED_EDGE ( 'NONE', *, *, #86216, .F. ) ;
#9410 = CARTESIAN_POINT ( 'NONE',  ( -58.58953762381671737, -23.48783264082478439, -1.443836473390069264 ) ) ;
#9411 = CARTESIAN_POINT ( 'NONE',  ( 20.99545381566289137, 7.807860396396394620, -1.500000000000002220 ) ) ;
#9412 = ORIENTED_EDGE ( 'NONE', *, *, #51413, .F. ) ;
#9413 = EDGE_LOOP ( 'NONE', ( #71384, #76610, #1249, #34376 ) ) ;
#9414 = CARTESIAN_POINT ( 'NONE',  ( -112.5870093442895552, -24.66019654487200086, 8.947790411086112172 ) ) ;
#9415 = CARTESIAN_POINT ( 'NONE',  ( -94.59719660544779174, -23.73791477778912196, 11.05961554403170588 ) ) ;
#9416 = FACE_OUTER_BOUND ( 'NONE', #59700, .T. ) ;
#9417 = LINE ( 'NONE', #80440, #14111 ) ;
#9418 = AXIS2_PLACEMENT_3D ( 'NONE', #60248, #74937, #20656 ) ;
#9419 = SHAPE_REPRESENTATION ( 'oval head_am_B18.6.7M - M2.5 x 0.45 x 20 Type I Cross Recessed OHMS --20C', ( #37391 ), #16366 ) ;
#9420 = FACE_BOUND ( 'NONE', #42955, .T. ) ;
#9421 = CARTESIAN_POINT ( 'NONE',  ( -18.58057592369839384, -6.135153870360039896, 11.49999999999998934 ) ) ;
#9422 = CARTESIAN_POINT ( 'NONE',  ( 8.971512145086528278, -9.528487854913501920, 4.500000000000001776 ) ) ;
#9423 = ORIENTED_EDGE ( 'NONE', *, *, #58422, .F. ) ;
#9424 = CARTESIAN_POINT ( 'NONE',  ( 10.13398631766115443, 18.95262098133242290, 11.49999999999998934 ) ) ;
#9425 = DIRECTION ( 'NONE',  ( -0.000000000000000000, -0.000000000000000000, 1.000000000000000000 ) ) ;
#9426 = DIRECTION ( 'NONE',  ( 2.352173255807796549E-16, -0.000000000000000000, -1.000000000000000000 ) ) ;
#9427 = CARTESIAN_POINT ( 'NONE',  ( -123.5228709571500474, -24.51387760970726504, 9.387446482453404073 ) ) ;
#9428 = PLANE ( 'NONE',  #19634 ) ;
#9429 = CARTESIAN_POINT ( 'NONE',  ( 22.67525425759127344, 3.225002893152739247, -1.500000000000002220 ) ) ;
#9430 = AXIS2_PLACEMENT_3D ( 'NONE', #74235, #95208, #71881 ) ;
#9431 = EDGE_CURVE ( 'NONE', #7104, #99233, #94142, .T. ) ;
#9432 = B_SPLINE_CURVE_WITH_KNOTS ( 'NONE', 3,
 ( #43249, #11286, #42266, #28015, #35132, #4682, #35631, #73198, #81298, #87915, #65104, #96519, #96023, #26519, #56979, #27015, #18398, #57982, #11782, #57482 ),
 .UNSPECIFIED., .F., .F.,
 ( 4, 2, 2, 2, 2, 2, 2, 2, 2, 4 ),
 ( 0.01762611779143858845, 0.01933231655155710771, 0.02018541593161636907, 0.02103851531167562697, 0.02274471407179414623, 0.02445091283191266548, 0.02786331035214970400, 0.02871640973220896190, 0.02956950911226821979, 0.03127570787238673905 ),
 .UNSPECIFIED. ) ;
#9433 = PERSON_AND_ORGANIZATION_ROLE ( 'classification_officer' ) ;
#9434 = CARTESIAN_POINT ( 'NONE',  ( -93.62287095715005592, -24.65952944569304606, 1.056160979905701236 ) ) ;
#9435 = CARTESIAN_POINT ( 'NONE',  ( -70.48090377608006918, -25.31151630342660752, 5.317320600521428631 ) ) ;
#9436 = CARTESIAN_POINT ( 'NONE',  ( 9.011679573027636891, 17.89655708981447901, 11.49999999999999645 ) ) ;
#9437 = CARTESIAN_POINT ( 'NONE',  ( -80.30894842687054336, -25.26612373909271625, 4.506569033378546862 ) ) ;
#9438 = DIRECTION ( 'NONE',  ( -0.8788171126619707119, 0.4771587602595986910, 0.000000000000000000 ) ) ;
#9439 = EDGE_CURVE ( 'NONE', #18541, #91718, #54768, .T. ) ;
#9440 = AXIS2_PLACEMENT_3D ( 'NONE', #18326, #65531, #89342 ) ;
#9441 = EDGE_CURVE ( 'NONE', #70995, #86012, #10921, .T. ) ;
#9442 = LINE ( 'NONE', #54137, #53874 ) ;
#9443 = B_SPLINE_CURVE_WITH_KNOTS ( 'NONE', 3,
 ( #7778, #38224, #6775, #100099 ),
 .UNSPECIFIED., .F., .F.,
 ( 4, 4 ),
 ( 0.000000000000000000, 9.999999999997510880E-05 ),
 .UNSPECIFIED. ) ;
#9444 = CARTESIAN_POINT ( 'NONE',  ( -39.52287095715006870, -23.47596703998600631, 11.44779298504229281 ) ) ;
#9445 = CARTESIAN_POINT ( 'NONE',  ( -85.62287095715009855, -24.62226745350437440, 0.9660975649728092973 ) ) ;
#9446 = ADVANCED_FACE ( 'NONE', ( #34265 ), #56108, .T. ) ;
#9447 = CARTESIAN_POINT ( 'NONE',  ( -3.058130702743298901, -21.54894043062209263, -1.500000000000002220 ) ) ;
#9448 = CARTESIAN_POINT ( 'NONE',  ( -90.62287095715002749, -25.00182538069145366, 7.747789668545099317 ) ) ;
#9449 = CARTESIAN_POINT ( 'NONE',  ( 2.289404864003111051, -19.52285375609543294, -1.500000000000002220 ) ) ;
#9450 = EDGE_CURVE ( 'NONE', #56961, #58188, #10413, .T. ) ;
#9451 = CARTESIAN_POINT ( 'NONE',  ( 7.749999999999998224, 24.84999999999999787, 2.100000000000000089 ) ) ;
#9452 = EDGE_CURVE ( 'NONE', #91541, #87632, #31748, .T. ) ;
#9453 = AXIS2_PLACEMENT_3D ( 'NONE', #62134, #17443, #32166 ) ;
#9454 = FACE_OUTER_BOUND ( 'NONE', #57114, .T. ) ;
#9455 = APPROVAL_ROLE ( '' ) ;
#9456 = CARTESIAN_POINT ( 'NONE',  ( -91.63120720951806675, -24.15620529776628445, 10.23563542870660115 ) ) ;
#9457 = DIRECTION ( 'NONE',  ( -0.8368789961609474082, 0.000000000000000000, 0.5473879298857851072 ) ) ;
#9458 = CARTESIAN_POINT ( 'NONE',  ( -10.41206725544052780, -17.73373708237225799, 11.49999999999999645 ) ) ;
#9459 = PLANE ( 'NONE',  #78133 ) ;
#9460 = CARTESIAN_POINT ( 'NONE',  ( -120.5884188931606644, -24.83618233451451118, 1.606449574219542598 ) ) ;
#9461 = CARTESIAN_POINT ( 'NONE',  ( -22.56969522194696509, -0.6267768857631424995, 11.49999999999999645 ) ) ;
#9462 = EDGE_LOOP ( 'NONE', ( #78487, #53291, #72691, #96306 ) ) ;
#9463 = CARTESIAN_POINT ( 'NONE',  ( -70.12829555472771403, -25.25639598314597478, 7.087033306383300868 ) ) ;
#9464 = CARTESIAN_POINT ( 'NONE',  ( -60.62287095715004881, -24.99132157543084531, 2.256160258750667502 ) ) ;
#9465 = CARTESIAN_POINT ( 'NONE',  ( -51.23496102711971645, -25.29265441195226671, 4.254405096667612796 ) ) ;
#9466 = CARTESIAN_POINT ( 'NONE',  ( -100.6814946224345846, -25.31267346029541443, 4.736250531364077254 ) ) ;
#9467 = EDGE_CURVE ( 'NONE', #28216, #88881, #26140, .T. ) ;
#9468 = CARTESIAN_POINT ( 'NONE',  ( -117.6228709571500559, -23.47596703998600631, 11.44779298504227683 ) ) ;
#9469 = DIRECTION ( 'NONE',  ( 0.000000000000000000, 0.000000000000000000, -1.000000000000000000 ) ) ;
#9470 = ORIENTED_EDGE ( 'NONE', *, *, #15639, .T. ) ;
#9471 = EDGE_CURVE ( 'NONE', #55321, #21027, #88726, .T. ) ;
#9472 = CARTESIAN_POINT ( 'NONE',  ( -80.19887417545862718, -25.26749879569623047, 4.982290670770169072 ) ) ;
#9473 = CARTESIAN_POINT ( 'NONE',  ( -0.7673284989158746239, 22.82873350090251918, -1.500000000000002220 ) ) ;
#9474 = CARTESIAN_POINT ( 'NONE',  ( -74.53891675414917017, -24.65952944569304606, 1.056160979905701902 ) ) ;
#9475 = FACE_OUTER_BOUND ( 'NONE', #78929, .T. ) ;
#9476 = CARTESIAN_POINT ( 'NONE',  ( -63.56611925033352151, -23.48786465467241058, 11.44779295918254824 ) ) ;
#9477 = CARTESIAN_POINT ( 'NONE',  ( 12.99221220249228281, -18.32192329980629708, 11.49999999999999645 ) ) ;
#9478 = ORIENTED_EDGE ( 'NONE', *, *, #62782, .T. ) ;
#9479 = B_SPLINE_CURVE_WITH_KNOTS ( 'NONE', 3,
 ( #22361, #70060, #8667, #29991 ),
 .UNSPECIFIED., .F., .F.,
 ( 4, 4 ),
 ( 0.000000000000000000, 0.0001000000000000028644 ),
 .UNSPECIFIED. ) ;
#9480 = CARTESIAN_POINT ( 'NONE',  ( -38.62287095715005592, -23.72773821059535848, 11.05748984161097503 ) ) ;
#9481 = B_SPLINE_CURVE_WITH_KNOTS ( 'NONE', 3,
 ( #52872, #28521, #81818, #59484 ),
 .UNSPECIFIED., .F., .F.,
 ( 4, 4 ),
 ( 0.000000000000000000, 0.0001000000000000028644 ),
 .UNSPECIFIED. ) ;
#9482 = CARTESIAN_POINT ( 'NONE',  ( 11.39931579351042679, 18.75040340349860557, -1.500000000000002220 ) ) ;
#9483 = CARTESIAN_POINT ( 'NONE',  ( -124.6623340026854834, -25.38352273315424057, 4.245316684715575661 ) ) ;
#9484 = CARTESIAN_POINT ( 'NONE',  ( -110.5562042904833788, -25.00158670708909625, 2.256160236439166855 ) ) ;
#9485 = DIRECTION ( 'NONE',  ( 0.000000000000000000, 0.000000000000000000, -1.000000000000000000 ) ) ;
#9486 = ORIENTED_EDGE ( 'NONE', *, *, #4887, .T. ) ;
#9487 = LINE ( 'NONE', #62801, #67070 ) ;
#9488 = CARTESIAN_POINT ( 'NONE',  ( -97.52287095715007581, -23.47593901973090524, -1.443836447538996648 ) ) ;
#9489 = VERTEX_POINT ( 'NONE', #33759 ) ;
#9490 = CARTESIAN_POINT ( 'NONE',  ( -19.64171699416042571, -5.764624264842452384, -1.500000000000002220 ) ) ;
#9491 = ORIENTED_EDGE ( 'NONE', *, *, #12082, .F. ) ;
#9492 = EDGE_LOOP ( 'NONE', ( #30468, #28625, #63559, #55292 ) ) ;
#9493 = ORIENTED_EDGE ( 'NONE', *, *, #82578, .F. ) ;
#9494 = ORIENTED_EDGE ( 'NONE', *, *, #50856, .T. ) ;
#9495 = CARTESIAN_POINT ( 'NONE',  ( -8.701767255460435280, 21.38705905713849020, 11.49999999999998934 ) ) ;
#9496 = DIRECTION ( 'NONE',  ( -0.000000000000000000, 2.173523156925979552E-06, -0.9999999999976378895 ) ) ;
#9497 = CARTESIAN_POINT ( 'NONE',  ( 6.837353022973060135, 19.10023500134885310, -1.500000000000002220 ) ) ;
#9498 = ORIENTED_EDGE ( 'NONE', *, *, #4434, .T. ) ;
#9499 = CARTESIAN_POINT ( 'NONE',  ( 29.70435979725210274, 3.845442984095253536, 28.14021868772163160 ) ) ;
#9500 = AXIS2_PLACEMENT_3D ( 'NONE', #91929, #7186, #91421 ) ;
#9501 = DIRECTION ( 'NONE',  ( -0.000000000000000000, 1.000000000000000000, -0.000000000000000000 ) ) ;
#9502 = EDGE_CURVE ( 'NONE', #5789, #42735, #18026, .T. ) ;
#9503 = CARTESIAN_POINT ( 'NONE',  ( 1.140932434931746582E-13, -5.876774720514426953, 21.78128695274321203 ) ) ;
#9504 = CARTESIAN_POINT ( 'NONE',  ( 4.328803674008796065, -6.376774720514406525, 18.75671216747623049 ) ) ;
#9506 = ORIENTED_EDGE ( 'NONE', *, *, #54633, .T. ) ;
#9505 = CARTESIAN_POINT ( 'NONE',  ( -0.7226137440361984909, -21.50112622129444162, 11.49999999999999645 ) ) ;
#9507 = CARTESIAN_POINT ( 'NONE',  ( -89.55620429048337883, -24.64965694238574656, 8.947790433994201820 ) ) ;
#9508 = CARTESIAN_POINT ( 'NONE',  ( -112.5228709571500616, -24.64898659630529210, 1.056161002820831474 ) ) ;
#9509 = ORIENTED_EDGE ( 'NONE', *, *, #48468, .T. ) ;
#9510 = CARTESIAN_POINT ( 'NONE',  ( -11.67826063220891086, 17.12864047899337550, 11.49999999999998934 ) ) ;
#9511 = EDGE_CURVE ( 'NONE', #2616, #76877, #10104, .T. ) ;
#9512 = ORIENTED_EDGE ( 'NONE', *, *, #31678, .F. ) ;
#9514 = ORIENTED_EDGE ( 'NONE', *, *, #75882, .T. ) ;
#9513 = CARTESIAN_POINT ( 'NONE',  ( -125.6236348478159073, -24.92564183028979485, 1.928384488918254425 ) ) ;
#9515 = CARTESIAN_POINT ( 'NONE',  ( -111.6245959756683561, -24.51419770103157703, 9.386484678747162747 ) ) ;
#9516 = CARTESIAN_POINT ( 'NONE',  ( -53.52287095715006870, -24.65952944569304606, 1.056160979905693686 ) ) ;
#9517 = VERTEX_POINT ( 'NONE', #71827 ) ;
#9518 = ORIENTED_EDGE ( 'NONE', *, *, #43400, .T. ) ;
#9519 = CARTESIAN_POINT ( 'NONE',  ( -109.5895376238167245, -23.47596703998600631, 11.44779298504227683 ) ) ;
#9520 = AXIS2_PLACEMENT_3D ( 'NONE', #24060, #7841, #1245 ) ;
#9521 = CARTESIAN_POINT ( 'NONE',  ( -42.65525658569841028, -23.73791477778911485, 11.05961554403171299 ) ) ;
#9522 = CARTESIAN_POINT ( 'NONE',  ( -29.72012931874203900, -25.17545358843327108, 3.652302162786316142 ) ) ;
#9524 = EDGE_LOOP ( 'NONE', ( #9397, #15137 ) ) ;
#9523 = CARTESIAN_POINT ( 'NONE',  ( 8.687672273659204691, 20.25853876245846408, 11.49999999999999645 ) ) ;
#9525 = CARTESIAN_POINT ( 'NONE',  ( -48.93017815765824707, -25.21617556241885438, 6.556673522205215932 ) ) ;
#9526 = CARTESIAN_POINT ( 'NONE',  ( 10.27952223434480494, 20.12118371629609470, 11.49999999999998934 ) ) ;
#9527 = B_SPLINE_CURVE_WITH_KNOTS ( 'NONE', 3,
 ( #8854, #21202, #44557, #1257, #32186, #98828 ),
 .UNSPECIFIED., .F., .F.,
 ( 4, 2, 4 ),
 ( 0.000000000000000000, 0.001380901958385387894, 0.002761803916770775788 ),
 .UNSPECIFIED. ) ;
#9528 = CARTESIAN_POINT ( 'NONE',  ( 18.89479412359299815, 9.153864009170110450, -1.500000000000002220 ) ) ;
#9530 = ORIENTED_EDGE ( 'NONE', *, *, #73942, .F. ) ;
#9529 = FACE_OUTER_BOUND ( 'NONE', #62430, .T. ) ;
#9531 = B_SPLINE_CURVE_WITH_KNOTS ( 'NONE', 3,
 ( #41447, #85737, #2899, #72405 ),
 .UNSPECIFIED., .F., .F.,
 ( 4, 4 ),
 ( 0.6109362546251637660, 0.6199426858972792997 ),
 .UNSPECIFIED. ) ;
#9532 = ORIENTED_EDGE ( 'NONE', *, *, #95831, .F. ) ;
#9533 = DIRECTION ( 'NONE',  ( 0.000000000000000000, 0.08084198211964954695, -0.9967269304714136968 ) ) ;
#9534 = CARTESIAN_POINT ( 'NONE',  ( 9.045332206306587963, -0.8999999999999999112, -3.697389739420775090 ) ) ;
#9535 = ORIENTED_EDGE ( 'NONE', *, *, #17582, .T. ) ;
#9536 = CARTESIAN_POINT ( 'NONE',  ( 10.98566517548414012, -18.08203305749968592, -1.500000000000002220 ) ) ;
#9537 = DIRECTION ( 'NONE',  ( 1.000000000000000000, 3.773278334444166432E-23, 8.201307841325785021E-29 ) ) ;
#9538 = CARTESIAN_POINT ( 'NONE',  ( -59.79220569025929422, -25.27183489919805126, 3.712349809207164952 ) ) ;
#9539 = CARTESIAN_POINT ( 'NONE',  ( -75.62287095715005592, -23.47593901973091235, -1.443836447539004642 ) ) ;
#9540 = CARTESIAN_POINT ( 'NONE',  ( -32.55620429048339304, -23.47596703998600276, 11.44779298504227505 ) ) ;
#9541 = CARTESIAN_POINT ( 'NONE',  ( -7.641025641025638748, -5.876774720514426953, 21.75000000000001066 ) ) ;
#9542 = CARTESIAN_POINT ( 'NONE',  ( 22.20168578472828358, 1.497490109320031682, -1.500000000000002220 ) ) ;
#9543 = CARTESIAN_POINT ( 'NONE',  ( -49.72218425784361528, -25.03220880655923608, 7.443037874571290402 ) ) ;
#9544 = ORIENTED_EDGE ( 'NONE', *, *, #58941, .F. ) ;
#9545 = CARTESIAN_POINT ( 'NONE',  ( 15.58962545129234911, -1.684774720514426560, -26.91365498785467025 ) ) ;
#9546 = CARTESIAN_POINT ( 'NONE',  ( -37.49079198358890608, -24.34968618360933590, 0.1864209137778856384 ) ) ;
#9547 = DIRECTION ( 'NONE',  ( 0.000000000000000000, 0.000000000000000000, -1.000000000000000000 ) ) ;
#9548 = CARTESIAN_POINT ( 'NONE',  ( -100.5484642610753951, -24.63355581998385091, 0.9682620441943978751 ) ) ;
#9549 = CARTESIAN_POINT ( 'NONE',  ( 11.92939068485097209, -2.682774720514424782, -27.07380692790804488 ) ) ;
#9550 = CARTESIAN_POINT ( 'NONE',  ( 6.171429453590791425, 18.48145409631445446, -1.500000000000002220 ) ) ;
#9551 = CARTESIAN_POINT ( 'NONE',  ( 21.20698605602738951, -2.876969938318672870, -1.500000000000002220 ) ) ;
#9552 = LINE ( 'NONE', #17667, #22313 ) ;
#9553 = CARTESIAN_POINT ( 'NONE',  ( -60.48076987232976620, -25.00182538069856619, 7.747789668514392325 ) ) ;
#9554 = CARTESIAN_POINT ( 'NONE',  ( -100.6228709571500559, -25.00182538069145721, 7.747789668545099317 ) ) ;
#9555 = CARTESIAN_POINT ( 'NONE',  ( -100.8624150394625616, -25.18440029588451168, 3.378658976843279760 ) ) ;
#9556 = CARTESIAN_POINT ( 'NONE',  ( -17.51746294255814718, -14.55262482891283504, -1.500000000000002220 ) ) ;
#9557 = EDGE_CURVE ( 'NONE', #59937, #32327, #57609, .T. ) ;
#9558 = CARTESIAN_POINT ( 'NONE',  ( -102.5888672789946980, -24.34968618360934656, 0.1864209137778959358 ) ) ;
#9559 = CARTESIAN_POINT ( 'NONE',  ( -98.62287095715005592, -23.96127896941632685, -0.6493128931037821516 ) ) ;
#9560 = CARTESIAN_POINT ( 'NONE',  ( 16.83370257367741019, -10.51912618480096206, 11.49999999999999645 ) ) ;
#9561 = CARTESIAN_POINT ( 'NONE',  ( 6.329711958793041049, -6.376774720514411854, 19.73172534246499765 ) ) ;
#9562 = AXIS2_PLACEMENT_3D ( 'NONE', #14078, #36427, #12084 ) ;
#9563 = EDGE_CURVE ( 'NONE', #19646, #908, #91042, .T. ) ;
#9564 = AXIS2_PLACEMENT_3D ( 'NONE', #33695, #16448, #8847 ) ;
#9565 = FACE_OUTER_BOUND ( 'NONE', #93133, .T. ) ;
#9566 = CARTESIAN_POINT ( 'NONE',  ( -65.52287095715006160, -23.47593901973090169, -1.443836447538996870 ) ) ;
#9567 = ORIENTED_EDGE ( 'NONE', *, *, #87451, .T. ) ;
#9568 = CARTESIAN_POINT ( 'NONE',  ( -49.86628797114703815, -25.13894531369371421, 7.008864803050190773 ) ) ;
#9569 = CARTESIAN_POINT ( 'NONE',  ( -5.941268476065055815, -5.876774720514417183, 20.11414146978959749 ) ) ;
#9570 = EDGE_CURVE ( 'NONE', #28435, #4160, #26895, .T. ) ;
#9571 = CARTESIAN_POINT ( 'NONE',  ( -50.89113880358890185, -25.27412246153383890, 2.917241017069057030 ) ) ;
#9572 = CARTESIAN_POINT ( 'NONE',  ( -21.36891742734480104, 3.643610035731704055, 11.49999999999998934 ) ) ;
#9573 = CARTESIAN_POINT ( 'NONE',  ( -56.55997175465316218, -23.73791477778911840, 11.05961554403170766 ) ) ;
#9574 = AXIS2_PLACEMENT_3D ( 'NONE', #41285, #18444, #16940 ) ;
#9575 = CARTESIAN_POINT ( 'NONE',  ( -15.31790942089943286, 12.02624123284522106, -1.500000000000002220 ) ) ;
#9576 = EDGE_CURVE ( 'NONE', #64433, #72799, #56023, .T. ) ;
#9577 = FACE_OUTER_BOUND ( 'NONE', #14020, .T. ) ;
#9578 = VERTEX_POINT ( 'NONE', #56614 ) ;
#9579 = EDGE_CURVE ( 'NONE', #5085, #46960, #85120, .T. ) ;
#9580 = VECTOR ( 'NONE', #39287, 1000.000000000000227 ) ;
#9581 = CARTESIAN_POINT ( 'NONE',  ( 3.609400094169940676, -20.08663944828865766, 11.49999999999999645 ) ) ;
#9582 = LINE ( 'NONE', #78572, #86126 ) ;
#9583 = EDGE_CURVE ( 'NONE', #51818, #76194, #82913, .T. ) ;
#9584 = B_SPLINE_CURVE_WITH_KNOTS ( 'NONE', 3,
 ( #71124, #86834, #17325, #100035 ),
 .UNSPECIFIED., .F., .F.,
 ( 4, 4 ),
 ( 0.000000000000000000, 9.999999999998897304E-05 ),
 .UNSPECIFIED. ) ;
#9585 = DIRECTION ( 'NONE',  ( 0.000000000000000000, -1.000000000000000000, 0.000000000000000000 ) ) ;
#9586 = EDGE_LOOP ( 'NONE', ( #96272, #41667, #6138, #19931, #15471, #29350 ) ) ;
#9587 = CARTESIAN_POINT ( 'NONE',  ( -80.09320475646708815, -25.04201173125214908, 7.520314828238249483 ) ) ;
#9588 = CARTESIAN_POINT ( 'NONE',  ( 33.63416148851499088, 3.931067265920685561, -11.97433369283768734 ) ) ;
#9589 = CARTESIAN_POINT ( 'NONE',  ( -39.36780865613509661, -25.27985487685322141, 5.233841631192319710 ) ) ;
#9590 = VECTOR ( 'NONE', #66909, 1000.000000000000000 ) ;
#9591 = CARTESIAN_POINT ( 'NONE',  ( -49.32129151558435609, -25.31439425002071530, 5.877610906657145584 ) ) ;
#9592 = DIRECTION ( 'NONE',  ( 0.000000000000000000, 0.000000000000000000, -1.000000000000000000 ) ) ;
#9593 = CARTESIAN_POINT ( 'NONE',  ( 18.22116949570664701, -8.484823103377051368, -1.500000000000002220 ) ) ;
#9594 = CARTESIAN_POINT ( 'NONE',  ( 0.000000000000000000, 6.099999999999999645, 0.000000000000000000 ) ) ;
#9595 = ORIENTED_EDGE ( 'NONE', *, *, #80933, .T. ) ;
#9596 = LINE ( 'NONE', #33428, #7419 ) ;
#9597 = CARTESIAN_POINT ( 'NONE',  ( -13.60431050971674694, 18.46711184989817411, 11.49999999999999645 ) ) ;
#9598 = CARTESIAN_POINT ( 'NONE',  ( 18.51665531608540860, 13.21585733361752801, -1.500000000000002220 ) ) ;
#9599 = VERTEX_POINT ( 'NONE', #35763 ) ;
#9600 = CARTESIAN_POINT ( 'NONE',  ( -30.47287095715005734, -25.21920238677788362, 6.407047544386642812 ) ) ;
#9601 = CARTESIAN_POINT ( 'NONE',  ( -98.52287095715006160, -24.65952944569304606, 1.056160979905702346 ) ) ;
#9602 = CARTESIAN_POINT ( 'NONE',  ( -81.52287095715006160, -24.64965694238408034, 8.947790433994198267 ) ) ;
#9603 = CARTESIAN_POINT ( 'NONE',  ( -30.57287095715006942, -23.48213395187224606, 11.44779283644488999 ) ) ;
#9604 = CARTESIAN_POINT ( 'NONE',  ( -69.51084105356602549, -23.96169478059712787, 10.65365249895718414 ) ) ;
#9605 = AXIS2_PLACEMENT_3D ( 'NONE', #44775, #37650, #98038 ) ;
#9606 = CARTESIAN_POINT ( 'NONE',  ( -27.68651082257923335, -24.77145582263907286, 2.274903367125437281 ) ) ;
#9607 = DIRECTION ( 'NONE',  ( 0.000000000000000000, 0.000000000000000000, -1.000000000000000000 ) ) ;
#9608 = CARTESIAN_POINT ( 'NONE',  ( -99.04404089887771079, -25.25460591887426531, 5.494369256536408841 ) ) ;
#9609 = ORIENTED_EDGE ( 'NONE', *, *, #99966, .T. ) ;
#9610 = CARTESIAN_POINT ( 'NONE',  ( 20.11976772532220181, -3.360927329567881205, 11.49999999999998934 ) ) ;
#9611 = EDGE_LOOP ( 'NONE', ( #52192, #66396, #80001, #91808, #67147, #71073, #85023, #2644 ) ) ;
#9612 = ORIENTED_EDGE ( 'NONE', *, *, #83269, .T. ) ;
#9613 = CARTESIAN_POINT ( 'NONE',  ( -6.685540227124203483, -22.02754839873749404, -1.500000000000002220 ) ) ;
#9614 = CARTESIAN_POINT ( 'NONE',  ( -7.326923076923076650, -5.876774720514418071, 20.36318108974359831 ) ) ;
#9615 = ORIENTED_EDGE ( 'NONE', *, *, #63852, .F. ) ;
#9616 = PLANE ( 'NONE',  #44454 ) ;
#9617 = FACE_OUTER_BOUND ( 'NONE', #68677, .T. ) ;
#9618 = B_SPLINE_CURVE_WITH_KNOTS ( 'NONE', 3,
 ( #66870, #58744, #59247, #3473, #49647, #20169, #82078, #12562, #43526, #74463, #90188, #13052, #7438, #59753, #29785, #98282, #30785, #6945, #44013, #60751, #36401, #100266 ),
 .UNSPECIFIED., .F., .F.,
 ( 4, 2, 2, 2, 2, 2, 2, 2, 2, 2, 4 ),
 ( 8.673617379884035472E-19, 0.0005541007949657107429, 0.001108201589931420619, 0.001662302384897130711, 0.002216403179862840370, 0.002770503974828550462, 0.003047554372311408761, 0.003324604769794267060, 0.003878705564759983224, 0.004155755962242840655, 0.004432806359725698954 ),
 .UNSPECIFIED. ) ;
#9619 = CARTESIAN_POINT ( 'NONE',  ( -95.63923414667179657, -23.85016227208581086, -0.8807180028928282001 ) ) ;
#9620 = CARTESIAN_POINT ( 'NONE',  ( -119.4728709571500360, -25.30558663486607429, 5.000950657679038791 ) ) ;
#9622 = ORIENTED_EDGE ( 'NONE', *, *, #94115, .F. ) ;
#9621 = CARTESIAN_POINT ( 'NONE',  ( -6.196366259867160942, 20.41550611124569059, 11.49999999999999645 ) ) ;
#9623 = ORIENTED_EDGE ( 'NONE', *, *, #76817, .F. ) ;
#9624 = CARTESIAN_POINT ( 'NONE',  ( -21.66996937300057269, -4.939502015459471096, 11.49999999999998934 ) ) ;
#9625 = CARTESIAN_POINT ( 'NONE',  ( 17.37421522561336928, 11.14841987994331696, 11.49999999999998934 ) ) ;
#9626 = EDGE_CURVE ( 'NONE', #44485, #16795, #70566, .T. ) ;
#9627 = ORIENTED_EDGE ( 'NONE', *, *, #29992, .F. ) ;
#9628 = CARTESIAN_POINT ( 'NONE',  ( -5.970505764849975527, -5.876774720514411854, 19.55848054040323802 ) ) ;
#9629 = ADVANCED_FACE ( 'NONE', ( #81435 ), #90044, .T. ) ;
#9630 = CARTESIAN_POINT ( 'NONE',  ( -95.51302621525215386, -24.15602025860896163, 10.28564288303535967 ) ) ;
#9631 = ORIENTED_EDGE ( 'NONE', *, *, #43474, .T. ) ;
#9632 = CARTESIAN_POINT ( 'NONE',  ( -124.5228709571500616, -29.50250786944525672, 11.44777988621622811 ) ) ;
#9633 = VECTOR ( 'NONE', #33185, 1000.000000000000000 ) ;
#9634 = ORIENTED_EDGE ( 'NONE', *, *, #27935, .F. ) ;
#9635 = LINE ( 'NONE', #47205, #99794 ) ;
#9636 = B_SPLINE_CURVE_WITH_KNOTS ( 'NONE', 3,
 ( #25485, #10263, #2667, #33602, #64586, #95500, #74652, #58946, #26992, #57959, #72673, #11263, #50335, #82270, #3172, #49849 ),
 .UNSPECIFIED., .F., .F.,
 ( 4, 2, 2, 2, 2, 2, 2, 4 ),
 ( 0.000000000000000000, 0.0004662014769087530121, 0.0009324029538175060243, 0.001398604430726259036, 0.001864805907635012049, 0.002331007384543765278, 0.002797208861452518073, 0.003729611815270027567 ),
 .UNSPECIFIED. ) ;
#9637 =( NAMED_UNIT ( * ) PLANE_ANGLE_UNIT ( ) SI_UNIT ( $, .RADIAN. ) );
#9638 = CARTESIAN_POINT ( 'NONE',  ( -13.77211689728001964, -15.67653869864640903, -1.500000000000002220 ) ) ;
#9639 = CARTESIAN_POINT ( 'NONE',  ( -19.95566455537076678, 8.849265345510103131, 11.49999999999999645 ) ) ;
#9640 = CARTESIAN_POINT ( 'NONE',  ( 25.12780715347580696, -4.914991111971125370, -10.18391567818362731 ) ) ;
#9641 = CARTESIAN_POINT ( 'NONE',  ( -37.62287095715005592, -23.48783264082477373, -1.443836473390072372 ) ) ;
#9642 = CARTESIAN_POINT ( 'NONE',  ( 20.54305097139451064, 9.177977666691313985, -1.500000000000002220 ) ) ;
#9643 = AXIS2_PLACEMENT_3D ( 'NONE', #9645, #64967, #64469 ) ;
#9644 = DIRECTION ( 'NONE',  ( 0.000000000000000000, 0.9999999999976377785, 2.173523156925979975E-06 ) ) ;
#9645 = CARTESIAN_POINT ( 'NONE',  ( 0.7603455638109648529, 10.87344814783205038, 0.000000000000000000 ) ) ;
#9646 = CARTESIAN_POINT ( 'NONE',  ( -54.55620429048340014, -24.65952944569304606, 1.056160979905694131 ) ) ;
#9647 = ORIENTED_EDGE ( 'NONE', *, *, #759, .F. ) ;
#9648 = AXIS2_PLACEMENT_3D ( 'NONE', #5112, #97944, #36062 ) ;
#9649 = EDGE_LOOP ( 'NONE', ( #87308, #38312, #51319, #81010 ) ) ;
#9650 = AXIS2_PLACEMENT_3D ( 'NONE', #17842, #71631, #87339 ) ;
#9651 = ORIENTED_EDGE ( 'NONE', *, *, #13084, .F. ) ;
#9652 = CARTESIAN_POINT ( 'NONE',  ( -100.3181550757389147, -25.26221317742673378, 7.099294928845378827 ) ) ;
#9653 = EDGE_CURVE ( 'NONE', #88472, #43961, #68205, .T. ) ;
#9654 = ORIENTED_EDGE ( 'NONE', *, *, #45916, .T. ) ;
#9655 = VECTOR ( 'NONE', #85898, 1000.000000000000114 ) ;
#9656 = CARTESIAN_POINT ( 'NONE',  ( 21.39645853268639186, 0.3907444525687319703, -1.500000000000002220 ) ) ;
#9657 = CARTESIAN_POINT ( 'NONE',  ( 20.23429811176546167, 9.490607074118958764, 11.49999999999999645 ) ) ;
#9658 = ORIENTED_EDGE ( 'NONE', *, *, #17709, .F. ) ;
#9659 = DIRECTION ( 'NONE',  ( 0.000000000000000000, -1.000000000000000000, 0.000000000000000000 ) ) ;
#9660 = CARTESIAN_POINT ( 'NONE',  ( 20.41947327098772647, -5.118016103960565388, -1.500000000000002220 ) ) ;
#9661 = CARTESIAN_POINT ( 'NONE',  ( -30.44997090143552043, -24.04449549154637111, 10.47557002954947336 ) ) ;
#9662 = CARTESIAN_POINT ( 'NONE',  ( 1.593314845114734535, -19.89410510517485164, -1.500000000000002220 ) ) ;
#9663 = APPLICATION_CONTEXT ( 'configuration controlled 3d designs of mechanical parts and assemblies' ) ;
#9664 =( BOUNDED_SURFACE ( )  B_SPLINE_SURFACE ( 3, 2, ( 
 ( #85447, #94566, #25050 ),
 ( #26570, #49418, #58028 ),
 ( #81349, #12318, #95570 ),
 ( #10335, #4227, #97068 ),
 ( #96563, #88967, #48911 ),
 ( #19935, #35676, #19440 ),
 ( #2738, #43295, #3737 ),
 ( #35180, #74231, #59021 ),
 ( #50405, #42802, #50904 ),
 ( #72748, #11827, #73731 ),
 ( #27570, #89462, #96075 ),
 ( #66151, #65651, #3246 ),
 ( #27064, #4726, #81846 ),
 ( #49920, #72246, #58521 ),
 ( #89953, #66651, #73243 ),
 ( #57530, #97565, #57029 ),
 ( #28064, #80344, #88465 ),
 ( #18940, #79837, #34678 ) ),
 .UNSPECIFIED., .F., .F., .T. ) 
 B_SPLINE_SURFACE_WITH_KNOTS ( ( 4, 2, 2, 2, 2, 2, 2, 2, 4 ),
 ( 3, 3 ),
 ( -3.428680950268159222E-15, 0.002319258964652063781, 0.003478888446979810228, 0.004058703188143683235, 0.004638517929307556242, 0.005798147411635302256, 0.006377962152799175263, 0.006957776893963049138, 0.009277035858618542033 ),
 ( 0.000000000000000000, 1.000000000000000000 ),
 .UNSPECIFIED. ) 
 GEOMETRIC_REPRESENTATION_ITEM ( )  RATIONAL_B_SPLINE_SURFACE ( (
 ( 1.000000000000000000, 0.7071067811865475727, 1.000000000000000000),
 ( 1.000000000000000000, 0.7071067811865475727, 1.000000000000000000),
 ( 1.000000000000000000, 0.7071067811865471286, 1.000000000000000000),
 ( 1.000000000000000000, 0.7071067811865471286, 1.000000000000000000),
 ( 1.000000000000000000, 0.7071067811865473507, 1.000000000000000000),
 ( 1.000000000000000000, 0.7071067811865473507, 1.000000000000000000),
 ( 1.000000000000000000, 0.7071067811865475727, 1.000000000000000000),
 ( 1.000000000000000000, 0.7071067811865475727, 1.000000000000000000),
 ( 1.000000000000000000, 0.7071067811865476838, 1.000000000000000000),
 ( 1.000000000000000000, 0.7071067811865476838, 1.000000000000000000),
 ( 1.000000000000000000, 0.7071067811865473507, 1.000000000000000000),
 ( 1.000000000000000000, 0.7071067811865473507, 1.000000000000000000),
 ( 1.000000000000000000, 0.7071067811865471286, 1.000000000000000000),
 ( 1.000000000000000000, 0.7071067811865471286, 1.000000000000000000),
 ( 1.000000000000000000, 0.7071067811865471286, 1.000000000000000000),
 ( 1.000000000000000000, 0.7071067811865471286, 1.000000000000000000),
 ( 1.000000000000000000, 0.7071067811865475727, 1.000000000000000000),
 ( 1.000000000000000000, 0.7071067811865475727, 1.000000000000000000) ) ) 
 REPRESENTATION_ITEM ( '' )  SURFACE ( )  );
#9665 = CARTESIAN_POINT ( 'NONE',  ( -114.5562042904833930, -23.48786465467241769, 11.44779295918253936 ) ) ;
#9666 = CARTESIAN_POINT ( 'NONE',  ( -64.62287095715005592, -24.65952944569304250, 1.056160979905695685 ) ) ;
#9667 = CARTESIAN_POINT ( 'NONE',  ( -15.57331531552114612, -15.56871402003811333, -1.500000000000002220 ) ) ;
#9668 = ORIENTED_EDGE ( 'NONE', *, *, #12309, .T. ) ;
#9669 = CARTESIAN_POINT ( 'NONE',  ( -65.49580353523785448, -24.52399227489126687, 9.353111116836529959 ) ) ;
#9670 = CARTESIAN_POINT ( 'NONE',  ( -64.62287095715005592, -29.50250243563736774, 8.947779886222145151 ) ) ;
#9671 = CARTESIAN_POINT ( 'NONE',  ( -19.30504728598367237, -7.930543132070424051, 11.49999999999999645 ) ) ;
#9672 = CARTESIAN_POINT ( 'NONE',  ( 31.63443928675788186, -3.712996582965905290, 27.28441363938236464 ) ) ;
#9673 = CARTESIAN_POINT ( 'NONE',  ( -125.5228709571500616, -24.82576562948885623, 8.398263436605594379 ) ) ;
#9674 = CARTESIAN_POINT ( 'NONE',  ( 282.9764569301858046, 5.965225279485572685, 20.79159422840526616 ) ) ;
#9675 = CARTESIAN_POINT ( 'NONE',  ( -19.36244235409943926, 8.944087295975924334, -1.500000000000002220 ) ) ;
#9676 = DIRECTION ( 'NONE',  ( 3.773278334444167608E-23, -1.000000000000000000, 0.000000000000000000 ) ) ;
#9677 = CARTESIAN_POINT ( 'NONE',  ( 8.971512145086531831, -9.528487854913505473, -6.499999999999998224 ) ) ;
#9678 = CARTESIAN_POINT ( 'NONE',  ( -75.62287095715005592, -23.48783264082478084, -1.443836473390065489 ) ) ;
#9679 = CARTESIAN_POINT ( 'NONE',  ( -5.439936175300728927, -5.876774720514410077, 19.67454710845353816 ) ) ;
#9680 = CARTESIAN_POINT ( 'NONE',  ( -10.21242994381667657, -20.12718729479640700, -1.500000000000002220 ) ) ;
#9681 = DIRECTION ( 'NONE',  ( 0.000000000000000000, -0.000000000000000000, -1.000000000000000000 ) ) ;
#9682 = ORIENTED_EDGE ( 'NONE', *, *, #26797, .T. ) ;
#9683 = CARTESIAN_POINT ( 'NONE',  ( -79.98140449170570321, -25.29705034626280025, 4.546672010081276305 ) ) ;
#9684 = CARTESIAN_POINT ( 'NONE',  ( 2.904396343079095111, -6.376774720514415407, 19.95793242748194984 ) ) ;
#9685 = CARTESIAN_POINT ( 'NONE',  ( -15.16924259816527609, 12.53091941037558854, 11.49999999999999645 ) ) ;
#9686 = CARTESIAN_POINT ( 'NONE',  ( 6.660000000000001030, -2.191226316053958875E-18, 2.701633758479787833E-17 ) ) ;
#9687 = FACE_OUTER_BOUND ( 'NONE', #21059, .T. ) ;
#9688 = ORIENTED_EDGE ( 'NONE', *, *, #66428, .F. ) ;
#9689 = DIRECTION ( 'NONE',  ( 0.000000000000000000, 0.000000000000000000, 1.000000000000000000 ) ) ;
#9690 = CARTESIAN_POINT ( 'NONE',  ( -55.62287095715005592, -23.47593901973091235, -1.443836447539007972 ) ) ;
#9691 = EDGE_CURVE ( 'NONE', #35831, #10125, #97157, .T. ) ;
#9692 = DIRECTION ( 'NONE',  ( 1.000000000000000000, 0.000000000000000000, 0.000000000000000000 ) ) ;
#9693 = CARTESIAN_POINT ( 'NONE',  ( -95.52287095715011844, -24.83620972994591725, 8.398175272781369216 ) ) ;
#9694 = EDGE_CURVE ( 'NONE', #95924, #70766, #36754, .T. ) ;
#9695 = CARTESIAN_POINT ( 'NONE',  ( -126.5228709571500616, -29.50250243563736774, 8.947779886222132717 ) ) ;
#9696 = CARTESIAN_POINT ( 'NONE',  ( 18.24634267693259559, -7.554628487255452107, -1.500000000000002220 ) ) ;
#9697 = EDGE_LOOP ( 'NONE', ( #80618, #97957, #37094, #4192 ) ) ;
#9698 = EDGE_CURVE ( 'NONE', #20703, #67226, #42571, .T. ) ;
#9699 = CARTESIAN_POINT ( 'NONE',  ( -16.41926757845921614, -11.79510067912178606, 11.49999999999999645 ) ) ;
#9700 = CARTESIAN_POINT ( 'NONE',  ( -7.617563585130437076, -5.876774720514412742, 19.95084900476494383 ) ) ;
#9701 = EDGE_CURVE ( 'NONE', #38179, #5224, #23083, .T. ) ;
#9702 = AXIS2_PLACEMENT_3D ( 'NONE', #65730, #49496, #42880 ) ;
#9703 = VERTEX_POINT ( 'NONE', #42881 ) ;
#9704 = CARTESIAN_POINT ( 'NONE',  ( -117.6228709571500559, -29.50247984919015209, -1.443849546365046699 ) ) ;
#9705 = CARTESIAN_POINT ( 'NONE',  ( -7.641025641025638748, -6.376774720514427841, 21.75000000000001066 ) ) ;
#9706 = CARTESIAN_POINT ( 'NONE',  ( -68.62287095715005592, -23.47593901973091235, -1.443836447539006196 ) ) ;
#9707 = CARTESIAN_POINT ( 'NONE',  ( -83.22287095715010707, -23.47593901973090524, -1.443836447538997536 ) ) ;
#9708 = VECTOR ( 'NONE', #87860, 1000.000000000000000 ) ;
#9709 = CARTESIAN_POINT ( 'NONE',  ( -2.499999999999993339, 4.999999999999997335, 0.000000000000000000 ) ) ;
#9710 = LINE ( 'NONE', #79714, #98049 ) ;
#9711 = CARTESIAN_POINT ( 'NONE',  ( -20.00956492049148494, -0.6725752471728385640, 11.49999999999998934 ) ) ;
#9712 = ADVANCED_FACE ( 'NONE', ( #81927 ), #27651, .T. ) ;
#9713 = CARTESIAN_POINT ( 'NONE',  ( -62.62287095715004881, -23.47593901973091235, -1.443836447539007972 ) ) ;
#9714 = CARTESIAN_POINT ( 'NONE',  ( -116.5555263298079183, -23.96169478059713853, 10.65365249895717348 ) ) ;
#9715 = ORIENTED_EDGE ( 'NONE', *, *, #24533, .F. ) ;
#9716 = AXIS2_PLACEMENT_3D ( 'NONE', #98364, #35977, #20741 ) ;
#9717 = VECTOR ( 'NONE', #34214, 1000.000000000000114 ) ;
#9718 = DIRECTION ( 'NONE',  ( 0.000000000000000000, 1.000000000000000000, 0.000000000000000000 ) ) ;
#9719 = DIRECTION ( 'NONE',  ( -3.773278334444167608E-23, 1.000000000000000000, 0.000000000000000000 ) ) ;
#9720 = CARTESIAN_POINT ( 'NONE',  ( -79.37567067213733196, -25.28636030991100370, 5.689218636705552612 ) ) ;
#9721 = AXIS2_PLACEMENT_3D ( 'NONE', #53283, #51278, #83718 ) ;
#9722 = CARTESIAN_POINT ( 'NONE',  ( -124.5228709571500616, -24.65952944569305316, 1.056160979905705899 ) ) ;
#9723 = CARTESIAN_POINT ( 'NONE',  ( -83.64499529382760556, -23.48783264082477018, -1.443836473390093911 ) ) ;
#9724 = CIRCLE ( 'NONE', #66474, 2.899999999999999911 ) ;
#9725 = LINE ( 'NONE', #62515, #83571 ) ;
#9726 = LINE ( 'NONE', #55917, #97150 ) ;
#9727 = EDGE_LOOP ( 'NONE', ( #14667, #88221, #87997, #44930 ) ) ;
#9728 = CARTESIAN_POINT ( 'NONE',  ( 13.48481281434462531, 15.16087405922196041, 11.49999999999998934 ) ) ;
#9729 = CARTESIAN_POINT ( 'NONE',  ( 29.58524742607616176, 4.112217781777255610, 29.11978736867098760 ) ) ;
#9730 = CARTESIAN_POINT ( 'NONE',  ( -34.52672225899539171, -24.65952944569304606, 1.056160979905694353 ) ) ;
#9731 = CARTESIAN_POINT ( 'NONE',  ( -107.5228709571501184, -23.96177878511309345, 10.65340807706329507 ) ) ;
#9732 = EDGE_LOOP ( 'NONE', ( #86978, #2511, #25124, #92848 ) ) ;
#9734 = EDGE_CURVE ( 'NONE', #68021, #17108, #60396, .T. ) ;
#9733 = CARTESIAN_POINT ( 'NONE',  ( -81.62287095715008434, -24.34917612406837506, 0.1852690917426648154 ) ) ;
#9735 = CARTESIAN_POINT ( 'NONE',  ( -12.03079493616482765, -17.41531974249929249, 11.49999999999999645 ) ) ;
#9736 = CARTESIAN_POINT ( 'NONE',  ( 13.35222405703702186, 17.66689192352044913, 11.49999999999998934 ) ) ;
#9737 = EDGE_CURVE ( 'NONE', #70011, #9517, #71640, .T. ) ;
#9738 = CARTESIAN_POINT ( 'NONE',  ( 0.1292827521129817636, -20.55975067039486603, 11.49999999999998934 ) ) ;
#9739 = VERTEX_POINT ( 'NONE', #52483 ) ;
#9740 = CARTESIAN_POINT ( 'NONE',  ( -116.6228709571500559, -24.64965695001469115, 8.947790433994175174 ) ) ;
#9741 = EDGE_LOOP ( 'NONE', ( #41238, #56920, #92463, #55551 ) ) ;
#9742 = CARTESIAN_POINT ( 'NONE',  ( 7.166040305186291093, -6.376774720514420736, 20.81030863372915718 ) ) ;
#9743 = CARTESIAN_POINT ( 'NONE',  ( -110.6228709571500417, -24.15516710230295772, 10.28746687063727094 ) ) ;
#9744 = ORIENTED_EDGE ( 'NONE', *, *, #18343, .T. ) ;
#9745 = ORIENTED_EDGE ( 'NONE', *, *, #9441, .F. ) ;
#9746 = VERTEX_POINT ( 'NONE', #66231 ) ;
#9747 = LINE ( 'NONE', #79754, #4855 ) ;
#9748 = CARTESIAN_POINT ( 'NONE',  ( 6.727829057902616761, -5.876774720514417183, 20.13865202822440281 ) ) ;
#9749 = CARTESIAN_POINT ( 'NONE',  ( 5.329826657887789310, -6.376774720514418959, 20.66144943787464783 ) ) ;
#9750 = CARTESIAN_POINT ( 'NONE',  ( -9.011640028862021978, 18.61544202926687674, -1.500000000000002220 ) ) ;
#9751 = CARTESIAN_POINT ( 'NONE',  ( 21.02075834227166951, -5.193550065563941942, 11.49999999999999645 ) ) ;
#9752 = ORIENTED_EDGE ( 'NONE', *, *, #30514, .T. ) ;
#9753 = FACE_OUTER_BOUND ( 'NONE', #24210, .T. ) ;
#9754 = DIRECTION ( 'NONE',  ( 0.000000000000000000, 1.000000000000000000, 0.000000000000000000 ) ) ;
#9755 = CARTESIAN_POINT ( 'NONE',  ( 19.55810785529653373, 10.91776788121007868, 11.49999999999998934 ) ) ;
#9756 = LINE ( 'NONE', #26988, #75590 ) ;
#9757 = CARTESIAN_POINT ( 'NONE',  ( -84.58278115369181194, -24.65952944569303895, 1.056160979905700348 ) ) ;
#9758 = ORIENTED_EDGE ( 'NONE', *, *, #6536, .F. ) ;
#9759 = FACE_OUTER_BOUND ( 'NONE', #54566, .T. ) ;
#9760 = DIRECTION ( 'NONE',  ( -3.773278334453079030E-23, 0.9999999999976377785, 2.173523156925979128E-06 ) ) ;
#9761 = ORIENTED_EDGE ( 'NONE', *, *, #30298, .T. ) ;
#9762 = ORIENTED_EDGE ( 'NONE', *, *, #63312, .T. ) ;
#9763 = AXIS2_PLACEMENT_3D ( 'NONE', #88002, #80885, #97106 ) ;
#9764 = DIRECTION ( 'NONE',  ( 3.773278334444167608E-23, -1.000000000000000000, 0.000000000000000000 ) ) ;
#9765 = CC_DESIGN_DATE_AND_TIME_ASSIGNMENT ( #64257, #88075, ( #95340 ) ) ;
#9766 = ORIENTED_EDGE ( 'NONE', *, *, #77825, .T. ) ;
#9767 = DIRECTION ( 'NONE',  ( 2.145277261456712182E-39, 2.173523156925979128E-06, -0.9999999999976378895 ) ) ;
#9768 = CARTESIAN_POINT ( 'NONE',  ( -14.73150212448299357, 15.28860238833873808, -1.500000000000002220 ) ) ;
#9769 = ORIENTED_EDGE ( 'NONE', *, *, #3194, .F. ) ;
#9770 = CARTESIAN_POINT ( 'NONE',  ( -50.48629971621463142, -24.63355581998386867, 0.9682620441943859957 ) ) ;
#9771 = CARTESIAN_POINT ( 'NONE',  ( 15.22768361601695020, -15.61070304372801587, 11.49999999999998934 ) ) ;
#9772 = CARTESIAN_POINT ( 'NONE',  ( -103.5953284589405143, -23.73791477778911840, 11.05961554403170410 ) ) ;
#9773 = CARTESIAN_POINT ( 'NONE',  ( 7.343377932919765705, -6.376774720514422512, 21.31293098237466310 ) ) ;
#9774 = CARTESIAN_POINT ( 'NONE',  ( 5.963731207934512391, -5.876774720514413630, 19.80418863844947097 ) ) ;
#9775 = CARTESIAN_POINT ( 'NONE',  ( 13.86046232669119149, 16.88393516940953276, -1.500000000000002220 ) ) ;
#9776 = CARTESIAN_POINT ( 'NONE',  ( -30.57287095715004455, -25.10844925379378623, 7.250334085407572182 ) ) ;
#9777 = ORIENTED_EDGE ( 'NONE', *, *, #43739, .F. ) ;
#9778 = CARTESIAN_POINT ( 'NONE',  ( 25.25345159561841868, 4.807191536106888208, -10.50260803520238895 ) ) ;
#9779 = PLANE ( 'NONE',  #92887 ) ;
#9780 = ORIENTED_EDGE ( 'NONE', *, *, #36647, .T. ) ;
#9781 = EDGE_CURVE ( 'NONE', #1208, #25123, #65553, .T. ) ;
#9782 = ORIENTED_EDGE ( 'NONE', *, *, #68327, .T. ) ;
#9783 = B_SPLINE_CURVE_WITH_KNOTS ( 'NONE', 3,
 ( #71343, #10941, #80952, #32769 ),
 .UNSPECIFIED., .F., .F.,
 ( 4, 4 ),
 ( 0.000000000000000000, 9.999999999998897304E-05 ),
 .UNSPECIFIED. ) ;
#9784 = VECTOR ( 'NONE', #8038, 1000.000000000000000 ) ;
#9785 = ORIENTED_EDGE ( 'NONE', *, *, #28062, .F. ) ;
#9786 = CARTESIAN_POINT ( 'NONE',  ( -89.49044894935767047, -25.12049752546738191, 2.832404795212222659 ) ) ;
#9787 = CIRCLE ( 'NONE', #84304, 80.18232118519037499 ) ;
#9788 = CARTESIAN_POINT ( 'NONE',  ( -82.54408211365957015, -24.51314013834315375, 0.6176544820404155089 ) ) ;
#9789 = CARTESIAN_POINT ( 'NONE',  ( -21.08860491664495029, 2.407354197416772035, 11.49999999999998934 ) ) ;
#9790 = CARTESIAN_POINT ( 'NONE',  ( 30.54125281784916268, -0.6647747205144264315, 23.11160796525322070 ) ) ;
#9791 = CARTESIAN_POINT ( 'NONE',  ( -30.61333094834725088, -24.36247485673954927, 0.01136689895587368430 ) ) ;
#9792 = CARTESIAN_POINT ( 'NONE',  ( -73.62287095715005592, -29.50248528299804818, 1.056150453629036701 ) ) ;
#9793 = FACE_OUTER_BOUND ( 'NONE', #82030, .T. ) ;
#9794 = VECTOR ( 'NONE', #7557, 1000.000000000000227 ) ;
#9795 = CARTESIAN_POINT ( 'NONE',  ( 15.36829964806744364, -11.83880051060199712, -1.500000000000002220 ) ) ;
#9796 = CARTESIAN_POINT ( 'NONE',  ( -45.57860970357442909, -24.83618233451450408, 1.606449574219532384 ) ) ;
#9797 = ORIENTED_EDGE ( 'NONE', *, *, #91106, .F. ) ;
#9798 = CIRCLE ( 'NONE', #85925, 3.349999999999998757 ) ;
#9799 = CARTESIAN_POINT ( 'NONE',  ( -19.43040671759091609, -1.856541507571394467, 11.49999999999999645 ) ) ;
#9800 = CARTESIAN_POINT ( 'NONE',  ( -5.544977400725785266, -5.876774720514410077, 19.92818918856636401 ) ) ;
#9801 = EDGE_CURVE ( 'NONE', #97499, #16640, #4314, .T. ) ;
#9802 = CARTESIAN_POINT ( 'NONE',  ( -68.52287095715009002, -23.72747288104470087, -1.053458166803227014 ) ) ;
#9803 = ORIENTED_EDGE ( 'NONE', *, *, #76050, .F. ) ;
#9804 = DIRECTION ( 'NONE',  ( 0.000000000000000000, 0.000000000000000000, -1.000000000000000000 ) ) ;
#9805 = CARTESIAN_POINT ( 'NONE',  ( -89.55462902144884652, -23.96119346886881374, -0.6495511937831908167 ) ) ;
#9806 = CARTESIAN_POINT ( 'NONE',  ( -98.52287095715006160, -24.65952944569304606, 1.056160979905702346 ) ) ;
#9807 = B_SPLINE_CURVE_WITH_KNOTS ( 'NONE', 3,
 ( #72592, #55874, #57383, #65000 ),
 .UNSPECIFIED., .F., .F.,
 ( 4, 4 ),
 ( 0.000000000000000000, 1.000000000000000000 ),
 .UNSPECIFIED. ) ;
#9808 = CARTESIAN_POINT ( 'NONE',  ( -81.83126432988071031, -25.03155843045780315, 6.560967614844648743 ) ) ;
#9809 = CARTESIAN_POINT ( 'NONE',  ( -18.24527198174902765, 7.358211898524878336, -1.500000000000002220 ) ) ;
#9810 = ORIENTED_EDGE ( 'NONE', *, *, #13134, .T. ) ;
#9811 = EDGE_CURVE ( 'NONE', #11540, #68689, #5299, .T. ) ;
#9812 = CARTESIAN_POINT ( 'NONE',  ( -55.62287095715005592, -29.50248528299804818, 1.056150453629034924 ) ) ;
#9813 = CARTESIAN_POINT ( 'NONE',  ( -43.52287095715006160, -24.64898659630528854, 1.056161002820819261 ) ) ;
#9814 = EDGE_CURVE ( 'NONE', #65965, #8482, #81345, .T. ) ;
#9815 = DATE_AND_TIME ( #26549, #39254 ) ;
#9816 = CARTESIAN_POINT ( 'NONE',  ( 3.787259615384621192, -6.376774720514426065, 21.48076923076922640 ) ) ;
#9817 = CARTESIAN_POINT ( 'NONE',  ( -90.52287095715003318, -24.62285846331438321, 9.038163153548227413 ) ) ;
#9818 = CARTESIAN_POINT ( 'NONE',  ( -109.2887704616800590, -25.18211350563075257, 3.273023101274771918 ) ) ;
#9819 = CARTESIAN_POINT ( 'NONE',  ( -97.52218080935233502, -23.48786465467241413, 11.44779295918254469 ) ) ;
#9820 = CARTESIAN_POINT ( 'NONE',  ( -1.044871794871790938, -6.376774720514427841, 21.75000000000000355 ) ) ;
#9821 = CARTESIAN_POINT ( 'NONE',  ( 6.179707021866671646, -6.376774720514426065, 21.45334750074374242 ) ) ;
#9822 = CARTESIAN_POINT ( 'NONE',  ( -121.6228709571500843, -24.51387760970725083, 9.387446482453405849 ) ) ;
#9823 = CARTESIAN_POINT ( 'NONE',  ( -111.3776484685884327, -25.18425808373743635, 4.332404656630714612 ) ) ;
#9824 = CARTESIAN_POINT ( 'NONE',  ( -10.02925392579303576, -17.20239368982820238, -1.500000000000002220 ) ) ;
#9825 = EDGE_CURVE ( 'NONE', #73894, #95505, #88542, .T. ) ;
#9826 = CARTESIAN_POINT ( 'NONE',  ( -75.63385634215764242, -24.52399227489127043, 9.353111116836526406 ) ) ;
#9827 = CARTESIAN_POINT ( 'NONE',  ( -9.134819693115781902, 17.59984377705169933, -1.500000000000002220 ) ) ;
#9828 = ORIENTED_EDGE ( 'NONE', *, *, #64449, .T. ) ;
#9829 = CARTESIAN_POINT ( 'NONE',  ( 22.02124265030973760, 6.143225279485574397, 19.55402280011862004 ) ) ;
#9830 = CARTESIAN_POINT ( 'NONE',  ( -101.6228709571500559, -29.50248528299804818, 1.056150453629042030 ) ) ;
#9831 = CARTESIAN_POINT ( 'NONE',  ( -12.65407072091355722, 0.3587747205143968499, -26.15404995688569301 ) ) ;
#9832 = CARTESIAN_POINT ( 'NONE',  ( 2.040502595053849788, 20.68626321094233944, 11.49999999999999645 ) ) ;
#9833 = DIRECTION ( 'NONE',  ( 0.000000000000000000, -0.000000000000000000, -1.000000000000000000 ) ) ;
#9834 = CIRCLE ( 'NONE', #61719, 132.8284398600581824 ) ;
#9835 = CARTESIAN_POINT ( 'NONE',  ( -106.5926168708341635, -23.96119346886880308, -0.6495511937832030291 ) ) ;
#9836 = CARTESIAN_POINT ( 'NONE',  ( -13.73562189146022661, -18.16285900770654393, 11.49999999999999645 ) ) ;
#9837 = ORIENTED_EDGE ( 'NONE', *, *, #98676, .T. ) ;
#9838 = CARTESIAN_POINT ( 'NONE',  ( 29.73860345376319003, 5.356774720496559894, 19.84760796525321780 ) ) ;
#9839 = CARTESIAN_POINT ( 'NONE',  ( -100.6228709571500559, -25.00158670708909625, 2.256160236439166411 ) ) ;
#9840 = ORIENTED_EDGE ( 'NONE', *, *, #43489, .T. ) ;
#9841 = CARTESIAN_POINT ( 'NONE',  ( 14.71488472389458124, -13.84269218943631508, -1.500000000000002220 ) ) ;
#9842 = FACE_OUTER_BOUND ( 'NONE', #99215, .T. ) ;
#9843 = CARTESIAN_POINT ( 'NONE',  ( -69.55620429048339304, -23.48783264082478084, -1.443836473390067265 ) ) ;
#9844 = ORIENTED_EDGE ( 'NONE', *, *, #67711, .F. ) ;
#9845 = DIRECTION ( 'NONE',  ( -0.000000000000000000, 1.000000000000000000, -0.000000000000000000 ) ) ;
#9846 = CARTESIAN_POINT ( 'NONE',  ( -10.40290173325841216, 6.376774720514426953, 27.45402280011861862 ) ) ;
#9847 = AXIS2_PLACEMENT_3D ( 'NONE', #86039, #53612, #32251 ) ;
#9848 = CARTESIAN_POINT ( 'NONE',  ( -11.50144725928494438, 16.33591932373696665, -1.500000000000002220 ) ) ;
#9849 = CYLINDRICAL_SURFACE ( 'NONE', #31827, 12.23252173913042995 ) ;
#9850 = CARTESIAN_POINT ( 'NONE',  ( 13.87900837158347755, -15.70065903812341013, 11.49999999999999645 ) ) ;
#9851 = VECTOR ( 'NONE', #78242, 1000.000000000000000 ) ;
#9852 = CARTESIAN_POINT ( 'NONE',  ( -106.5228709571500758, -24.64898659630368627, 1.056161002820831474 ) ) ;
#9853 = CARTESIAN_POINT ( 'NONE',  ( -93.52287095715007581, -23.96177878511308990, 10.65340807706329684 ) ) ;
#9854 = CARTESIAN_POINT ( 'NONE',  ( 9.306852550357104903, -20.00191182576189064, -1.500000000000002220 ) ) ;
#9855 = B_SPLINE_CURVE_WITH_KNOTS ( 'NONE', 3,
 ( #4278, #17997, #49465, #18493 ),
 .UNSPECIFIED., .F., .F.,
 ( 4, 4 ),
 ( 0.000000000000000000, 9.999999999998897304E-05 ),
 .UNSPECIFIED. ) ;
#9856 = B_SPLINE_CURVE_WITH_KNOTS ( 'NONE', 3,
 ( #34384, #87165, #26268, #11046, #65361, #96280, #79046, #40501 ),
 .UNSPECIFIED., .F., .F.,
 ( 4, 2, 2, 4 ),
 ( 0.000000000000000000, 0.002001098010032682784, 0.003001647015049024175, 0.004002196020065365567 ),
 .UNSPECIFIED. ) ;
#9857 = CARTESIAN_POINT ( 'NONE',  ( -124.4728709548940486, -25.21112548385455199, 2.000950967214091936 ) ) ;
#9859 = ORIENTED_EDGE ( 'NONE', *, *, #5950, .T. ) ;
#9858 = ADVANCED_FACE ( 'NONE', ( #22997, #46358 ), #82959, .T. ) ;
#9860 = CARTESIAN_POINT ( 'NONE',  ( -127.6228709571500275, -23.48786465467242124, 11.44779295918253403 ) ) ;
#9861 = CARTESIAN_POINT ( 'NONE',  ( -118.5228709571501184, -23.96177878511310055, 10.65340807706329507 ) ) ;
#9862 = CARTESIAN_POINT ( 'NONE',  ( -72.63936276973265649, -23.96119346886880663, -0.6495511937832119109 ) ) ;
#9863 = ORIENTED_EDGE ( 'NONE', *, *, #52297, .F. ) ;
#9864 = CARTESIAN_POINT ( 'NONE',  ( 3.632744579681756569, -6.376774720514402972, 18.17103827887095946 ) ) ;
#9865 = ORIENTED_EDGE ( 'NONE', *, *, #37159, .F. ) ;
#9866 = ORIENTED_EDGE ( 'NONE', *, *, #38979, .T. ) ;
#9867 = CARTESIAN_POINT ( 'NONE',  ( -101.7776484685884242, -25.26303730729093644, 3.986250639247583827 ) ) ;
#9868 = CARTESIAN_POINT ( 'NONE',  ( -4.444543648262984981, 12.92677669529668627, 2.100000000000000089 ) ) ;
#9869 = CARTESIAN_POINT ( 'NONE',  ( 30.53060340732035982, -1.477225279485574028, 19.84760796525321780 ) ) ;
#9870 = CARTESIAN_POINT ( 'NONE',  ( -19.38928925021375349, 6.733644070511561885, -1.500000000000002220 ) ) ;
#9871 = VERTEX_POINT ( 'NONE', #7286 ) ;
#9872 = DIRECTION ( 'NONE',  ( -3.773278334453079618E-23, 0.9999999999976377785, 2.173523156925979975E-06 ) ) ;
#9873 = CARTESIAN_POINT ( 'NONE',  ( 6.586338672804227024, -5.876774720514415407, 20.10086663068103618 ) ) ;
#9874 = DIRECTION ( 'NONE',  ( 0.000000000000000000, 0.000000000000000000, 1.000000000000000000 ) ) ;
#9875 = CARTESIAN_POINT ( 'NONE',  ( -6.278373996654322831, -21.41630973362384083, -1.500000000000002220 ) ) ;
#9876 = CARTESIAN_POINT ( 'NONE',  ( -90.62287095715004170, -23.47593901973091235, -1.443836447539002865 ) ) ;
#9877 = CARTESIAN_POINT ( 'NONE',  ( -1.955883090540335045, -5.876774720514411854, 19.49432735726521315 ) ) ;
#9878 = ORIENTED_EDGE ( 'NONE', *, *, #81083, .F. ) ;
#9879 = CARTESIAN_POINT ( 'NONE',  ( 32.84232313084847732, -4.840274619473232676, -11.71291885348859196 ) ) ;
#9880 = CARTESIAN_POINT ( 'NONE',  ( 3.787259615384621192, -5.876774720514425177, 21.48076923076922640 ) ) ;
#9881 = CARTESIAN_POINT ( 'NONE',  ( -5.376107494350208960, -20.15860285114975525, 11.49999999999998934 ) ) ;
#9882 = VERTEX_POINT ( 'NONE', #99624 ) ;
#9884 = ORIENTED_EDGE ( 'NONE', *, *, #11963, .F. ) ;
#9883 = CARTESIAN_POINT ( 'NONE',  ( -79.52287095715007581, -24.35013146730203815, 9.818937971375103047 ) ) ;
#9885 = ADVANCED_FACE ( 'NONE', ( #32127 ), #85454, .T. ) ;
#9886 = VERTEX_POINT ( 'NONE', #11298 ) ;
#9887 = CARTESIAN_POINT ( 'NONE',  ( -70.15801421577009478, -25.25935349274321950, 7.556454315002589794 ) ) ;
#9888 = CARTESIAN_POINT ( 'NONE',  ( 11.68726034403320746, 17.49698133428071145, -1.500000000000002220 ) ) ;
#9889 = EDGE_LOOP ( 'NONE', ( #50411, #68210, #37091, #77362 ) ) ;
#9890 = CARTESIAN_POINT ( 'NONE',  ( -110.6228709571500559, -29.50248789122583659, 2.256150453626215580 ) ) ;
#9891 = DIRECTION ( 'NONE',  ( 0.000000000000000000, -0.9967269304714136968, -0.08084198211964954695 ) ) ;
#9892 = FACE_OUTER_BOUND ( 'NONE', #44353, .T. ) ;
#9893 = EDGE_CURVE ( 'NONE', #9578, #54063, #33641, .T. ) ;
#9894 = CARTESIAN_POINT ( 'NONE',  ( -101.5316874056614012, -25.03152356804190148, 7.138213056438796222 ) ) ;
#9895 = CARTESIAN_POINT ( 'NONE',  ( -87.52287095715006160, -24.66019654487200086, 8.947790411086115725 ) ) ;
#9896 = CARTESIAN_POINT ( 'NONE',  ( -0.4625342273119020797, 21.68341340789531912, -1.500000000000002220 ) ) ;
#9897 = CARTESIAN_POINT ( 'NONE',  ( -78.62287095715005592, -29.50250786944525672, 11.44777988621623521 ) ) ;
#9899 = ORIENTED_EDGE ( 'NONE', *, *, #29719, .F. ) ;
#9898 = CARTESIAN_POINT ( 'NONE',  ( -18.12599551585701008, -12.76988789260850332, 11.49999999999999645 ) ) ;
#9900 = CARTESIAN_POINT ( 'NONE',  ( -98.89859089807453074, -25.27745440479792194, 5.967653818798817511 ) ) ;
#9901 = PLANE ( 'NONE',  #14868 ) ;
#9902 = ORIENTED_EDGE ( 'NONE', *, *, #39788, .T. ) ;
#9903 = CARTESIAN_POINT ( 'NONE',  ( -20.89466310375201985, -8.809181082428260368, -1.500000000000002220 ) ) ;
#9904 = EDGE_CURVE ( 'NONE', #34855, #41225, #35352, .T. ) ;
#9905 = EDGE_CURVE ( 'NONE', #36332, #79116, #18903, .T. ) ;
#9907 = VERTEX_POINT ( 'NONE', #71202 ) ;
#9906 = CARTESIAN_POINT ( 'NONE',  ( -6.720452724358975338, -6.376774720514411854, 19.46153846153846700 ) ) ;
#9908 = ORIENTED_EDGE ( 'NONE', *, *, #48589, .T. ) ;
#9909 = EDGE_CURVE ( 'NONE', #27856, #57803, #96036, .T. ) ;
#9910 = CARTESIAN_POINT ( 'NONE',  ( 31.13513474936813807, -5.356774720514427379, 3.331262582247329185 ) ) ;
#9911 = AXIS2_PLACEMENT_3D ( 'NONE', #4818, #97657, #98143 ) ;
#9912 = CARTESIAN_POINT ( 'NONE',  ( -17.93149374516376682, -9.230432107326475233, -1.500000000000002220 ) ) ;
#9913 = DIRECTION ( 'NONE',  ( -1.000000000000000000, 0.000000000000000000, 0.000000000000000000 ) ) ;
#9914 = ORIENTED_EDGE ( 'NONE', *, *, #12776, .T. ) ;
#9915 = CARTESIAN_POINT ( 'NONE',  ( -42.62287095715006302, -23.96177878511307568, 10.65340807706330395 ) ) ;
#9916 = CARTESIAN_POINT ( 'NONE',  ( 18.93296920960566965, -11.98514031388154599, -1.500000000000002220 ) ) ;
#9917 = EDGE_CURVE ( 'NONE', #13466, #48086, #94028, .T. ) ;
#9918 = ORIENTED_EDGE ( 'NONE', *, *, #27493, .F. ) ;
#9919 = ORIENTED_EDGE ( 'NONE', *, *, #32964, .T. ) ;
#9920 = LINE ( 'NONE', #25646, #22300 ) ;
#9921 = CARTESIAN_POINT ( 'NONE',  ( -4.223504350552545361, -6.376774720514411854, 19.52341893546492813 ) ) ;
#9922 = CARTESIAN_POINT ( 'NONE',  ( -61.52287095715004739, -24.50321055353803956, 9.387540953477522265 ) ) ;
#9923 = CARTESIAN_POINT ( 'NONE',  ( 30.77956504631911017, 6.277769580494330093, 0.6965969997247714041 ) ) ;
#9924 = CARTESIAN_POINT ( 'NONE',  ( -130.5728709571500588, -24.26743686635981234, 0.04347934593174140189 ) ) ;
#9925 = VECTOR ( 'NONE', #8818, 1000.000000000000114 ) ;
#9926 = CARTESIAN_POINT ( 'NONE',  ( 2.036066721924049805, 19.47704226162102614, -1.500000000000002220 ) ) ;
#9927 = CARTESIAN_POINT ( 'NONE',  ( -46.64649278270903920, -23.96119346886879953, -0.6495511937832144644 ) ) ;
#9929 = VERTEX_POINT ( 'NONE', #88429 ) ;
#9928 = AXIS2_PLACEMENT_3D ( 'NONE', #33391, #49148, #64382 ) ;
#9930 = CARTESIAN_POINT ( 'NONE',  ( 12.90647603486358364, 17.18646895862681134, -1.500000000000002220 ) ) ;
#9931 = CARTESIAN_POINT ( 'NONE',  ( -128.6243649391845452, -23.48783264082479150, -1.443836473390056829 ) ) ;
#9932 = CARTESIAN_POINT ( 'NONE',  ( -41.32836283488544638, -4.132774720514426292, 39.26872235229541985 ) ) ;
#9933 = CARTESIAN_POINT ( 'NONE',  ( -123.5228709571500474, -24.35013146730205236, 9.818937971375085283 ) ) ;
#9934 = DIRECTION ( 'NONE',  ( 1.000000000000000000, 3.773278334444167608E-23, 8.201307833595939069E-29 ) ) ;
#9935 = CARTESIAN_POINT ( 'NONE',  ( -17.45619364963476627, 14.87644265977633573, -1.500000000000002220 ) ) ;
#9936 = ADVANCED_FACE ( 'NONE', ( #25012 ), #13278, .T. ) ;
#9937 = EDGE_CURVE ( 'NONE', #54444, #31854, #53503, .T. ) ;
#9938 = PERSON_AND_ORGANIZATION_ROLE ( 'creator' ) ;
#9939 = DIRECTION ( 'NONE',  ( 0.000000000000000000, -1.000000000000000000, -2.891205793294678819E-16 ) ) ;
#9940 = CARTESIAN_POINT ( 'NONE',  ( -42.52287095715006870, -23.73907113217662257, -1.053371485781402495 ) ) ;
#9941 = CARTESIAN_POINT ( 'NONE',  ( -13.04681709000290013, -15.30929823114697541, 11.49999999999999645 ) ) ;
#9942 = CARTESIAN_POINT ( 'NONE',  ( 5.087148743171193033, 3.314277014504871222, -27.56324057082087364 ) ) ;
#9943 = CARTESIAN_POINT ( 'NONE',  ( 30.53060340732036693, 5.234153290856875529, 0.4067587357809892556 ) ) ;
#9944 = DIRECTION ( 'NONE',  ( -0.7071067811865452413, 8.659560562354961208E-17, -0.7071067811865497932 ) ) ;
#9945 = CARTESIAN_POINT ( 'NONE',  ( 6.660000000000001030, -0.2368809837866516499, 5.288828319098142217 ) ) ;
#9946 = LINE ( 'NONE', #86070, #59192 ) ;
#9947 = CARTESIAN_POINT ( 'NONE',  ( -17.59554656748941071, 9.132484154288260214, -1.500000000000002220 ) ) ;
#9948 = EDGE_CURVE ( 'NONE', #33339, #45268, #12316, .T. ) ;
#9949 = CARTESIAN_POINT ( 'NONE',  ( -4.706806674773570620, -21.25045708977441450, -1.500000000000002220 ) ) ;
#9950 = DIRECTION ( 'NONE',  ( -1.000000000000000000, -3.773278334444166432E-23, -8.201307841325785021E-29 ) ) ;
#9951 = CARTESIAN_POINT ( 'NONE',  ( -3.832734262880480358, 19.25313627021017382, -1.500000000000002220 ) ) ;
#9952 = LINE ( 'NONE', #35305, #7032 ) ;
#9953 = ADVANCED_FACE ( 'NONE', ( #82796 ), #44749, .T. ) ;
#9954 = EDGE_CURVE ( 'NONE', #49044, #18516, #97034, .T. ) ;
#9955 = CARTESIAN_POINT ( 'NONE',  ( -54.52287095715005449, -24.66019654487198665, 8.947790411086121054 ) ) ;
#9956 = ITEM_DEFINED_TRANSFORMATION ( 'NONE', 'NONE', #89327,  #37391 ) ;
#9957 = CARTESIAN_POINT ( 'NONE',  ( -103.5228709571500900, -23.72747288104470087, -1.053458166803225016 ) ) ;
#9958 = CARTESIAN_POINT ( 'NONE',  ( 2.589743589743596086, -5.876774720514416295, 20.00140224358974095 ) ) ;
#9959 = CARTESIAN_POINT ( 'NONE',  ( -19.86366060283327784, 5.362777492974458049, 11.49999999999999645 ) ) ;
#9960 = CARTESIAN_POINT ( 'NONE',  ( -0.02075734969026423599, -3.316774720514426456, -0.08597719988137648983 ) ) ;
#9961 = B_SPLINE_CURVE_WITH_KNOTS ( 'NONE', 3,
 ( #48980, #47976, #1802, #9399, #18515, #57600 ),
 .UNSPECIFIED., .F., .F.,
 ( 4, 2, 4 ),
 ( 6.384118694656723962E-06, 0.001386860460836396997, 0.002767336802978137555 ),
 .UNSPECIFIED. ) ;
#9962 = DIRECTION ( 'NONE',  ( 0.5656310827093757876, -0.8246584009594636333, -1.161164194647627127E-16 ) ) ;
#9963 = CARTESIAN_POINT ( 'NONE',  ( 12.73759380600583846, -18.68238426224762350, 11.49999999999999645 ) ) ;
#9964 = ORIENTED_EDGE ( 'NONE', *, *, #72035, .T. ) ;
#9965 = CARTESIAN_POINT ( 'NONE',  ( 13.10664265030973930, 0.3587747205144256601, -28.18129937523770678 ) ) ;
#9966 = CARTESIAN_POINT ( 'NONE',  ( 6.150000000000003908, 1.999999999999998224, 24.00000000000000000 ) ) ;
#9967 = CARTESIAN_POINT ( 'NONE',  ( -97.58661751571909804, -24.51314013834315730, 0.6176544820404147318 ) ) ;
#9968 = LINE ( 'NONE', #87599, #14270 ) ;
#9969 = CARTESIAN_POINT ( 'NONE',  ( -26.72222193076970953, -24.93063575608347193, 7.978874889883705634 ) ) ;
#9970 = CARTESIAN_POINT ( 'NONE',  ( -125.5895376238167245, -23.47596703998600631, 11.44779298504227683 ) ) ;
#9971 = EDGE_LOOP ( 'NONE', ( #79923, #15101, #4026, #2415 ) ) ;
#9972 = CARTESIAN_POINT ( 'NONE',  ( 21.75596283627254479, -7.788036635067100200, 11.49999999999999645 ) ) ;
#9973 = CARTESIAN_POINT ( 'NONE',  ( -22.76716317511769461, -1.676022972194794791, 11.49999999999998934 ) ) ;
#9974 = CARTESIAN_POINT ( 'NONE',  ( -110.6714443448221061, -25.19142773143022040, 3.340183518868431456 ) ) ;
#9975 = DIRECTION ( 'NONE',  ( 0.000000000000000000, 0.000000000000000000, -1.000000000000000000 ) ) ;
#9976 = CARTESIAN_POINT ( 'NONE',  ( -82.50599685478756840, -24.35071581493543036, 9.817618358456032368 ) ) ;
#9977 = CARTESIAN_POINT ( 'NONE',  ( 21.68943130245101258, -6.005725296444199834, 11.49999999999999645 ) ) ;
#9978 = ORIENTED_EDGE ( 'NONE', *, *, #77120, .T. ) ;
#9979 = CARTESIAN_POINT ( 'NONE',  ( -43.48234448701215626, -24.65952944569304606, 1.056160979905694131 ) ) ;
#9980 = AXIS2_PLACEMENT_3D ( 'NONE', #91177, #28787, #68849 ) ;
#9981 = CARTESIAN_POINT ( 'NONE',  ( -21.86317675896206225, -2.224439152981679602, 11.49999999999998934 ) ) ;
#9982 = CARTESIAN_POINT ( 'NONE',  ( -127.4728709570019163, -25.40556189117671693, 4.803963375099988831 ) ) ;
#9983 = CARTESIAN_POINT ( 'NONE',  ( 10.27515206207115739, 5.152774720514427642, -28.04856579873300149 ) ) ;
#9984 = DIRECTION ( 'NONE',  ( 0.000000000000000000, 0.000000000000000000, -1.000000000000000000 ) ) ;
#9985 = VERTEX_POINT ( 'NONE', #89919 ) ;
#9986 = CARTESIAN_POINT ( 'NONE',  ( -48.53562084801200882, -24.51419770103156637, 9.386484678747178734 ) ) ;
#9987 = LINE ( 'NONE', #33318, #47856 ) ;
#9988 = ORIENTED_EDGE ( 'NONE', *, *, #99355, .T. ) ;
#9989 = CARTESIAN_POINT ( 'NONE',  ( 20.06376955418885899, 4.186446014007643157, -1.500000000000002220 ) ) ;
#9990 = VERTEX_POINT ( 'NONE', #66614 ) ;
#9991 = ORIENTED_EDGE ( 'NONE', *, *, #52181, .F. ) ;
#9992 = ORIENTED_EDGE ( 'NONE', *, *, #12897, .F. ) ;
#9993 = ORIENTED_EDGE ( 'NONE', *, *, #79212, .F. ) ;
#9994 = CARTESIAN_POINT ( 'NONE',  ( -84.62287095715005592, -23.48783264082479150, -1.443836473390065489 ) ) ;
#9995 = CARTESIAN_POINT ( 'NONE',  ( 15.98122378838116120, 16.67787885001082770, -1.500000000000002220 ) ) ;
#9996 = CARTESIAN_POINT ( 'NONE',  ( -63.92287095715007439, -23.47596703998600631, 11.44779298504227860 ) ) ;
#9997 = CARTESIAN_POINT ( 'NONE',  ( 3.964343641299885146, 19.94596313931659992, -1.500000000000002220 ) ) ;
#9998 = VERTEX_POINT ( 'NONE', #75673 ) ;
#9999 = DIRECTION ( 'NONE',  ( 0.000000000000000000, 1.000000000000000000, 0.000000000000000000 ) ) ;
#10000 = CARTESIAN_POINT ( 'NONE',  ( -51.34369400408914430, -25.18091725095096578, 3.196477947496687122 ) ) ;
#10002 = CARTESIAN_POINT ( 'NONE',  ( -46.55620429048339304, -24.65952944569304606, 1.056160979905694797 ) ) ;
#10001 = CIRCLE ( 'NONE', #21352, 84.76210982660168725 ) ;
#10003 = CARTESIAN_POINT ( 'NONE',  ( -63.52287095715007581, -24.50321055353804667, 9.387540953477527594 ) ) ;
#10005 = ORIENTED_EDGE ( 'NONE', *, *, #46233, .T. ) ;
#10004 = CARTESIAN_POINT ( 'NONE',  ( -19.98823316618875268, 7.996883007359760320, 11.49999999999999645 ) ) ;
#10006 = CARTESIAN_POINT ( 'NONE',  ( -29.10059600771309007, -25.21531925493635740, 3.504324800834513809 ) ) ;
#10007 = CARTESIAN_POINT ( 'NONE',  ( -49.26189073845563371, -25.26385756805315452, 4.538720795355990489 ) ) ;
#10008 = APPROVAL_PERSON_ORGANIZATION ( #60003, #56877, #73226 ) ;
#10009 = ORIENTED_EDGE ( 'NONE', *, *, #43077, .F. ) ;
#10010 = CARTESIAN_POINT ( 'NONE',  ( 6.562613027033147084, 19.67253995144353240, 11.49999999999998934 ) ) ;
#10011 = EDGE_LOOP ( 'NONE', ( #82370, #55883, #93879, #19821 ) ) ;
#10013 = VERTEX_POINT ( 'NONE', #20388 ) ;
#10012 = CARTESIAN_POINT ( 'NONE',  ( -125.5215409636243606, -23.85016227208582151, -0.8807180028928047744 ) ) ;
#10014 = EDGE_CURVE ( 'NONE', #61766, #32857, #34448, .T. ) ;
#10015 = CARTESIAN_POINT ( 'NONE',  ( -92.62287095715005592, -29.50250786944525672, 11.44777988621623344 ) ) ;
#10016 = CARTESIAN_POINT ( 'NONE',  ( -51.89093686186974708, -25.27661087114319471, 5.843785486462916623 ) ) ;
#10017 = ORIENTED_EDGE ( 'NONE', *, *, #99155, .T. ) ;
#10018 = ORIENTED_EDGE ( 'NONE', *, *, #93177, .F. ) ;
#10019 = CARTESIAN_POINT ( 'NONE',  ( 2.021814659504407579E-13, -19.30000000000000426, -1.500000000000002220 ) ) ;
#10020 = DIRECTION ( 'NONE',  ( 0.000000000000000000, 1.000000000000000000, 0.000000000000000000 ) ) ;
#10021 = CARTESIAN_POINT ( 'NONE',  ( -30.64752034897746924, -23.47593901973090169, -1.443836447538997758 ) ) ;
#10023 = EDGE_LOOP ( 'NONE', ( #81029, #64190, #34250, #83507 ) ) ;
#10022 = CARTESIAN_POINT ( 'NONE',  ( 11.67614657018352453, 18.69773523334854914, 11.49999999999999645 ) ) ;
#10024 = CARTESIAN_POINT ( 'NONE',  ( -49.02498481075217995, -25.18391117716921102, 6.789210593061082655 ) ) ;
#10025 = CARTESIAN_POINT ( 'NONE',  ( -21.83012794225054165, -5.757306806698124113, -1.500000000000002220 ) ) ;
#10026 = EDGE_CURVE ( 'NONE', #11110, #22234, #61941, .T. ) ;
#10027 = EDGE_CURVE ( 'NONE', #38334, #98743, #12282, .T. ) ;
#10028 = EDGE_CURVE ( 'NONE', #28216, #94830, #67594, .T. ) ;
#10030 = EDGE_LOOP ( 'NONE', ( #74636, #93343, #86617, #6401 ) ) ;
#10029 = CARTESIAN_POINT ( 'NONE',  ( -80.96226385320382235, -25.13069340115295702, 2.947789388436138580 ) ) ;
#10031 = ORIENTED_EDGE ( 'NONE', *, *, #84034, .T. ) ;
#10032 = EDGE_CURVE ( 'NONE', #73391, #95103, #7461, .T. ) ;
#10033 = CARTESIAN_POINT ( 'NONE',  ( -88.52287095715000476, -24.35013146730203815, 9.818937971375095941 ) ) ;
#10034 = VECTOR ( 'NONE', #25118, 1000.000000000000000 ) ;
#10035 = CARTESIAN_POINT ( 'NONE',  ( 22.02124265030973760, -6.376774720514428729, 16.20402280011862217 ) ) ;
#10036 = ORIENTED_EDGE ( 'NONE', *, *, #19406, .F. ) ;
#10037 = CARTESIAN_POINT ( 'NONE',  ( 9.152908845159860363, 19.05633030926415472, 11.49999999999998934 ) ) ;
#10038 = CARTESIAN_POINT ( 'NONE',  ( -34.62287095715005592, -24.66019654487199020, 8.947790411086137041 ) ) ;
#10039 = CARTESIAN_POINT ( 'NONE',  ( -51.93023907722363219, -25.03148449460395142, 6.217084953208106946 ) ) ;
#10040 = CARTESIAN_POINT ( 'NONE',  ( -6.752792875861700850, -5.876774720514411854, 19.46247113826586528 ) ) ;
#10041 = CARTESIAN_POINT ( 'NONE',  ( -100.6228709571500559, -25.00158670708909625, 2.256160236439166411 ) ) ;
#10042 = CARTESIAN_POINT ( 'NONE',  ( -18.24902840909259538, -12.68162010772806170, -1.500000000000002220 ) ) ;
#10043 = LINE ( 'NONE', #24758, #12729 ) ;
#10044 = EDGE_CURVE ( 'NONE', #53562, #52778, #73978, .T. ) ;
#10045 = VERTEX_POINT ( 'NONE', #98011 ) ;
#10046 = CARTESIAN_POINT ( 'NONE',  ( -112.5228709571500616, -23.48783264083431988, -1.443836473375253782 ) ) ;
#10047 = CARTESIAN_POINT ( 'NONE',  ( -48.62287095715004881, -23.47593901973091235, -1.443836447539009749 ) ) ;
#10048 = CARTESIAN_POINT ( 'NONE',  ( -15.52061920455031618, -11.66286593722069931, 11.49999999999999645 ) ) ;
#10049 = CARTESIAN_POINT ( 'NONE',  ( -36.64213109380347078, -24.15620529776627379, 10.23563542870660825 ) ) ;
#10050 = SPHERICAL_SURFACE ( 'NONE', #12943, 6.600000000000001421 ) ;
#10051 = ADVANCED_FACE ( 'NONE', ( #76173 ), #45741, .T. ) ;
#10052 = CARTESIAN_POINT ( 'NONE',  ( -15.31790942089943286, 12.02624123284522106, 11.49999999999998934 ) ) ;
#10053 = CARTESIAN_POINT ( 'NONE',  ( -12.70309173801008562, -17.24390854791867511, 11.49999999999998934 ) ) ;
#10054 = DIRECTION ( 'NONE',  ( -1.000000000000000000, 0.000000000000000000, 0.000000000000000000 ) ) ;
#10055 = CARTESIAN_POINT ( 'NONE',  ( -60.59906223043246598, -24.15602025861359792, 10.28564288302606045 ) ) ;
#10056 = VECTOR ( 'NONE', #86825, 1000.000000000000114 ) ;
#10057 = CARTESIAN_POINT ( 'NONE',  ( -51.65198956701329536, -23.73766607897669445, -1.055555164236457788 ) ) ;
#10058 = CARTESIAN_POINT ( 'NONE',  ( -91.52287095715006160, -23.47596703998600631, 11.44779298504228393 ) ) ;
#10059 = B_SPLINE_CURVE_WITH_KNOTS ( 'NONE', 3,
 ( #14889, #46854, #92515, #6780, #37738, #31116 ),
 .UNSPECIFIED., .F., .F.,
 ( 4, 2, 4 ),
 ( 0.000000000000000000, 0.001380764517854760412, 0.002761529035709520824 ),
 .UNSPECIFIED. ) ;
#10060 = CARTESIAN_POINT ( 'NONE',  ( 22.67573665902413182, 1.879276792517311501, -1.500000000000002220 ) ) ;
#10061 = EDGE_CURVE ( 'NONE', #69079, #33824, #71749, .T. ) ;
#10062 = CARTESIAN_POINT ( 'NONE',  ( 27.53860345374808460, -6.475225279485576024, -9.012039699465272946 ) ) ;
#10063 = CARTESIAN_POINT ( 'NONE',  ( -102.5602245887073991, -23.48783264082478084, -1.443836473390064379 ) ) ;
#10064 = DIRECTION ( 'NONE',  ( 0.000000000000000000, 0.000000000000000000, 1.000000000000000000 ) ) ;
#10065 = CARTESIAN_POINT ( 'NONE',  ( 9.833179757865110560, 17.22857952739193266, 11.49999999999999645 ) ) ;
#10066 = CARTESIAN_POINT ( 'NONE',  ( -123.5886720077133134, -24.66019654487200441, 8.947790411086106843 ) ) ;
#10067 = LINE ( 'NONE', #58252, #52213 ) ;
#10068 = CARTESIAN_POINT ( 'NONE',  ( 33.13288845015618023, -5.965225279485572685, -0.1650522222209214185 ) ) ;
#10069 = ORIENTED_EDGE ( 'NONE', *, *, #67137, .T. ) ;
#10070 = CARTESIAN_POINT ( 'NONE',  ( -92.52287095715006160, -29.50250243563736774, 8.947779886222139822 ) ) ;
#10071 = CARTESIAN_POINT ( 'NONE',  ( -19.80875734969026425, 5.965225279485572685, 31.02402280011862246 ) ) ;
#10072 = CARTESIAN_POINT ( 'NONE',  ( -71.52287095715003318, -23.95044443724991723, 10.65354141964649415 ) ) ;
#10073 = CARTESIAN_POINT ( 'NONE',  ( 7.679218611123722837, 20.28660689097963399, -1.500000000000002220 ) ) ;
#10074 = CARTESIAN_POINT ( 'NONE',  ( -56.55352364353050376, -23.96169478059713498, 10.65365249895718236 ) ) ;
#10075 = CARTESIAN_POINT ( 'NONE',  ( -6.230579426152004885, -18.48807627814308674, -1.500000000000002220 ) ) ;
#10076 = CARTESIAN_POINT ( 'NONE',  ( -55.51140977391407461, -23.85049219812686161, 10.88485053497527133 ) ) ;
#10077 = EDGE_CURVE ( 'NONE', #31685, #20729, #21879, .T. ) ;
#10078 = VECTOR ( 'NONE', #37421, 1000.000000000000000 ) ;
#10079 = VERTEX_POINT ( 'NONE', #14776 ) ;
#10080 = CC_DESIGN_APPROVAL ( #71746, ( #34522 ) ) ;
#10081 = CARTESIAN_POINT ( 'NONE',  ( 20.39576089869593289, -0.2533167397448486957, 11.49999999999999645 ) ) ;
#10082 = CARTESIAN_POINT ( 'NONE',  ( -83.52287095715006160, -24.64965694238407323, 8.947790433994198267 ) ) ;
#10083 = EDGE_CURVE ( 'NONE', #4321, #19038, #16285, .T. ) ;
#10084 = PLANE ( 'NONE',  #70733 ) ;
#10085 = ORIENTED_EDGE ( 'NONE', *, *, #7411, .T. ) ;
#10086 = DIRECTION ( 'NONE',  ( -1.000000000000000000, -0.000000000000000000, -0.000000000000000000 ) ) ;
#10087 = CARTESIAN_POINT ( 'NONE',  ( -28.32169924589829080, 0.3587747205143964613, -8.244178532169451401 ) ) ;
#10088 = CARTESIAN_POINT ( 'NONE',  ( -114.5228709571500758, -23.47593901973090524, -1.443836447538996204 ) ) ;
#10089 = CARTESIAN_POINT ( 'NONE',  ( -50.52287095715006160, -23.48783264082477018, -1.443836473390095021 ) ) ;
#10090 = CARTESIAN_POINT ( 'NONE',  ( -1.044792363895550302, -6.376774720514417183, 20.41272575174754422 ) ) ;
#10091 = PLANE ( 'NONE',  #30578 ) ;
#10092 = ORIENTED_EDGE ( 'NONE', *, *, #57819, .F. ) ;
#10093 = CARTESIAN_POINT ( 'NONE',  ( -66.50057777483888799, -24.35071581493543036, 9.817618358456028815 ) ) ;
#10094 = CARTESIAN_POINT ( 'NONE',  ( -22.77861398648627400, -3.026084143414268013, 11.49999999999999645 ) ) ;
#10095 = CARTESIAN_POINT ( 'NONE',  ( 22.50852769316577096, -3.342225187595919689, -1.500000000000002220 ) ) ;
#10096 = CARTESIAN_POINT ( 'NONE',  ( 3.960462906497916435, -6.376774720514427841, 21.82884394085917279 ) ) ;
#10097 = B_SPLINE_SURFACE_WITH_KNOTS ( 'NONE', 3, 3, ( 
 ( #91363, #90868, #6128, #52317 ),
 ( #16121, #47091, #78007, #21339 ),
 ( #83251, #37081, #21839, #8519 ),
 ( #70421, #98970, #62829, #13732 ),
 ( #63328, #60442, #93743, #86139 ),
 ( #47593, #64843, #95753, #19620 ),
 ( #41988, #11510, #27250, #72431 ) ),
 .UNSPECIFIED., .F., .F., .F.,
 ( 4, 3, 4 ),
 ( 4, 4 ),
 ( 0.7945040050992245861, 0.8970133687736505657, 0.9995227324480766562 ),
 ( 0.8897200874468342846, 0.8911435658352574452 ),
 .UNSPECIFIED. ) ;
#10098 = CARTESIAN_POINT ( 'NONE',  ( 33.40725018382580913, 3.504198967030887069, -12.51830322776342008 ) ) ;
#10099 = CARTESIAN_POINT ( 'NONE',  ( -123.5895376238167103, -24.66019654487199730, 8.947790411086122830 ) ) ;
#10100 = B_SPLINE_CURVE_WITH_KNOTS ( 'NONE', 3,
 ( #75668, #84790, #62, #13769 ),
 .UNSPECIFIED., .F., .F.,
 ( 4, 4 ),
 ( 0.000000000000000000, 1.000000000000000000 ),
 .UNSPECIFIED. ) ;
#10101 = CARTESIAN_POINT ( 'NONE',  ( -4.568292318365942073, 0.3587747205144265483, 30.06720597538392425 ) ) ;
#10102 = CARTESIAN_POINT ( 'NONE',  ( -6.542779104410481494, 20.88585256366161502, 11.49999999999998934 ) ) ;
#10103 = FACE_OUTER_BOUND ( 'NONE', #50721, .T. ) ;
#10104 = CIRCLE ( 'NONE', #66843, 0.9999999999999997780 ) ;
#10105 = CARTESIAN_POINT ( 'NONE',  ( -48.97733596696294711, -25.30014187938330039, 5.627950841079814026 ) ) ;
#10106 = CARTESIAN_POINT ( 'NONE',  ( -122.5535501483336702, -24.65952944569305316, 1.056160979905708786 ) ) ;
#10107 = FACE_OUTER_BOUND ( 'NONE', #62084, .T. ) ;
#10108 = ORIENTED_EDGE ( 'NONE', *, *, #75428, .T. ) ;
#10109 = CARTESIAN_POINT ( 'NONE',  ( -20.42006937447004233, 0.3101567295262241952, 11.49999999999998934 ) ) ;
#10110 = ORIENTED_EDGE ( 'NONE', *, *, #39112, .T. ) ;
#10111 = ORIENTED_EDGE ( 'NONE', *, *, #60389, .T. ) ;
#10112 = CARTESIAN_POINT ( 'NONE',  ( -23.02147672596084149, 0.6323230698326208765, 11.49999999999998934 ) ) ;
#10113 = CARTESIAN_POINT ( 'NONE',  ( -1.318699232124953324, -5.876774720514410966, 19.74039977944280722 ) ) ;
#10114 = EDGE_LOOP ( 'NONE', ( #9899, #82309, #77769, #4438 ) ) ;
#10115 = DIRECTION ( 'NONE',  ( 0.000000000000000000, 1.000000000000000000, -0.000000000000000000 ) ) ;
#10116 = LINE ( 'NONE', #61537, #31964 ) ;
#10117 = CARTESIAN_POINT ( 'NONE',  ( -59.27315685164825965, -25.27306215940455658, 3.719512753259344606 ) ) ;
#10118 = PLANE ( 'NONE',  #41549 ) ;
#10120 = VERTEX_POINT ( 'NONE', #85294 ) ;
#10119 = CARTESIAN_POINT ( 'NONE',  ( 19.49461108348020133, 8.573440864381753457, 11.49999999999999645 ) ) ;
#10121 = CIRCLE ( 'NONE', #70017, 0.3000000000000016542 ) ;
#10122 = ORIENTED_EDGE ( 'NONE', *, *, #37403, .T. ) ;
#10123 = CARTESIAN_POINT ( 'NONE',  ( 12.24756355222007898, 18.56953561607567238, -1.500000000000002220 ) ) ;
#10124 = CARTESIAN_POINT ( 'NONE',  ( 20.62939718826500979, -0.8834638802319035866, -1.500000000000002220 ) ) ;
#10125 = VERTEX_POINT ( 'NONE', #53862 ) ;
#10126 = CARTESIAN_POINT ( 'NONE',  ( 32.40199294184733247, -6.475225279485576024, -12.82361242714783245 ) ) ;
#10127 = CARTESIAN_POINT ( 'NONE',  ( -95.55036893831936595, -24.40133493613050319, 9.663955038902802386 ) ) ;
#10128 = ORIENTED_EDGE ( 'NONE', *, *, #76248, .F. ) ;
#10129 = EDGE_CURVE ( 'NONE', #29436, #59687, #87899, .T. ) ;
#10130 = CARTESIAN_POINT ( 'NONE',  ( 15.99960863614631101, 3.577630190450212577, -27.91116951066581819 ) ) ;
#10131 = VERTEX_POINT ( 'NONE', #91402 ) ;
#10133 = EDGE_CURVE ( 'NONE', #24258, #87883, #46747, .T. ) ;
#10132 = CARTESIAN_POINT ( 'NONE',  ( -129.5228709571500758, -24.65952944569305316, 1.056160979905707675 ) ) ;
#10134 = DIRECTION ( 'NONE',  ( 0.1478094111296165969, -0.9890158633619159367, 0.000000000000000000 ) ) ;
#10135 = CARTESIAN_POINT ( 'NONE',  ( 17.12911088700535700, -11.98135219954639830, -1.500000000000002220 ) ) ;
#10136 = CARTESIAN_POINT ( 'NONE',  ( -20.59625928752216240, -7.366027188055905839, 11.49999999999999645 ) ) ;
#10137 = B_SPLINE_CURVE_WITH_KNOTS ( 'NONE', 3,
 ( #55372, #49768, #48259, #86306, #80698, #56384 ),
 .UNSPECIFIED., .F., .F.,
 ( 4, 2, 4 ),
 ( 0.000000000000000000, 0.001380764517854761279, 0.002761529035709522559 ),
 .UNSPECIFIED. ) ;
#10138 = EDGE_CURVE ( 'NONE', #25637, #81283, #7676, .T. ) ;
#10139 = CARTESIAN_POINT ( 'NONE',  ( -26.35118574718723750, -24.89279778413545330, 6.568084036181874197 ) ) ;
#10140 = CARTESIAN_POINT ( 'NONE',  ( 5.097264368844747651, -3.299463065352477908, -27.56135813788838718 ) ) ;
#10141 = CARTESIAN_POINT ( 'NONE',  ( 5.133194422563156500, 21.89913303424002677, -1.500000000000002220 ) ) ;
#10142 = EDGE_CURVE ( 'NONE', #30369, #14722, #98221, .T. ) ;
#10143 = CARTESIAN_POINT ( 'NONE',  ( 4.013313563623547964, -20.52093592976233438, 11.49999999999998934 ) ) ;
#10144 = CARTESIAN_POINT ( 'NONE',  ( -38.57583223673756123, -24.65952944569304606, 1.056160979905694131 ) ) ;
#10145 = DIRECTION ( 'NONE',  ( 0.000000000000000000, 0.000000000000000000, 1.000000000000000000 ) ) ;
#10146 = CIRCLE ( 'NONE', #23084, 19.00000000000000000 ) ;
#10147 = CARTESIAN_POINT ( 'NONE',  ( 4.931367317174526477, -5.876774720514419847, 20.61012727089847019 ) ) ;
#10148 = ORIENTED_EDGE ( 'NONE', *, *, #80046, .T. ) ;
#10149 = LOCAL_TIME ( 0, 54, 15.00000000000000000, #76682 ) ;
#10150 = EDGE_LOOP ( 'NONE', ( #25686, #44797, #91480, #5191 ) ) ;
#10151 = ORIENTED_EDGE ( 'NONE', *, *, #84216, .T. ) ;
#10152 = CARTESIAN_POINT ( 'NONE',  ( -52.55339754476869274, -23.96119346886881019, -0.6495511937831939253 ) ) ;
#10153 = ORIENTED_EDGE ( 'NONE', *, *, #94936, .T. ) ;
#10154 = CARTESIAN_POINT ( 'NONE',  ( -20.93543047832761417, 4.563121699532205255, -1.500000000000002220 ) ) ;
#10155 = AXIS2_PLACEMENT_3D ( 'NONE', #40887, #65748, #34780 ) ;
#10156 = ADVANCED_FACE ( 'NONE', ( #47246 ), #60320, .T. ) ;
#10157 = CARTESIAN_POINT ( 'NONE',  ( 1.438201247614206757, 22.34484416265529916, 11.49999999999999645 ) ) ;
#10158 = VERTEX_POINT ( 'NONE', #23379 ) ;
#10159 = DIRECTION ( 'NONE',  ( -0.09824042138329590335, 4.470611911092166224E-17, -0.9951627101165078093 ) ) ;
#10160 = CARTESIAN_POINT ( 'NONE',  ( -10.38599875782317206, -18.32754119035049101, 11.49999999999998934 ) ) ;
#10161 = CARTESIAN_POINT ( 'NONE',  ( -30.61200487207880983, -24.39002261744410660, 9.702671485061733492 ) ) ;
#10162 = CARTESIAN_POINT ( 'NONE',  ( -19.52388446859773552, -3.948942086532154061, -1.500000000000002220 ) ) ;
#10163 = CARTESIAN_POINT ( 'NONE',  ( -50.52962757068328159, -24.83644354573578639, 8.397322867130096569 ) ) ;
#10164 = CARTESIAN_POINT ( 'NONE',  ( -80.88924702628075636, -25.29534364326325857, 4.592921242107371960 ) ) ;
#10165 = CARTESIAN_POINT ( 'NONE',  ( -22.03165466229905789, 1.424673820674137614, -1.500000000000002220 ) ) ;
#10166 = CIRCLE ( 'NONE', #66891, 91.74549126261076992 ) ;
#10167 = VERTEX_POINT ( 'NONE', #562 ) ;
#10168 = CARTESIAN_POINT ( 'NONE',  ( -65.48373211964047869, -25.00182538069146432, 7.747789668545041586 ) ) ;
#10169 = CARTESIAN_POINT ( 'NONE',  ( -2.369893591381136755, -6.376774720514410077, 19.15221817653405623 ) ) ;
#10170 = CARTESIAN_POINT ( 'NONE',  ( -60.48284454307438551, -24.92564183028978775, 1.928384488918253092 ) ) ;
#10171 = CARTESIAN_POINT ( 'NONE',  ( -62.55372391215821892, -23.96169478059712787, 10.65365249895718414 ) ) ;
#10172 = FACE_OUTER_BOUND ( 'NONE', #19485, .T. ) ;
#10173 = MANIFOLD_SOLID_BREP ( 'Kes-Ekstr\X2\00fc\X0\zyon2', #87320 ) ;
#10174 = LINE ( 'NONE', #85797, #69159 ) ;
#10175 = CARTESIAN_POINT ( 'NONE',  ( -9.236746577462426444, 19.23066362772381055, -1.500000000000002220 ) ) ;
#10176 = CARTESIAN_POINT ( 'NONE',  ( -97.62287095715005592, -24.66019654487200086, 8.947790411086124607 ) ) ;
#10177 = CARTESIAN_POINT ( 'NONE',  ( -51.29687923781919068, -25.27367468601215350, 3.993462154588707680 ) ) ;
#10178 = DIRECTION ( 'NONE',  ( 0.000000000000000000, 0.000000000000000000, 1.000000000000000000 ) ) ;
#10179 = CARTESIAN_POINT ( 'NONE',  ( -81.04674198455134615, -25.14820543576475487, 6.953655299421349412 ) ) ;
#10180 = CARTESIAN_POINT ( 'NONE',  ( 21.16815136333514502, -7.790938087775149512, -1.500000000000002220 ) ) ;
#10181 = VECTOR ( 'NONE', #60239, 1000.000000000000114 ) ;
#10182 = B_SPLINE_SURFACE_WITH_KNOTS ( 'NONE', 3, 3, ( 
 ( #96230, #57185, #2892, #66292 ),
 ( #50549, #12970, #74379, #80494 ),
 ( #64809, #72398, #66796, #18587 ),
 ( #88120, #81502, #19088, #73885 ),
 ( #26213, #42455, #49563, #4877 ),
 ( #97223, #20585, #27714, #72898 ),
 ( #26712, #97715, #50059, #80999 ) ),
 .UNSPECIFIED., .F., .F., .F.,
 ( 4, 3, 4 ),
 ( 4, 4 ),
 ( 0.0004766839783823150411, 0.1029713700210899557, 0.2054660560637975864 ),
 ( 0.1895422135489633897, 0.1906423925340593462 ),
 .UNSPECIFIED. ) ;
#10183 = CARTESIAN_POINT ( 'NONE',  ( -51.52287095715008292, -24.35013146730202749, 9.818937971375104823 ) ) ;
#10184 = VERTEX_POINT ( 'NONE', #31510 ) ;
#10185 = DIRECTION ( 'NONE',  ( 1.000000000000000000, 3.773278334444166432E-23, 8.201307841325785021E-29 ) ) ;
#10186 = CARTESIAN_POINT ( 'NONE',  ( -31.52200024016721969, -23.48786465467240347, 11.44779295918255535 ) ) ;
#10187 = CARTESIAN_POINT ( 'NONE',  ( 9.421224358276909072, -17.24829524558457194, 11.49999999999999645 ) ) ;
#10188 = DIRECTION ( 'NONE',  ( 0.000000000000000000, 0.9967269304714136968, 0.08084198211964954695 ) ) ;
#10189 = DIRECTION ( 'NONE',  ( 0.06975647374412546897, 0.9975640502598241977, 0.000000000000000000 ) ) ;
#10190 = ORIENTED_EDGE ( 'NONE', *, *, #91939, .T. ) ;
#10191 = CARTESIAN_POINT ( 'NONE',  ( -29.62287095715004881, -29.50250473134420659, 10.00399446418115268 ) ) ;
#10192 = CARTESIAN_POINT ( 'NONE',  ( -124.4728709594060376, -25.40676174399605713, 8.000950338062997602 ) ) ;
#10193 = VECTOR ( 'NONE', #76237, 1000.000000000000000 ) ;
#10194 = CARTESIAN_POINT ( 'NONE',  ( 18.72495633783376334, 0.000000000000000000, 2.346898003627108320 ) ) ;
#10195 = PLANE ( 'NONE',  #68033 ) ;
#10196 = CARTESIAN_POINT ( 'NONE',  ( -32.82970096230013013, -25.05419505390707968, 2.466848186059392045 ) ) ;
#10197 = CARTESIAN_POINT ( 'NONE',  ( -68.55620429048339304, -24.64965694238574656, 8.947790433994198267 ) ) ;
#10198 = EDGE_CURVE ( 'NONE', #26695, #31094, #76466, .T. ) ;
#10199 = CARTESIAN_POINT ( 'NONE',  ( -13.31955177964949755, -14.60123061082138385, 11.49999999999998934 ) ) ;
#10200 = ORIENTED_EDGE ( 'NONE', *, *, #86589, .T. ) ;
#10201 = CIRCLE ( 'NONE', #66930, 6.600000000000001421 ) ;
#10202 = CARTESIAN_POINT ( 'NONE',  ( -19.95319933381289701, -3.276446921841525306, 11.49999999999999645 ) ) ;
#10203 = CARTESIAN_POINT ( 'NONE',  ( -7.024122139145243082, -5.876774720514408301, 19.17707164986947532 ) ) ;
#10204 = ADVANCED_FACE ( 'NONE', ( #70579 ), #94413, .T. ) ;
#10205 = ORIENTED_EDGE ( 'NONE', *, *, #11203, .T. ) ;
#10206 = CARTESIAN_POINT ( 'NONE',  ( 29.77147767949870527, 4.540774720514427543, 26.15915692125055614 ) ) ;
#10207 = CARTESIAN_POINT ( 'NONE',  ( -81.10370361591597543, -25.30541368948374981, 5.079816334721119375 ) ) ;
#10208 = LINE ( 'NONE', #63513, #49303 ) ;
#10209 = CARTESIAN_POINT ( 'NONE',  ( -115.5228709571500616, -23.47596703998600631, 11.44779298504227860 ) ) ;
#10210 = DIRECTION ( 'NONE',  ( -0.000000000000000000, 1.000000000000000000, -0.000000000000000000 ) ) ;
#10211 = CARTESIAN_POINT ( 'NONE',  ( -71.62287095715002749, -24.50216790748206108, 0.6166512839542562796 ) ) ;
#10212 = CARTESIAN_POINT ( 'NONE',  ( -16.84340083857899018, -10.81494551495373457, -1.500000000000002220 ) ) ;
#10213 = CARTESIAN_POINT ( 'NONE',  ( -99.12380231474227799, -25.27533115719222678, 4.001575131757423520 ) ) ;
#10214 = ORIENTED_EDGE ( 'NONE', *, *, #99789, .F. ) ;
#10215 = VECTOR ( 'NONE', #93293, 1000.000000000000114 ) ;
#10216 = B_SPLINE_CURVE_WITH_KNOTS ( 'NONE', 3,
 ( #34506, #19755, #50731, #57362, #3066, #81676, #64982, #41629, #94014, #88294 ),
 .UNSPECIFIED., .F., .F.,
 ( 4, 2, 2, 2, 4 ),
 ( 2.602085213965210642E-18, 0.0002062928591221676493, 0.0004125857182443326966, 0.0008251714364886473954, 0.001650342872977302380 ),
 .UNSPECIFIED. ) ;
#10218 = CARTESIAN_POINT ( 'NONE',  ( -13.89275734969026388, 0.3587747205144262708, 31.02402280011862246 ) ) ;
#10217 = APPROVAL_PERSON_ORGANIZATION ( #23158, #6561, #92679 ) ;
#10219 = CARTESIAN_POINT ( 'NONE',  ( -33.62287095715005592, -23.48783264082477373, -1.443836473390074371 ) ) ;
#10220 = CARTESIAN_POINT ( 'NONE',  ( -63.62287095715004881, -24.64965695001468404, 8.947790433994185832 ) ) ;
#10221 = CARTESIAN_POINT ( 'NONE',  ( -38.55620429048340014, -23.48783264082477373, -1.443836473390072817 ) ) ;
#10222 = CARTESIAN_POINT ( 'NONE',  ( -103.5228709571501042, -23.73907113216989373, -1.053371485793248574 ) ) ;
#10223 = FACE_OUTER_BOUND ( 'NONE', #45092, .T. ) ;
#10224 = AXIS2_PLACEMENT_3D ( 'NONE', #91806, #60388, #91311 ) ;
#10225 = CARTESIAN_POINT ( 'NONE',  ( -49.65333006503131941, -25.22444173014155666, 3.599674781239922350 ) ) ;
#10226 = ORIENTED_EDGE ( 'NONE', *, *, #16659, .T. ) ;
#10227 = CARTESIAN_POINT ( 'NONE',  ( 20.05691770114479766, 3.104179615465487707, 11.49999999999998934 ) ) ;
#10228 = VERTEX_POINT ( 'NONE', #25905 ) ;
#10229 = DIRECTION ( 'NONE',  ( -1.000000000000000000, 0.000000000000000000, -0.000000000000000000 ) ) ;
#10230 = CARTESIAN_POINT ( 'NONE',  ( -122.5228709571500332, -23.48783264082477018, -1.443836473390084807 ) ) ;
#10231 = CARTESIAN_POINT ( 'NONE',  ( -59.55362377784436489, -23.96169478059712787, 10.65365249895718769 ) ) ;
#10232 = CARTESIAN_POINT ( 'NONE',  ( -83.58953762381673869, -23.48786465467241769, 11.44779295918254469 ) ) ;
#10233 = CARTESIAN_POINT ( 'NONE',  ( -65.62287095715008434, -23.84081130438201868, 10.88220057463249191 ) ) ;
#10234 = CARTESIAN_POINT ( 'NONE',  ( -19.86647519178106691, -7.318714840676754818, 11.49999999999999645 ) ) ;
#10235 = CARTESIAN_POINT ( 'NONE',  ( -18.17467834739497690, 12.62983929299386965, 11.49999999999998934 ) ) ;
#10236 = CARTESIAN_POINT ( 'NONE',  ( -4.563637348303267949, -20.04915943051449645, 11.49999999999998934 ) ) ;
#10237 = VERTEX_POINT ( 'NONE', #17798 ) ;
#10238 = CARTESIAN_POINT ( 'NONE',  ( -116.5228709571500616, -24.64965694238575011, 8.947790433994191162 ) ) ;
#10239 = ORIENTED_EDGE ( 'NONE', *, *, #93816, .F. ) ;
#10240 = CARTESIAN_POINT ( 'NONE',  ( -54.52206328644955846, -23.48783264082476663, -1.443836473390098130 ) ) ;
#10241 = CARTESIAN_POINT ( 'NONE',  ( -110.6228709571500701, -25.00182538069145011, 7.747789668545099317 ) ) ;
#10242 = ORIENTED_EDGE ( 'NONE', *, *, #35008, .F. ) ;
#10244 = ORIENTED_EDGE ( 'NONE', *, *, #48241, .F. ) ;
#10243 = EDGE_CURVE ( 'NONE', #27531, #62142, #6910, .T. ) ;
#10245 =( BOUNDED_SURFACE ( )  B_SPLINE_SURFACE ( 3, 2, ( 
 ( #10918, #9910, #10411 ),
 ( #18522, #88544, #41371 ),
 ( #71825, #65235, #2316 ),
 ( #33246, #26647, #49495 ),
 ( #42390, #64226, #56611 ),
 ( #86534, #95154, #25638 ) ),
 .UNSPECIFIED., .F., .F., .T. ) 
 B_SPLINE_SURFACE_WITH_KNOTS ( ( 4, 2, 4 ),
 ( 3, 3 ),
 ( 0.04217399329892001364, 0.04576393237407583303, 0.04935387144923164549 ),
 ( 0.000000000000000000, 1.000000000000000000 ),
 .UNSPECIFIED. ) 
 GEOMETRIC_REPRESENTATION_ITEM ( )  RATIONAL_B_SPLINE_SURFACE ( (
 ( 1.000000000000000000, 0.7071067811865475727, 1.000000000000000000),
 ( 1.000000000000000000, 0.7325703083253984893, 1.000000000000000000),
 ( 1.000000000000000000, 0.7567337024450505600, 1.000000000000000000),
 ( 1.000000000000000000, 0.8025768260704856383, 1.000000000000000000),
 ( 1.000000000000000000, 0.8242588182985012280, 1.000000000000000000),
 ( 1.000000000000000000, 0.8446854842613638059, 1.000000000000000000) ) ) 
 REPRESENTATION_ITEM ( '' )  SURFACE ( )  );
#10246 = VERTEX_POINT ( 'NONE', #95916 ) ;
#10247 = CARTESIAN_POINT ( 'NONE',  ( -111.4287875950415554, -25.20169993477061254, 3.340150141510382031 ) ) ;
#10248 = CARTESIAN_POINT ( 'NONE',  ( -127.6228709571500275, -24.51387760970724372, 9.387446482453405849 ) ) ;
#10249 = CARTESIAN_POINT ( 'NONE',  ( 6.365284455128204399, -5.876774720514413630, 19.73076923076922640 ) ) ;
#10250 = CARTESIAN_POINT ( 'NONE',  ( -19.01758589260300525, -8.224767016273846210, -1.500000000000002220 ) ) ;
#10251 = CARTESIAN_POINT ( 'NONE',  ( 8.597998336517790108, -19.88058937513707392, 11.49999999999999645 ) ) ;
#10252 = VERTEX_POINT ( 'NONE', #41144 ) ;
#10253 = AXIS2_PLACEMENT_3D ( 'NONE', #95247, #16608, #87640 ) ;
#10254 = ADVANCED_FACE ( 'NONE', ( #1072 ), #3087, .T. ) ;
#10255 = CARTESIAN_POINT ( 'NONE',  ( -60.52287095715007581, -24.92604778743751481, 8.074972756821495068 ) ) ;
#10256 = CARTESIAN_POINT ( 'NONE',  ( 33.96422015159436114, -0.3587747205144265483, -7.233236000911337449 ) ) ;
#10257 = CARTESIAN_POINT ( 'NONE',  ( 21.16571772479873204, -7.350578744355993344, 11.49999999999998934 ) ) ;
#10258 = EDGE_CURVE ( 'NONE', #89740, #89130, #79843, .T. ) ;
#10259 = CARTESIAN_POINT ( 'NONE',  ( 3.138110291115776995, 11.54688212118755075, 3.549999999999999822 ) ) ;
#10260 = CARTESIAN_POINT ( 'NONE',  ( -102.5228709571500758, -24.51387760970725438, 9.387446482453409402 ) ) ;
#10261 = ORIENTED_EDGE ( 'NONE', *, *, #68061, .F. ) ;
#10262 = CYLINDRICAL_SURFACE ( 'NONE', #74467, 1.836000000000000743 ) ;
#10263 = CARTESIAN_POINT ( 'NONE',  ( 12.28518416766336507, -5.152774720514428530, -26.38359849988869144 ) ) ;
#10264 = VECTOR ( 'NONE', #43421, 1000.000000000000000 ) ;
#10265 = EDGE_CURVE ( 'NONE', #83981, #84492, #96970, .T. ) ;
#10266 = VERTEX_POINT ( 'NONE', #33518 ) ;
#10267 = ADVANCED_FACE ( 'NONE', ( #87809 ), #48254, .F. ) ;
#10268 = ORIENTED_EDGE ( 'NONE', *, *, #74509, .F. ) ;
#10269 = CARTESIAN_POINT ( 'NONE',  ( -71.22287095715005023, -23.47596703998600276, 11.44779298504227860 ) ) ;
#10270 = ORIENTED_EDGE ( 'NONE', *, *, #14986, .T. ) ;
#10271 = CARTESIAN_POINT ( 'NONE',  ( -51.52764846858840997, -29.50249643624320584, 6.187563540074810575 ) ) ;
#10272 = CARTESIAN_POINT ( 'NONE',  ( -21.08002519818654363, -2.465602145356518893, -1.500000000000002220 ) ) ;
#10273 = ORIENTED_EDGE ( 'NONE', *, *, #45664, .T. ) ;
#10274 = DIRECTION ( 'NONE',  ( 0.000000000000000000, 0.9999999999976377785, 2.173523156925979975E-06 ) ) ;
#10275 = CARTESIAN_POINT ( 'NONE',  ( -13.95179422449595208, 16.79422078803934326, 11.49999999999998934 ) ) ;
#10276 = CARTESIAN_POINT ( 'NONE',  ( -103.5113892122844277, -24.51419770103155926, 9.386484678747176957 ) ) ;
#10277 = PLANE ( 'NONE',  #77711 ) ;
#10278 = DIRECTION ( 'NONE',  ( -0.000000000000000000, 1.000000000000000000, -0.000000000000000000 ) ) ;
#10279 = CARTESIAN_POINT ( 'NONE',  ( 15.24057855588860377, 15.72025634131890470, -1.500000000000002220 ) ) ;
#10280 = LINE ( 'NONE', #26513, #93312 ) ;
#10281 = ORIENTED_EDGE ( 'NONE', *, *, #48984, .T. ) ;
#10282 = EDGE_CURVE ( 'NONE', #9142, #59928, #70373, .T. ) ;
#10283 = DIRECTION ( 'NONE',  ( -3.773278334453080206E-23, 0.9999999999976377785, 2.173523156925979975E-06 ) ) ;
#10284 = CARTESIAN_POINT ( 'NONE',  ( -48.89385731722059347, -25.26337357799507544, 6.392748942997004136 ) ) ;
#10285 = ORIENTED_EDGE ( 'NONE', *, *, #29767, .T. ) ;
#10286 = ORIENTED_EDGE ( 'NONE', *, *, #94882, .T. ) ;
#10287 = AXIS2_PLACEMENT_3D ( 'NONE', #41245, #175, #54971 ) ;
#10288 = ORIENTED_EDGE ( 'NONE', *, *, #62222, .F. ) ;
#10289 = CARTESIAN_POINT ( 'NONE',  ( -58.58953762381673158, -24.64965694238407323, 8.947790433994656567 ) ) ;
#10290 = CARTESIAN_POINT ( 'NONE',  ( -31.24388727629347429, -25.01990435277411606, 2.279866971661216546 ) ) ;
#10291 = CARTESIAN_POINT ( 'NONE',  ( -10.85727797829764185, 18.24708236899833835, 11.49999999999998934 ) ) ;
#10292 = CARTESIAN_POINT ( 'NONE',  ( -125.5895376238167245, -25.00182538069145721, 7.747789668545099317 ) ) ;
#10293 = DIRECTION ( 'NONE',  ( 0.000000000000000000, 0.9999999999976377785, 2.173523156925979975E-06 ) ) ;
#10294 = CARTESIAN_POINT ( 'NONE',  ( -10.21384395349174490, 3.316774720514427344, 29.49402280011862487 ) ) ;
#10295 = CARTESIAN_POINT ( 'NONE',  ( -118.5228709571500758, -29.50247984919015209, -1.443849546365046699 ) ) ;
#10297 = CARTESIAN_POINT ( 'NONE',  ( -19.30698013599780083, -2.078282243779251637, -1.500000000000002220 ) ) ;
#10296 = AXIS2_PLACEMENT_3D ( 'NONE', #72866, #87581, #34300 ) ;
#10298 = CARTESIAN_POINT ( 'NONE',  ( -117.5885002923016884, -24.51419770103158768, 9.386484678747164523 ) ) ;
#10299 = ORIENTED_EDGE ( 'NONE', *, *, #78709, .F. ) ;
#10300 = CARTESIAN_POINT ( 'NONE',  ( 13.27039818535887505, -14.28956163997708906, 11.49999999999999645 ) ) ;
#10301 = CARTESIAN_POINT ( 'NONE',  ( 31.63608488009069575, -3.478648800329905644, 27.34773273846989738 ) ) ;
#10302 = AXIS2_PLACEMENT_3D ( 'NONE', #22747, #30878, #47118 ) ;
#10303 = DIRECTION ( 'NONE',  ( -3.773278334453079618E-23, 0.9999999999976377785, 2.173523156925979975E-06 ) ) ;
#10304 = ADVANCED_FACE ( 'NONE', ( #49267 ), #93908, .T. ) ;
#10305 = VERTEX_POINT ( 'NONE', #63492 ) ;
#10306 = CARTESIAN_POINT ( 'NONE',  ( 4.400426145423703694, -6.376774720514426065, 21.64763382324305852 ) ) ;
#10307 = CARTESIAN_POINT ( 'NONE',  ( -89.58586318894654710, -24.51314013834317151, 0.6176544820404251679 ) ) ;
#10308 = DIRECTION ( 'NONE',  ( -0.000000000000000000, 1.000000000000000000, -0.000000000000000000 ) ) ;
#10309 = EDGE_CURVE ( 'NONE', #27242, #75398, #22012, .T. ) ;
#10310 = CARTESIAN_POINT ( 'NONE',  ( -117.6228709571500559, -29.50250786944525672, 11.44777988621622811 ) ) ;
#10311 = CARTESIAN_POINT ( 'NONE',  ( -10.66912846187372210, -16.51573522771486324, 11.49999999999998934 ) ) ;
#10312 = ORIENTED_EDGE ( 'NONE', *, *, #89855, .F. ) ;
#10313 = CARTESIAN_POINT ( 'NONE',  ( -8.063330319165405768, -10.15233964170348457, 1.310587897985993733 ) ) ;
#10314 = CARTESIAN_POINT ( 'NONE',  ( 17.26854690438276307, -15.35948741044508559, -1.500000000000002220 ) ) ;
#10315 = APPROVAL_DATE_TIME ( #33659, #53771 ) ;
#10316 = EDGE_CURVE ( 'NONE', #45280, #8769, #9807, .T. ) ;
#10317 = CARTESIAN_POINT ( 'NONE',  ( 3.249631081431332280, -6.376774720514424288, 21.24682042713427776 ) ) ;
#10318 = DIRECTION ( 'NONE',  ( 1.000000000000000000, 3.773278334444167608E-23, 8.201307833595939069E-29 ) ) ;
#10319 = CARTESIAN_POINT ( 'NONE',  ( -79.52287095715006160, -24.66019654487199375, 8.947790411086122830 ) ) ;
#10320 = CARTESIAN_POINT ( 'NONE',  ( -97.54989192072140725, -24.35071581493543746, 9.817618358456025263 ) ) ;
#10321 = CARTESIAN_POINT ( 'NONE',  ( -80.90972592788718032, -25.29489613318244423, 6.057562805997258160 ) ) ;
#10322 = CARTESIAN_POINT ( 'NONE',  ( -43.62287095715003460, -23.73934037231756733, 11.05740245334329153 ) ) ;
#10323 = CARTESIAN_POINT ( 'NONE',  ( -68.62287095715005592, -29.50250243563736774, 8.947779886222143375 ) ) ;
#10324 = CARTESIAN_POINT ( 'NONE',  ( -50.62287095715007013, -24.62226745350439572, 0.9660975649728152925 ) ) ;
#10325 = CARTESIAN_POINT ( 'NONE',  ( -1.646307629438301667, 19.86461321233117872, -1.500000000000002220 ) ) ;
#10326 = EDGE_CURVE ( 'NONE', #21001, #41837, #10684, .T. ) ;
#10327 = VECTOR ( 'NONE', #18514, 1000.000000000000000 ) ;
#10328 = CARTESIAN_POINT ( 'NONE',  ( -75.53594935777978492, -24.92592662359561118, 8.075495903018000021 ) ) ;
#10329 = CARTESIAN_POINT ( 'NONE',  ( -12.84220538718065185, 15.17226672225704398, -1.500000000000002220 ) ) ;
#10330 = ORIENTED_EDGE ( 'NONE', *, *, #88660, .F. ) ;
#10331 = CARTESIAN_POINT ( 'NONE',  ( -90.70643032827079821, -25.32958289424478338, 5.296252972553156191 ) ) ;
#10332 = AXIS2_PLACEMENT_3D ( 'NONE', #65367, #26775, #26275 ) ;
#10333 = CARTESIAN_POINT ( 'NONE',  ( -125.5228709571501184, -23.84047902841604127, -0.8780736468305687659 ) ) ;
#10334 = CARTESIAN_POINT ( 'NONE',  ( 30.53060340732036337, -2.682774720514426559, -8.442346167188910400 ) ) ;
#10335 = CARTESIAN_POINT ( 'NONE',  ( 7.822518687389895753, -3.316774720514091168, -28.18023264461383448 ) ) ;
#10336 = CARTESIAN_POINT ( 'NONE',  ( -11.07951500695464553, -17.62175104703424466, 11.49999999999999645 ) ) ;
#10337 = CARTESIAN_POINT ( 'NONE',  ( -6.775140224358976226, -5.876774720514408301, 19.14743589743590846 ) ) ;
#10338 = CC_DESIGN_PERSON_AND_ORGANIZATION_ASSIGNMENT ( #86935, #2718, ( #44230 ) ) ;
#10339 = CARTESIAN_POINT ( 'NONE',  ( -50.40445135320380388, -25.18492896333868103, 3.293943116708552221 ) ) ;
#10340 = CARTESIAN_POINT ( 'NONE',  ( 21.15473741701296362, -8.388382055385795510, 11.49999999999999645 ) ) ;
#10341 = ORIENTED_EDGE ( 'NONE', *, *, #68339, .F. ) ;
#10342 = CARTESIAN_POINT ( 'NONE',  ( 30.53060340732036337, -5.099191132445380248, -0.7211848363580904975 ) ) ;
#10343 = CARTESIAN_POINT ( 'NONE',  ( 0.000000000000000000, -2.056774720514426669, 0.000000000000000000 ) ) ;
#10344 = ORIENTED_EDGE ( 'NONE', *, *, #96217, .T. ) ;
#10345 = CARTESIAN_POINT ( 'NONE',  ( 15.73562052650688514, -12.66937975264744587, 11.49999999999998934 ) ) ;
#10346 = CARTESIAN_POINT ( 'NONE',  ( 7.343377932919765705, -6.376774720514422512, 21.31293098237466310 ) ) ;
#10347 = CARTESIAN_POINT ( 'NONE',  ( -41.03061461742554883, -25.30559429607382782, 4.924307031744522334 ) ) ;
#10348 = CARTESIAN_POINT ( 'NONE',  ( -100.6228709571500559, -25.00158670708909625, 2.256160236439166411 ) ) ;
#10349 = VERTEX_POINT ( 'NONE', #26410 ) ;
#10350 = DIRECTION ( 'NONE',  ( -0.000000000000000000, 1.000000000000000000, -0.000000000000000000 ) ) ;
#10351 = CARTESIAN_POINT ( 'NONE',  ( -10.18932761084327865, 5.341047792237469949, 29.75743496038930758 ) ) ;
#10352 = CARTESIAN_POINT ( 'NONE',  ( -6.099057486122481997, -19.05896565686126110, -1.500000000000002220 ) ) ;
#10353 = CARTESIAN_POINT ( 'NONE',  ( 15.12549221760053086, 14.48511125727034177, 11.49999999999999645 ) ) ;
#10354 = CARTESIAN_POINT ( 'NONE',  ( 5.271800844963591359, -0.3587747205143965168, -28.56638892015329745 ) ) ;
#10355 = DIRECTION ( 'NONE',  ( 0.000000000000000000, 0.000000000000000000, -1.000000000000000000 ) ) ;
#10356 = CARTESIAN_POINT ( 'NONE',  ( 13.08019894233326319, 17.74467248152726384, 11.49999999999998934 ) ) ;
#10357 = CARTESIAN_POINT ( 'NONE',  ( -42.62287095715004881, -24.64898659630367561, 1.056161002820819261 ) ) ;
#10358 = VERTEX_POINT ( 'NONE', #1580 ) ;
#10359 = CARTESIAN_POINT ( 'NONE',  ( -82.52287095715006160, -29.50250786944525672, 11.44777988621623521 ) ) ;
#10360 = CARTESIAN_POINT ( 'NONE',  ( -49.54012794836013001, -25.18440211203497725, 3.796733314902499767 ) ) ;
#10361 = CARTESIAN_POINT ( 'NONE',  ( -74.62287095715005592, -24.64965695001467694, 8.947790433994184056 ) ) ;
#10362 = ORIENTED_EDGE ( 'NONE', *, *, #83422, .F. ) ;
#10363 = FACE_OUTER_BOUND ( 'NONE', #49297, .T. ) ;
#10364 = ORIENTED_EDGE ( 'NONE', *, *, #52752, .F. ) ;
#10365 = ORIENTED_EDGE ( 'NONE', *, *, #38650, .T. ) ;
#10366 = ADVANCED_FACE ( 'NONE', ( #32517 ), #71591, .T. ) ;
#10367 = DIRECTION ( 'NONE',  ( -0.000000000000000000, -1.000000000000000000, -0.000000000000000000 ) ) ;
#10368 = CARTESIAN_POINT ( 'NONE',  ( 2.449489742783179214, -16.94322527948557422, 2.499999999999999112 ) ) ;
#10369 = CARTESIAN_POINT ( 'NONE',  ( -4.930333147521421822, -6.376774720514410077, 19.46306892155547530 ) ) ;
#10370 = CARTESIAN_POINT ( 'NONE',  ( 18.67943556539783856, 8.552475402716291697, -1.500000000000002220 ) ) ;
#10371 = ORIENTED_EDGE ( 'NONE', *, *, #34119, .F. ) ;
#10372 = LINE ( 'NONE', #95613, #18648 ) ;
#10373 = CARTESIAN_POINT ( 'NONE',  ( -38.52287095715006870, -24.65952944569303895, 1.056160979905691910 ) ) ;
#10374 = CARTESIAN_POINT ( 'NONE',  ( -41.52287095715007581, -24.50321055353804667, 9.387540953477524042 ) ) ;
#10375 = CARTESIAN_POINT ( 'NONE',  ( 7.190675130926929448, -21.12231643677837312, 11.49999999999998934 ) ) ;
#10376 = B_SPLINE_CURVE_WITH_KNOTS ( 'NONE', 3,
 ( #68290, #59692, #92607, #99706, #98223, #61195, #92114, #28731 ),
 .UNSPECIFIED., .F., .F.,
 ( 4, 2, 2, 4 ),
 ( 0.000000000000000000, 0.0003937098746455595455, 0.0007874197492911190911, 0.001574839498582238182 ),
 .UNSPECIFIED. ) ;
#10377 = LINE ( 'NONE', #94107, #44830 ) ;
#10378 = CARTESIAN_POINT ( 'NONE',  ( 0.7051282051282083962, -5.876774720514426953, 21.75000000000000000 ) ) ;
#10379 = EDGE_LOOP ( 'NONE', ( #47807, #69557, #40344, #5525 ) ) ;
#10380 = CARTESIAN_POINT ( 'NONE',  ( 33.55334901790278224, -3.914284326356132659, -11.46592497341461758 ) ) ;
#10381 = LINE ( 'NONE', #71291, #26421 ) ;
#10382 = EDGE_CURVE ( 'NONE', #91571, #78143, #8518, .T. ) ;
#10383 = CARTESIAN_POINT ( 'NONE',  ( -14.93763623016880082, -14.57113377498261997, 11.49999999999998934 ) ) ;
#10384 = ADVANCED_FACE ( 'NONE', ( #65997 ), #58369, .F. ) ;
#10385 = EDGE_LOOP ( 'NONE', ( #15638, #75770, #94801, #53958 ) ) ;
#10387 = ORIENTED_EDGE ( 'NONE', *, *, #28575, .F. ) ;
#10386 = CARTESIAN_POINT ( 'NONE',  ( -0.3544984435505275644, -6.376774720514408301, 19.15251819062245531 ) ) ;
#10388 = ORIENTED_EDGE ( 'NONE', *, *, #10614, .F. ) ;
#10389 = CARTESIAN_POINT ( 'NONE',  ( -69.62994293422308090, -25.25935311477814693, 7.382559191806408627 ) ) ;
#10390 = CARTESIAN_POINT ( 'NONE',  ( -20.88184962559319402, -2.832954952542597660, -1.500000000000002220 ) ) ;
#10391 = ORIENTED_EDGE ( 'NONE', *, *, #83780, .T. ) ;
#10392 = CARTESIAN_POINT ( 'NONE',  ( 0.3910256410256418569, -6.376774720514420736, 20.67377804487180271 ) ) ;
#10393 = DIRECTION ( 'NONE',  ( 0.000000000000000000, -1.000000000000000000, 0.000000000000000000 ) ) ;
#10394 = CARTESIAN_POINT ( 'NONE',  ( 6.499999999999992895, 1.999999999999998668, 3.499999999999999112 ) ) ;
#10395 = CARTESIAN_POINT ( 'NONE',  ( -86.59502610026325442, -23.96169478059713498, 10.65365249895717881 ) ) ;
#10396 = CARTESIAN_POINT ( 'NONE',  ( -59.59291227190924189, -24.15543982623906416, -0.2315651400026668416 ) ) ;
#10397 = CARTESIAN_POINT ( 'NONE',  ( -19.97641003480726241, 8.421946895145676848, -1.500000000000002220 ) ) ;
#10398 = DIRECTION ( 'NONE',  ( 0.000000000000000000, 7.440411327181627631E-14, -1.000000000000000000 ) ) ;
#10400 = ORIENTED_EDGE ( 'NONE', *, *, #47148, .T. ) ;
#10399 = CARTESIAN_POINT ( 'NONE',  ( 18.07686251855496096, -12.98574554580779861, 11.49999999999999645 ) ) ;
#10401 = ADVANCED_FACE ( 'NONE', ( #73092 ), #74086, .F. ) ;
#10402 = LINE ( 'NONE', #56602, #79380 ) ;
#10403 = CARTESIAN_POINT ( 'NONE',  ( 21.97688922017995594, 1.477225279485574028, -18.55878510778118340 ) ) ;
#10404 = CARTESIAN_POINT ( 'NONE',  ( -70.35895856474229504, -25.30161620421289470, 5.313173632321669615 ) ) ;
#10405 = EDGE_LOOP ( 'NONE', ( #37519, #78111, #33704, #20880 ) ) ;
#10406 = VECTOR ( 'NONE', #82607, 1000.000000000000000 ) ;
#10408 = ORIENTED_EDGE ( 'NONE', *, *, #42828, .T. ) ;
#10407 = LINE ( 'NONE', #26134, #39421 ) ;
#10409 = VECTOR ( 'NONE', #52928, 1000.000000000000114 ) ;
#10410 = ORIENTED_EDGE ( 'NONE', *, *, #88218, .F. ) ;
#10411 = CARTESIAN_POINT ( 'NONE',  ( 31.13513474936813807, -4.540774720514427543, 3.331262582247328741 ) ) ;
#10412 = CARTESIAN_POINT ( 'NONE',  ( 19.84801528777503776, 3.447069022702595742, -1.500000000000002220 ) ) ;
#10413 = LINE ( 'NONE', #96160, #53861 ) ;
#10414 = ORIENTED_EDGE ( 'NONE', *, *, #34564, .F. ) ;
#10415 = CARTESIAN_POINT ( 'NONE',  ( -130.5728709571500588, -25.05579301371511747, 7.915991903154699472 ) ) ;
#10416 = CARTESIAN_POINT ( 'NONE',  ( -21.16225983376422448, 7.283793490815352989, -1.500000000000002220 ) ) ;
#10417 = EDGE_LOOP ( 'NONE', ( #7144, #34230, #51084, #4510 ) ) ;
#10418 = ORIENTED_EDGE ( 'NONE', *, *, #2962, .F. ) ;
#10419 = CYLINDRICAL_SURFACE ( 'NONE', #66103, 1.699999999999998401 ) ;
#10420 = CARTESIAN_POINT ( 'NONE',  ( -101.6367508631515477, -23.48786465467240703, 11.44779295918254114 ) ) ;
#10421 = CARTESIAN_POINT ( 'NONE',  ( -67.62287095715005592, -24.64965695001468404, 8.947790433994184056 ) ) ;
#10422 = CARTESIAN_POINT ( 'NONE',  ( -56.52287095715006870, -29.50250243563736774, 8.947779886222145151 ) ) ;
#10423 = CARTESIAN_POINT ( 'NONE',  ( -63.91869748439341237, -24.82959736273286921, 8.370978854367633559 ) ) ;
#10424 = ADVANCED_FACE ( 'NONE', ( #37883 ), #42154, .F. ) ;
#10425 = CARTESIAN_POINT ( 'NONE',  ( -6.824658503225996320, 18.35159230250476270, -1.500000000000002220 ) ) ;
#10426 = DIRECTION ( 'NONE',  ( 0.000000000000000000, 0.000000000000000000, 1.000000000000000000 ) ) ;
#10427 = ORIENTED_EDGE ( 'NONE', *, *, #25961, .T. ) ;
#10428 = CARTESIAN_POINT ( 'NONE',  ( -15.45034113870702441, -14.97902827799142500, -1.500000000000002220 ) ) ;
#10429 = DIRECTION ( 'NONE',  ( -1.000000000000000000, 0.000000000000000000, 1.250865172912931245E-15 ) ) ;
#10430 = CARTESIAN_POINT ( 'NONE',  ( -80.43221577628075636, -25.31572646011074212, 4.967019755498037981 ) ) ;
#10431 = CARTESIAN_POINT ( 'NONE',  ( -1.358974358974355257, -6.376774720514427841, 21.75000000000000711 ) ) ;
#10432 = LINE ( 'NONE', #96670, #74736 ) ;
#10433 = CARTESIAN_POINT ( 'NONE',  ( -22.24355531667433539, 5.575215412481045796, -1.500000000000002220 ) ) ;
#10434 = ADVANCED_FACE ( 'NONE', ( #21637 ), #68338, .T. ) ;
#10435 = DATE_TIME_ROLE ( 'classification_date' ) ;
#10436 = CARTESIAN_POINT ( 'NONE',  ( -89.81226385320383088, -25.27880950044345454, 5.947789066509452383 ) ) ;
#10437 = CARTESIAN_POINT ( 'NONE',  ( -53.63293900283483140, -24.34968618360933590, 0.1864209137778786440 ) ) ;
#10438 = CARTESIAN_POINT ( 'NONE',  ( -19.68739882612603864, 4.164723872966736629, 11.49999999999999645 ) ) ;
#10439 = CARTESIAN_POINT ( 'NONE',  ( -40.62287095715004170, -25.00182538069145011, 7.747789668545099317 ) ) ;
#10440 = DIRECTION ( 'NONE',  ( 0.000000000000000000, -1.000000000000000000, 0.000000000000000000 ) ) ;
#10441 = DIRECTION ( 'NONE',  ( -3.773278334453079030E-23, 0.9999999999976377785, 2.173523156925979128E-06 ) ) ;
#10442 = DIRECTION ( 'NONE',  ( 0.000000000000000000, 0.9999999999976377785, 2.173523156925979975E-06 ) ) ;
#10443 = B_SPLINE_CURVE_WITH_KNOTS ( 'NONE', 3,
 ( #58760, #42056, #50159, #43541 ),
 .UNSPECIFIED., .F., .F.,
 ( 4, 4 ),
 ( 0.000000000000000000, 0.0004434240296263077972 ),
 .UNSPECIFIED. ) ;
#10444 = CARTESIAN_POINT ( 'NONE',  ( 15.32643653063178668, 3.582999323269832725, -27.14485409495428314 ) ) ;
#10445 = CARTESIAN_POINT ( 'NONE',  ( -15.99800673754971037, 11.70972097625665675, -1.500000000000002220 ) ) ;
#10446 = CARTESIAN_POINT ( 'NONE',  ( -6.720452724358975338, -6.376774720514411854, 19.46153846153846700 ) ) ;
#10447 = CARTESIAN_POINT ( 'NONE',  ( -2.340448316220725467, 19.49152957720520618, -1.500000000000002220 ) ) ;
#10448 = CARTESIAN_POINT ( 'NONE',  ( -42.56928426289123735, -23.48783264082477373, -1.443836473390076147 ) ) ;
#10449 = CARTESIAN_POINT ( 'NONE',  ( -58.52287095715006160, -23.48786465467241058, 11.44779295918254824 ) ) ;
#10450 = PERSON_AND_ORGANIZATION ( #85150, #50564 ) ;
#10451 = CARTESIAN_POINT ( 'NONE',  ( -60.52287095715007581, -24.82576562948885623, 8.398263436605553522 ) ) ;
#10452 = CARTESIAN_POINT ( 'NONE',  ( -39.15118670841629012, -25.30439178025131142, 4.799404196304809744 ) ) ;
#10453 = CARTESIAN_POINT ( 'NONE',  ( -18.12278953325389708, -9.833843834435361586, 11.49999999999999645 ) ) ;
#10454 = FACE_OUTER_BOUND ( 'NONE', #72545, .T. ) ;
#10455 = B_SPLINE_CURVE_WITH_KNOTS ( 'NONE', 3,
 ( #7476, #44052, #74984, #29819 ),
 .UNSPECIFIED., .F., .F.,
 ( 4, 4 ),
 ( 0.000000000000000000, 9.999999999998897304E-05 ),
 .UNSPECIFIED. ) ;
#10456 = AXIS2_PLACEMENT_3D ( 'NONE', #77806, #39263, #39760 ) ;
#10457 = EDGE_CURVE ( 'NONE', #59016, #11739, #14659, .T. ) ;
#10458 = CARTESIAN_POINT ( 'NONE',  ( 1.949999999999999956, -0.1925000000000001155, -0.1925000000000000600 ) ) ;
#10459 = CARTESIAN_POINT ( 'NONE',  ( -4.885077187424587741, 22.05487924249641551, 11.49999999999999645 ) ) ;
#10460 = ORIENTED_EDGE ( 'NONE', *, *, #37901, .T. ) ;
#10461 = CARTESIAN_POINT ( 'NONE',  ( -53.55620429048339304, -24.65952944569304606, 1.056160979905692576 ) ) ;
#10462 = CARTESIAN_POINT ( 'NONE',  ( -51.07385796617099061, -25.30408280926228670, 4.469399184940273884 ) ) ;
#10463 = CARTESIAN_POINT ( 'NONE',  ( -128.6228709571500417, -24.66019654487200441, 8.947790411086121054 ) ) ;
#10464 = CARTESIAN_POINT ( 'NONE',  ( -110.5228709571500474, -24.52232992886363050, 0.6492154411906037037 ) ) ;
#10465 = AXIS2_PLACEMENT_3D ( 'NONE', #64828, #41459, #82012 ) ;
#10466 = CARTESIAN_POINT ( 'NONE',  ( 25.83488407601165093, 4.132774720514426292, -11.31196583263648137 ) ) ;
#10467 = EDGE_CURVE ( 'NONE', #34684, #15382, #65497, .T. ) ;
#10468 = EDGE_CURVE ( 'NONE', #49598, #41774, #69102, .T. ) ;
#10469 = ORIENTED_EDGE ( 'NONE', *, *, #68209, .F. ) ;
#10470 = LINE ( 'NONE', #12468, #51725 ) ;
#10471 = CARTESIAN_POINT ( 'NONE',  ( -22.55118551311790753, 3.560990644294375063, 11.49999999999998934 ) ) ;
#10472 = CARTESIAN_POINT ( 'NONE',  ( -111.3164332061762991, -25.26394802776237114, 3.995147376310239196 ) ) ;
#10473 = CARTESIAN_POINT ( 'NONE',  ( -92.62287095715005592, -23.47593901973091235, -1.443836447539002865 ) ) ;
#10474 = CARTESIAN_POINT ( 'NONE',  ( -63.64766708060687250, -23.73791477778912196, 11.05961554403170766 ) ) ;
#10475 = CARTESIAN_POINT ( 'NONE',  ( 19.74966320730700176, -10.79507447929251107, 11.49999999999999645 ) ) ;
#10476 = ORIENTED_EDGE ( 'NONE', *, *, #68896, .T. ) ;
#10477 = CARTESIAN_POINT ( 'NONE',  ( -5.366453405989236813, 0.000000000000000000, 0.000000000000000000 ) ) ;
#10478 = CARTESIAN_POINT ( 'NONE',  ( -21.86317675896206225, -2.224439152981679602, -1.500000000000002220 ) ) ;
#10479 = CARTESIAN_POINT ( 'NONE',  ( -54.62287095715006302, -23.73907113216990439, -1.053371485793231921 ) ) ;
#10480 = LINE ( 'NONE', #70386, #31670 ) ;
#10481 = LINE ( 'NONE', #81998, #15199 ) ;
#10482 = ORIENTED_EDGE ( 'NONE', *, *, #96079, .F. ) ;
#10483 = FACE_OUTER_BOUND ( 'NONE', #25588, .T. ) ;
#10484 = FACE_OUTER_BOUND ( 'NONE', #57597, .T. ) ;
#10485 = ORIENTED_EDGE ( 'NONE', *, *, #66526, .F. ) ;
#10486 = CARTESIAN_POINT ( 'NONE',  ( -54.50803268341093144, -23.96169478059712787, 10.65365249895718947 ) ) ;
#10487 = CARTESIAN_POINT ( 'NONE',  ( 1.819314030819549233, -20.42850443921780013, 11.49999999999998934 ) ) ;
#10488 = EDGE_LOOP ( 'NONE', ( #64313, #79865, #43674, #63053, #45254, #16705, #1316, #73928, #29473, #67952, #52929 ) ) ;
#10489 = ORIENTED_EDGE ( 'NONE', *, *, #27804, .F. ) ;
#10490 = ORIENTED_EDGE ( 'NONE', *, *, #27894, .T. ) ;
#10491 = ORIENTED_EDGE ( 'NONE', *, *, #14791, .F. ) ;
#10492 = ADVANCED_FACE ( 'NONE', ( #57877 ), #37390, .T. ) ;
#10493 = CARTESIAN_POINT ( 'NONE',  ( -71.62287095715005592, -23.47593901973091235, -1.443836447539006196 ) ) ;
#10494 = CARTESIAN_POINT ( 'NONE',  ( 22.67273400128462058, 4.441195646929153362, -1.500000000000002220 ) ) ;
#10495 = CARTESIAN_POINT ( 'NONE',  ( -104.5495314845192496, -24.51419770103158768, 9.386484678747166299 ) ) ;
#10496 = CARTESIAN_POINT ( 'NONE',  ( -20.10423522397153562, 3.301153050299447056, -1.500000000000002220 ) ) ;
#10497 = ORIENTED_EDGE ( 'NONE', *, *, #40966, .T. ) ;
#10498 = CARTESIAN_POINT ( 'NONE',  ( -71.37981187788743398, -25.12275311710066461, 7.103969935991345075 ) ) ;
#10499 = PLANE ( 'NONE',  #14133 ) ;
#10500 = CARTESIAN_POINT ( 'NONE',  ( -113.5228709571500616, -23.47593901973090524, -1.443836447538996204 ) ) ;
#10501 = CARTESIAN_POINT ( 'NONE',  ( 4.593956459244529889, -6.376774720514410077, 19.29001220640957115 ) ) ;
#10502 = VERTEX_POINT ( 'NONE', #12167 ) ;
#10503 = CARTESIAN_POINT ( 'NONE',  ( -108.8968792378191921, -29.50249817218807635, 6.986241424688308221 ) ) ;
#10504 = CARTESIAN_POINT ( 'NONE',  ( -49.74369414166532977, -25.31573832230478516, 4.940877928549117115 ) ) ;
#10505 = VECTOR ( 'NONE', #32915, 1000.000000000000114 ) ;
#10506 = EDGE_LOOP ( 'NONE', ( #48416, #17574, #18828, #98353 ) ) ;
#10507 = CARTESIAN_POINT ( 'NONE',  ( -12.88759680649768136, 16.30154091734715749, 11.49999999999998934 ) ) ;
#10508 = EDGE_CURVE ( 'NONE', #67048, #85400, #58360, .T. ) ;
#10509 = ORIENTED_EDGE ( 'NONE', *, *, #94259, .F. ) ;
#10511 = ORIENTED_EDGE ( 'NONE', *, *, #36921, .F. ) ;
#10510 = CARTESIAN_POINT ( 'NONE',  ( -125.5894646780946999, -24.63355581998386512, 0.9682620441944075340 ) ) ;
#10512 = ADVANCED_FACE ( 'NONE', ( #53123 ), #88815, .F. ) ;
#10513 = B_SPLINE_CURVE_WITH_KNOTS ( 'NONE', 3,
 ( #48365, #41249, #72205, #90411 ),
 .UNSPECIFIED., .F., .F.,
 ( 4, 4 ),
 ( 2.907410163773248763E-09, 0.002226547977040467356 ),
 .UNSPECIFIED. ) ;
#10514 = CARTESIAN_POINT ( 'NONE',  ( -83.62287095715005592, -29.50250786944525672, 11.44777988621623521 ) ) ;
#10515 = DIRECTION ( 'NONE',  ( 2.352173255807804438E-16, -2.352173255807796056E-16, -1.000000000000000000 ) ) ;
#10516 = ORIENTED_EDGE ( 'NONE', *, *, #5204, .T. ) ;
#10517 = ORIENTED_EDGE ( 'NONE', *, *, #29709, .F. ) ;
#10518 = CARTESIAN_POINT ( 'NONE',  ( -6.369015873774380943, -5.876774720514413630, 19.23384392940399934 ) ) ;
#10519 = DIRECTION ( 'NONE',  ( 0.000000000000000000, 0.000000000000000000, -1.000000000000000000 ) ) ;
#10520 = B_SPLINE_CURVE_WITH_KNOTS ( 'NONE', 3,
 ( #10348, #80865, #41303, #72264, #30817, #2751, #11352, #33692 ),
 .UNSPECIFIED., .F., .F.,
 ( 4, 2, 2, 4 ),
 ( -0.001224873891641419573, -0.0002244903592271039420, 0.0007758931731872116891, 0.002776660238015838614 ),
 .UNSPECIFIED. ) ;
#10521 = CARTESIAN_POINT ( 'NONE',  ( -46.52287095715006160, -23.48786465467241058, 11.44779295918255002 ) ) ;
#10523 = ORIENTED_EDGE ( 'NONE', *, *, #14542, .F. ) ;
#10522 = CARTESIAN_POINT ( 'NONE',  ( 14.91618686576236108, -16.25093855066790738, 11.49999999999999645 ) ) ;
#10524 = EDGE_CURVE ( 'NONE', #33210, #65583, #19281, .T. ) ;
#10525 = CARTESIAN_POINT ( 'NONE',  ( -48.90936936008873914, -25.22646736291544656, 6.474846148537197976 ) ) ;
#10526 = CARTESIAN_POINT ( 'NONE',  ( -22.11960324842224423, 4.537628740662121629, 11.49999999999998934 ) ) ;
#10527 = EDGE_CURVE ( 'NONE', #66719, #36980, #84052, .T. ) ;
#10529 = ORIENTED_EDGE ( 'NONE', *, *, #76817, .T. ) ;
#10528 = CARTESIAN_POINT ( 'NONE',  ( -101.1944152955115044, -29.50249789396666245, 6.858236616996303603 ) ) ;
#10530 = VERTEX_POINT ( 'NONE', #68836 ) ;
#10531 = CARTESIAN_POINT ( 'NONE',  ( -93.55620429048339304, -23.47593901973091235, -1.443836447539002865 ) ) ;
#10532 = VECTOR ( 'NONE', #36050, 1000.000000000000114 ) ;
#10533 = CARTESIAN_POINT ( 'NONE',  ( -94.58953762381672448, -24.64898659630528854, 1.056161002820827699 ) ) ;
#10534 = ORIENTED_EDGE ( 'NONE', *, *, #35129, .T. ) ;
#10535 = CARTESIAN_POINT ( 'NONE',  ( -4.955175619359221351, 20.59750927568439138, 11.49999999999998934 ) ) ;
#10536 = PLANE ( 'NONE',  #15739 ) ;
#10537 = FACE_OUTER_BOUND ( 'NONE', #59261, .T. ) ;
#10538 = CARTESIAN_POINT ( 'NONE',  ( -7.188523146553190912, -5.876774720514413630, 19.66116880005639800 ) ) ;
#10539 = CARTESIAN_POINT ( 'NONE',  ( 8.160000000000000142, 0.000000000000000000, 0.000000000000000000 ) ) ;
#10540 = CARTESIAN_POINT ( 'NONE',  ( 6.060481786824854389, 21.40074245971799627, -1.500000000000002220 ) ) ;
#10541 = DIRECTION ( 'NONE',  ( 1.232047923278981953E-16, -1.000000000000000000, 0.000000000000000000 ) ) ;
#10542 = ORIENTED_EDGE ( 'NONE', *, *, #55328, .T. ) ;
#10543 = DIRECTION ( 'NONE',  ( -1.000000000000000000, 0.000000000000000000, 0.000000000000000000 ) ) ;
#10544 = CARTESIAN_POINT ( 'NONE',  ( -37.52763684613194783, -24.65952944569304250, 1.056160979905692576 ) ) ;
#10545 = CARTESIAN_POINT ( 'NONE',  ( -16.37229413335033001, -10.43475415037859655, 11.49999999999999645 ) ) ;
#10546 = CIRCLE ( 'NONE', #21890, 0.2999999999999981570 ) ;
#10547 = CARTESIAN_POINT ( 'NONE',  ( -36.62904760676421745, -24.51419770103156637, 9.386484678747175181 ) ) ;
#10548 = CARTESIAN_POINT ( 'NONE',  ( 8.160000000000000142, -10.65233964170348635, -1.621096496867198589 ) ) ;
#10549 = EDGE_CURVE ( 'NONE', #14489, #88666, #99754, .T. ) ;
#10550 = CARTESIAN_POINT ( 'NONE',  ( -10.96721834449554933, 16.09610527815933168, 11.49999999999998934 ) ) ;
#10551 = CARTESIAN_POINT ( 'NONE',  ( -15.65470850568805083, 14.63654280257262386, -1.500000000000002220 ) ) ;
#10552 = CARTESIAN_POINT ( 'NONE',  ( -56.62287095715005592, -23.72747288104469376, -1.053458166803227014 ) ) ;
#10553 = B_SPLINE_CURVE_WITH_KNOTS ( 'NONE', 3,
 ( #3072, #4566, #72085, #11167 ),
 .UNSPECIFIED., .F., .F.,
 ( 4, 4 ),
 ( 0.000000000000000000, 1.000000000000000000 ),
 .UNSPECIFIED. ) ;
#10554 = CARTESIAN_POINT ( 'NONE',  ( -1.304987980769231948, -5.876774720514413630, 19.76512419871795245 ) ) ;
#10555 = LINE ( 'NONE', #61740, #4946 ) ;
#10556 = CARTESIAN_POINT ( 'NONE',  ( -57.62287095715004881, -23.47593901973091235, -1.443836447539007972 ) ) ;
#10557 = CARTESIAN_POINT ( 'NONE',  ( 12.47407908559008760, -19.03963781694049473, -1.500000000000002220 ) ) ;
#10558 = DIRECTION ( 'NONE',  ( -1.000000000000000000, 1.671923888193404544E-16, 3.473133724237705775E-15 ) ) ;
#10559 = CARTESIAN_POINT ( 'NONE',  ( -106.6235367854833243, -24.66019654487200441, 8.947790411086108620 ) ) ;
#10560 = CARTESIAN_POINT ( 'NONE',  ( -73.52287095715007581, -23.47593901973090169, -1.443836447538996870 ) ) ;
#10561 = CARTESIAN_POINT ( 'NONE',  ( 19.12242951303546334, 5.485007674754557527, 11.49999999999999645 ) ) ;
#10562 = CARTESIAN_POINT ( 'NONE',  ( -78.62287095715005592, -24.64898659630367916, 1.056161002820826145 ) ) ;
#10563 = CARTESIAN_POINT ( 'NONE',  ( -39.50522431325583739, -23.96169478059712787, 10.65365249895718769 ) ) ;
#10564 = LINE ( 'NONE', #47643, #74719 ) ;
#10565 = VERTEX_POINT ( 'NONE', #30258 ) ;
#10566 = LINE ( 'NONE', #24296, #23429 ) ;
#10567 = LINE ( 'NONE', #96807, #53973 ) ;
#10568 = CARTESIAN_POINT ( 'NONE',  ( -15.38093110518717666, 15.28219592669002402, -1.500000000000002220 ) ) ;
#10569 = CARTESIAN_POINT ( 'NONE',  ( -56.65739320408659552, -23.48786465467241413, 11.44779295918254647 ) ) ;
#10570 = CARTESIAN_POINT ( 'NONE',  ( -12.57844902324429448, -14.85176824229388437, -1.500000000000002220 ) ) ;
#10572 = B_SPLINE_CURVE_WITH_KNOTS ( 'NONE', 3,
 ( #80755, #54539, #93582, #46425 ),
 .UNSPECIFIED., .F., .F.,
 ( 4, 4 ),
 ( 0.000000000000000000, 0.0001000000000000028644 ),
 .UNSPECIFIED. ) ;
#10571 = DIRECTION ( 'NONE',  ( -3.773278334453080206E-23, 0.9999999999976377785, 2.173523156925979975E-06 ) ) ;
#10573 = ORIENTED_EDGE ( 'NONE', *, *, #86984, .T. ) ;
#10574 = CIRCLE ( 'NONE', #67304, 28.96799999999999642 ) ;
#10575 = CARTESIAN_POINT ( 'NONE',  ( 29.80070917940689412, -0.6647747205144266536, 27.39560796525321607 ) ) ;
#10576 = CARTESIAN_POINT ( 'NONE',  ( 17.38039551199336685, -10.77953091123627694, 11.49999999999999645 ) ) ;
#10577 = PLANE ( 'NONE',  #37530 ) ;
#10578 = CARTESIAN_POINT ( 'NONE',  ( -118.6228709571500701, -23.48783264082478794, -1.443836473390058384 ) ) ;
#10579 = EDGE_CURVE ( 'NONE', #44655, #52932, #60496, .T. ) ;
#10580 = ORIENTED_EDGE ( 'NONE', *, *, #31784, .T. ) ;
#10581 = DIRECTION ( 'NONE',  ( 3.773278334444166432E-23, -1.000000000000000000, 0.000000000000000000 ) ) ;
#10582 = CARTESIAN_POINT ( 'NONE',  ( 33.64447732616053344, 3.738877066258443627, -11.77943383154337376 ) ) ;
#10583 = CARTESIAN_POINT ( 'NONE',  ( 7.089543269230769162, -6.376774720514413630, 19.75741185897435415 ) ) ;
#10584 = DIRECTION ( 'NONE',  ( 1.000000000000000000, -0.000000000000000000, -0.000000000000000000 ) ) ;
#10585 = LINE ( 'NONE', #32932, #60857 ) ;
#10586 = FACE_OUTER_BOUND ( 'NONE', #19783, .T. ) ;
#10587 = VERTEX_POINT ( 'NONE', #47501 ) ;
#10588 = EDGE_CURVE ( 'NONE', #18475, #31114, #93654, .T. ) ;
#10589 = CARTESIAN_POINT ( 'NONE',  ( -66.55943436801386781, -23.73791477778911840, 11.05961554403170766 ) ) ;
#10590 = EDGE_CURVE ( 'NONE', #99097, #13321, #53299, .T. ) ;
#10591 = ADVANCED_FACE ( 'NONE', ( #94157 ), #69835, .T. ) ;
#10592 = CARTESIAN_POINT ( 'NONE',  ( 17.95915693031428262, 14.28781372813260120, 11.49999999999999645 ) ) ;
#10593 = CARTESIAN_POINT ( 'NONE',  ( 7.803535043518188274, -21.38454823780343617, 11.49999999999998934 ) ) ;
#10594 = CARTESIAN_POINT ( 'NONE',  ( 4.780030342074717886, -6.376774720514424288, 21.16398229115527130 ) ) ;
#10595 = CARTESIAN_POINT ( 'NONE',  ( -75.62287095715007013, -23.85229601348995132, 10.88205029486209163 ) ) ;
#10596 = CARTESIAN_POINT ( 'NONE',  ( -90.50112360221751828, -24.83618233451451118, 1.606449574219535492 ) ) ;
#10597 = EDGE_CURVE ( 'NONE', #68497, #62307, #22633, .T. ) ;
#10598 = CARTESIAN_POINT ( 'NONE',  ( 0.4325450954222598288, 2.877919977996279827E-16, -2.350000000000000089 ) ) ;
#10599 = CARTESIAN_POINT ( 'NONE',  ( -69.34917151123886470, -25.24288101849653998, 6.331981848628771559 ) ) ;
#10600 = VECTOR ( 'NONE', #82606, 1000.000000000000000 ) ;
#10601 = CARTESIAN_POINT ( 'NONE',  ( 8.256513476402210117, 20.27555108428041208, -1.500000000000002220 ) ) ;
#10602 = CARTESIAN_POINT ( 'NONE',  ( -69.58050984181491572, -24.66019654487199375, 8.947790411086119278 ) ) ;
#10603 = AXIS2_PLACEMENT_3D ( 'NONE', #64939, #79625, #77224 ) ;
#10604 = B_SPLINE_CURVE_WITH_KNOTS ( 'NONE', 3,
 ( #84594, #32311, #69374, #70888, #30304, #77963 ),
 .UNSPECIFIED., .F., .F.,
 ( 4, 2, 4 ),
 ( 0.000000000000000000, 0.001380764517854766050, 0.002761529035709532100 ),
 .UNSPECIFIED. ) ;
#10605 = CARTESIAN_POINT ( 'NONE',  ( -48.87380231474225667, -25.26256937810135028, 6.137091986423513390 ) ) ;
#10606 = CARTESIAN_POINT ( 'NONE',  ( -71.69009546357753493, -25.26814388089136187, 5.957693125896286190 ) ) ;
#10607 = CARTESIAN_POINT ( 'NONE',  ( -99.16166289166534398, -25.25460552112298984, 5.311370849885090450 ) ) ;
#10608 = ORIENTED_EDGE ( 'NONE', *, *, #13103, .T. ) ;
#10609 = CARTESIAN_POINT ( 'NONE',  ( -19.37329759448073574, 6.469241145865432863, 11.49999999999998934 ) ) ;
#10610 = ORIENTED_EDGE ( 'NONE', *, *, #67090, .T. ) ;
#10611 = VECTOR ( 'NONE', #56737, 1000.000000000000000 ) ;
#10612 = ORIENTED_EDGE ( 'NONE', *, *, #71566, .T. ) ;
#10613 = B_SPLINE_CURVE_WITH_KNOTS ( 'NONE', 3,
 ( #6345, #76829, #36803, #13449, #67265, #74848, #90582 ),
 .UNSPECIFIED., .F., .F.,
 ( 4, 1, 1, 1, 4 ),
 ( 0.000000000000000000, 0.2537340756906609762, 0.5030351201318566945, 0.7500135973308793558, 1.000000000000000000 ),
 .UNSPECIFIED. ) ;
#10614 = EDGE_CURVE ( 'NONE', #87028, #17763, #12132, .T. ) ;
#10615 = EDGE_CURVE ( 'NONE', #85130, #78621, #39282, .T. ) ;
#10616 = CARTESIAN_POINT ( 'NONE',  ( 22.26416322464526232, -5.798680748638591176, 11.49999999999998934 ) ) ;
#10617 = LINE ( 'NONE', #34459, #50293 ) ;
#10618 = CIRCLE ( 'NONE', #73768, 24.00000000000000000 ) ;
#10619 = ORIENTED_EDGE ( 'NONE', *, *, #58290, .T. ) ;
#10620 = CARTESIAN_POINT ( 'NONE',  ( -108.5200640884878283, -23.73791477778912196, 11.05961554403169878 ) ) ;
#10621 = CARTESIAN_POINT ( 'NONE',  ( -48.52287095715006870, -23.96177878511308634, 10.65340807706329862 ) ) ;
#10622 = AXIS2_PLACEMENT_3D ( 'NONE', #14698, #7091, #61399 ) ;
#10623 = EDGE_CURVE ( 'NONE', #94697, #76683, #31262, .T. ) ;
#10624 = DIRECTION ( 'NONE',  ( -1.000000000000000000, 0.000000000000000000, -0.000000000000000000 ) ) ;
#10625 = CARTESIAN_POINT ( 'NONE',  ( -117.0509084556500881, -25.24723402497068037, 6.200314804519077683 ) ) ;
#10627 = EDGE_LOOP ( 'NONE', ( #86489, #67763, #63507, #93065 ) ) ;
#10626 = CARTESIAN_POINT ( 'NONE',  ( -20.51402961445061734, 6.013860829077147585, 11.49999999999999645 ) ) ;
#10628 = ORIENTED_EDGE ( 'NONE', *, *, #39112, .F. ) ;
#10629 = CARTESIAN_POINT ( 'NONE',  ( -10.71655374829924767, -19.46388382022006525, -1.500000000000002220 ) ) ;
#10630 = CARTESIAN_POINT ( 'NONE',  ( 12.06641648444584369, 16.80774221200798735, 11.49999999999998934 ) ) ;
#10631 = EDGE_CURVE ( 'NONE', #95426, #42247, #26701, .T. ) ;
#10632 = ORIENTED_EDGE ( 'NONE', *, *, #47073, .F. ) ;
#10633 = CARTESIAN_POINT ( 'NONE',  ( -5.923037968371668072, -5.876774720514413630, 19.62288733224861303 ) ) ;
#10634 = LINE ( 'NONE', #97370, #37245 ) ;
#10635 = ORIENTED_EDGE ( 'NONE', *, *, #55309, .F. ) ;
#10636 = DIRECTION ( 'NONE',  ( -3.773278334453079618E-23, 0.9999999999976377785, 2.173523156925979975E-06 ) ) ;
#10637 = ORIENTED_EDGE ( 'NONE', *, *, #89330, .F. ) ;
#10638 = CARTESIAN_POINT ( 'NONE',  ( -50.38191529551148307, -25.27517877397642110, 2.832404459008946773 ) ) ;
#10639 =( LENGTH_UNIT ( ) NAMED_UNIT ( * ) SI_UNIT ( .MILLI., .METRE. ) );
#10640 = CARTESIAN_POINT ( 'NONE',  ( -0.7727808018759799724, -20.89725122839497828, -1.500000000000002220 ) ) ;
#10641 = CARTESIAN_POINT ( 'NONE',  ( -21.85961425739535358, 0.8689724601130633941, 11.49999999999999645 ) ) ;
#10642 = ADVANCED_FACE ( 'NONE', ( #53624 ), #70836, .T. ) ;
#10643 = CARTESIAN_POINT ( 'NONE',  ( -26.43901205547898670, -24.89279823874531061, 6.777242086831815726 ) ) ;
#10644 = FACE_OUTER_BOUND ( 'NONE', #32842, .T. ) ;
#10645 = CARTESIAN_POINT ( 'NONE',  ( 3.433349652534986696, 22.22849440524942111, 11.49999999999998934 ) ) ;
#10646 = CARTESIAN_POINT ( 'NONE',  ( -17.10473743203234775, -12.04273770408705246, 11.49999999999998934 ) ) ;
#10647 = EDGE_CURVE ( 'NONE', #13725, #26613, #52267, .T. ) ;
#10648 = CARTESIAN_POINT ( 'NONE',  ( -38.60080910673752896, -23.96119346886880308, -0.6495511937831990323 ) ) ;
#10649 = LINE ( 'NONE', #26372, #3217 ) ;
#10650 = CARTESIAN_POINT ( 'NONE',  ( -44.62287095715004881, -23.47593901973091235, -1.443836447539011525 ) ) ;
#10651 = ORIENTED_EDGE ( 'NONE', *, *, #23665, .F. ) ;
#10652 = EDGE_CURVE ( 'NONE', #67301, #20858, #84548, .T. ) ;
#10653 = VECTOR ( 'NONE', #28420, 1000.000000000000000 ) ;
#10654 = EDGE_LOOP ( 'NONE', ( #63493, #4580, #41701, #71296 ) ) ;
#10655 = ORIENTED_EDGE ( 'NONE', *, *, #97357, .F. ) ;
#10656 = CARTESIAN_POINT ( 'NONE',  ( -99.33919073176147663, -25.12215527841457785, 6.423374680119191993 ) ) ;
#10657 = ORIENTED_EDGE ( 'NONE', *, *, #17962, .F. ) ;
#10658 = B_SPLINE_CURVE_WITH_KNOTS ( 'NONE', 3,
 ( #95355, #89747, #33958, #42587 ),
 .UNSPECIFIED., .F., .F.,
 ( 4, 4 ),
 ( 0.5208719419040093168, 0.5298783731761248506 ),
 .UNSPECIFIED. ) ;
#10659 = CARTESIAN_POINT ( 'NONE',  ( 0.5228555243449846124, 21.43159495547403282, -1.500000000000002220 ) ) ;
#10660 = EDGE_LOOP ( 'NONE', ( #28962, #46528, #100186, #93501 ) ) ;
#10661 = CARTESIAN_POINT ( 'NONE',  ( 0.03625801282051022839, -6.376774720514410077, 19.27714342948718240 ) ) ;
#10662 = CARTESIAN_POINT ( 'NONE',  ( 10.44912437418449969, 18.32051524777507723, 11.49999999999998934 ) ) ;
#10663 = CARTESIAN_POINT ( 'NONE',  ( -30.59475437726466751, -24.84008585880724596, 8.370654131274084975 ) ) ;
#10664 = CARTESIAN_POINT ( 'NONE',  ( -127.4728709571500360, -25.40558663563398767, 5.000950440326727531 ) ) ;
#10665 = CARTESIAN_POINT ( 'NONE',  ( -10.34999999999999254, 4.999999999999999112, 0.000000000000000000 ) ) ;
#10666 = CARTESIAN_POINT ( 'NONE',  ( -101.6292215989844721, -24.15543982623907482, -0.2315651400026588480 ) ) ;
#10667 = LINE ( 'NONE', #58841, #53545 ) ;
#10668 = CARTESIAN_POINT ( 'NONE',  ( 6.148021820315829444, -21.18842874637755358, -1.500000000000002220 ) ) ;
#10669 = ORIENTED_EDGE ( 'NONE', *, *, #92593, .T. ) ;
#10670 = CARTESIAN_POINT ( 'NONE',  ( -116.6285100755955426, -23.73766607897671577, -1.055555164236427590 ) ) ;
#10671 = PLANE ( 'NONE',  #30281 ) ;
#10672 = CARTESIAN_POINT ( 'NONE',  ( -40.63161819696095733, -25.31624740998290335, 5.540357839096273551 ) ) ;
#10673 = CARTESIAN_POINT ( 'NONE',  ( -62.55964932266956424, -23.73791477778911840, 11.05961554403171121 ) ) ;
#10674 = B_SPLINE_CURVE_WITH_KNOTS ( 'NONE', 3,
 ( #98546, #28059, #89949, #58518 ),
 .UNSPECIFIED., .F., .F.,
 ( 4, 4 ),
 ( 0.8593950407724427754, 0.8603957878132079129 ),
 .UNSPECIFIED. ) ;
#10675 = FACE_OUTER_BOUND ( 'NONE', #64975, .T. ) ;
#10676 = CARTESIAN_POINT ( 'NONE',  ( -38.62287095715005592, -23.48786465467240703, 11.44779295918255180 ) ) ;
#10677 = CARTESIAN_POINT ( 'NONE',  ( -18.83571791729191958, -9.990160686573538840, 11.49999999999998934 ) ) ;
#10678 = DIRECTION ( 'NONE',  ( -1.000000000000000000, -3.773278334444167608E-23, -8.201307833595939069E-29 ) ) ;
#10679 = CARTESIAN_POINT ( 'NONE',  ( -50.61388679491238918, -25.19715874454066906, 3.309015525357478893 ) ) ;
#10680 = CARTESIAN_POINT ( 'NONE',  ( 8.160000000000000142, 8.793627758918228565, -2.994553991265763049 ) ) ;
#10681 = CARTESIAN_POINT ( 'NONE',  ( -81.45492590815939593, -25.22427035087299174, 6.407323222939080409 ) ) ;
#10682 = CARTESIAN_POINT ( 'NONE',  ( 18.83488669200175281, -12.41447709603701632, -1.500000000000002220 ) ) ;
#10683 = AXIS2_PLACEMENT_3D ( 'NONE', #89116, #11981, #42950 ) ;
#10684 = LINE ( 'NONE', #17289, #31167 ) ;
#10685 = ORIENTED_EDGE ( 'NONE', *, *, #40937, .F. ) ;
#10686 = VECTOR ( 'NONE', #99244, 1000.000000000000114 ) ;
#10687 = CARTESIAN_POINT ( 'NONE',  ( 10.11589461582716076, 3.316774720514427344, -28.03692668899584106 ) ) ;
#10688 = CARTESIAN_POINT ( 'NONE',  ( -67.62287095715005592, -23.47593901973091235, -1.443836447539006196 ) ) ;
#10689 = CARTESIAN_POINT ( 'NONE',  ( -19.65353550717971487, 1.628721094194526486, 11.49999999999999645 ) ) ;
#10690 = CARTESIAN_POINT ( 'NONE',  ( -38.62287095715005592, -29.50250243563736774, 8.947779886222148704 ) ) ;
#10691 = VECTOR ( 'NONE', #79699, 1000.000000000000000 ) ;
#10692 = CARTESIAN_POINT ( 'NONE',  ( -67.60279521098367184, -23.73766607897670511, -1.055555164236457788 ) ) ;
#10693 = ORIENTED_EDGE ( 'NONE', *, *, #12994, .F. ) ;
#10694 = AXIS2_PLACEMENT_3D ( 'NONE', #87732, #66903, #26823 ) ;
#10695 = CARTESIAN_POINT ( 'NONE',  ( -117.5562042904833788, -24.65952944569305316, 1.056160979905707009 ) ) ;
#10696 = FACE_OUTER_BOUND ( 'NONE', #69239, .T. ) ;
#10697 = FACE_OUTER_BOUND ( 'NONE', #88720, .T. ) ;
#10698 = CARTESIAN_POINT ( 'NONE',  ( -90.62287095715004170, -23.47593901973091235, -1.443836447539002865 ) ) ;
#10700 = LINE ( 'NONE', #30650, #90070 ) ;
#10699 = VECTOR ( 'NONE', #88481, 1000.000000000000000 ) ;
#10701 = CARTESIAN_POINT ( 'NONE',  ( -109.6228709571500417, -23.48783264082478794, -1.443836473390060382 ) ) ;
#10702 = CARTESIAN_POINT ( 'NONE',  ( -81.67165532884091306, -25.16133908214882808, 6.940091796881004527 ) ) ;
#10703 = CARTESIAN_POINT ( 'NONE',  ( -10.52764212615999639, 16.74383705166681580, 11.49999999999998934 ) ) ;
#10704 = ORIENTED_EDGE ( 'NONE', *, *, #95849, .F. ) ;
#10705 = CARTESIAN_POINT ( 'NONE',  ( 20.19498477198788322, 0.2509159868347127231, 11.49999999999999645 ) ) ;
#10706 = CARTESIAN_POINT ( 'NONE',  ( 5.872047395031165351, -5.876774720514416295, 20.29192741308114734 ) ) ;
#10707 = B_SPLINE_CURVE_WITH_KNOTS ( 'NONE', 3,
 ( #22665, #21180, #44534, #14568 ),
 .UNSPECIFIED., .F., .F.,
 ( 4, 4 ),
 ( 0.7610434424937544406, 0.7700498737658699744 ),
 .UNSPECIFIED. ) ;
#10708 = ORIENTED_EDGE ( 'NONE', *, *, #27874, .T. ) ;
#10709 = CARTESIAN_POINT ( 'NONE',  ( 26.73860345374794889, 5.356774720514427379, -3.111611894936215705 ) ) ;
#10710 = FACE_OUTER_BOUND ( 'NONE', #87007, .T. ) ;
#10711 = FACE_OUTER_BOUND ( 'NONE', #7136, .T. ) ;
#10712 = DIRECTION ( 'NONE',  ( 0.000000000000000000, 0.000000000000000000, -1.000000000000000000 ) ) ;
#10713 = ADVANCED_FACE ( 'NONE', ( #92654 ), #71338, .T. ) ;
#10714 = CARTESIAN_POINT ( 'NONE',  ( -39.62287095715006302, -23.73907113216990439, -1.053371485793234807 ) ) ;
#10715 = ADVANCED_FACE ( 'NONE', ( #77422 ), #23134, .F. ) ;
#10716 = CARTESIAN_POINT ( 'NONE',  ( -58.62287095715004881, -24.64898659630367916, 1.056161002820822592 ) ) ;
#10717 = CARTESIAN_POINT ( 'NONE',  ( 20.02521558760690112, -0.9251608499524575091, 11.49999999999998934 ) ) ;
#10718 = ADVANCED_FACE ( 'NONE', ( #88064 ), #88563, .F. ) ;
#10719 = DIRECTION ( 'NONE',  ( -3.773278334444166432E-23, 1.000000000000000000, 0.000000000000000000 ) ) ;
#10720 = ORIENTED_EDGE ( 'NONE', *, *, #1241, .T. ) ;
#10721 = ADVANCED_FACE ( 'NONE', ( #56627 ), #2837, .F. ) ;
#10722 = ADVANCED_FACE ( 'NONE', ( #64755 ), #19037, .F. ) ;
#10723 = CARTESIAN_POINT ( 'NONE',  ( -103.5228709571500758, -24.35013146730203815, 9.818937971375097717 ) ) ;
#10724 = CARTESIAN_POINT ( 'NONE',  ( -35.63737625694447786, -24.63355581998387223, 0.9682620441943878831 ) ) ;
#10725 = CARTESIAN_POINT ( 'NONE',  ( -79.62287095715005592, -29.50248528299804818, 1.056150453629038477 ) ) ;
#10726 = DIRECTION ( 'NONE',  ( -0.9951627101165076983, 0.000000000000000000, 0.09824042138329588947 ) ) ;
#10727 = CARTESIAN_POINT ( 'NONE',  ( -101.2039755539695136, -25.14901327759760719, 3.054686125765971205 ) ) ;
#10728 = CARTESIAN_POINT ( 'NONE',  ( -40.41683116089613748, -29.50249403413438642, 5.082395270846652657 ) ) ;
#10729 = CARTESIAN_POINT ( 'NONE',  ( -100.9381932429152045, -25.20650842489795807, 6.812665538484691474 ) ) ;
#10730 = ORIENTED_EDGE ( 'NONE', *, *, #88332, .T. ) ;
#10731 = CARTESIAN_POINT ( 'NONE',  ( -15.63206872509828571, 12.99414084278249071, 11.49999999999998934 ) ) ;
#10732 = ORIENTED_EDGE ( 'NONE', *, *, #42025, .F. ) ;
#10733 = EDGE_CURVE ( 'NONE', #70138, #67301, #65339, .T. ) ;
#10734 = CARTESIAN_POINT ( 'NONE',  ( -32.63552282000483018, -24.34968618360933590, 0.1864209137778856384 ) ) ;
#10735 = CARTESIAN_POINT ( 'NONE',  ( -127.5212380171430198, -24.35071581493544102, 9.817618358456009275 ) ) ;
#10736 = ORIENTED_EDGE ( 'NONE', *, *, #77590, .T. ) ;
#10737 = FACE_OUTER_BOUND ( 'NONE', #67519, .T. ) ;
#10738 = AXIS2_PLACEMENT_3D ( 'NONE', #23153, #62760, #14556 ) ;
#10739 = CARTESIAN_POINT ( 'NONE',  ( 15.07033713866346147, 3.525255902978593703, -27.30453278895961233 ) ) ;
#10740 = ADVANCED_FACE ( 'NONE', ( #72843 ), #52334, .F. ) ;
#10741 = CARTESIAN_POINT ( 'NONE',  ( -30.47287095715007510, -24.67069026960422562, 8.894128854304588216 ) ) ;
#10742 = CARTESIAN_POINT ( 'NONE',  ( 19.29917393477590437, 8.764703196630867055, 11.49999999999999645 ) ) ;
#10743 = CARTESIAN_POINT ( 'NONE',  ( 21.88104185797606505, 3.448541436957560880, -1.500000000000002220 ) ) ;
#10744 = CARTESIAN_POINT ( 'NONE',  ( 3.086129920417311823, 20.35385046113321295, -1.500000000000002220 ) ) ;
#10745 = CIRCLE ( 'NONE', #20431, 5.500000000000001776 ) ;
#10746 = ORIENTED_EDGE ( 'NONE', *, *, #83212, .F. ) ;
#10747 = CARTESIAN_POINT ( 'NONE',  ( -94.52287095715007581, -24.51387760970725083, 9.387446482453412955 ) ) ;
#10748 = ORIENTED_EDGE ( 'NONE', *, *, #18826, .F. ) ;
#10749 = DIRECTION ( 'NONE',  ( -3.773278334453079618E-23, 0.9999999999976377785, 2.173523156925979975E-06 ) ) ;
#10750 = CARTESIAN_POINT ( 'NONE',  ( -50.52287095715006870, -24.14406661686760458, 10.28769366194083013 ) ) ;
#10751 = VERTEX_POINT ( 'NONE', #49510 ) ;
#10752 = AXIS2_PLACEMENT_3D ( 'NONE', #38804, #87863, #41194 ) ;
#10753 = ORIENTED_EDGE ( 'NONE', *, *, #72999, .T. ) ;
#10754 = ORIENTED_EDGE ( 'NONE', *, *, #10960, .F. ) ;
#10755 = CARTESIAN_POINT ( 'NONE',  ( -83.62287095715004170, -23.96127896941632685, -0.6493128931037841500 ) ) ;
#10756 = CARTESIAN_POINT ( 'NONE',  ( 7.010993867624484288, -5.876774720514417183, 20.34381700913260715 ) ) ;
#10757 = CARTESIAN_POINT ( 'NONE',  ( -91.62287095715004170, -23.73907113216990794, -1.053371485793224149 ) ) ;
#10758 = CARTESIAN_POINT ( 'NONE',  ( 8.970943996638910178, -18.66293075132952950, -1.500000000000002220 ) ) ;
#10759 = CIRCLE ( 'NONE', #85277, 20.00000000000000355 ) ;
#10760 = CARTESIAN_POINT ( 'NONE',  ( -7.614213781628100364, -20.28429660096114517, 11.49999999999999645 ) ) ;
#10761 = ORIENTED_EDGE ( 'NONE', *, *, #50586, .F. ) ;
#10762 = CARTESIAN_POINT ( 'NONE',  ( -27.96875734969026084, -6.143225279485574397, 24.50402280011861933 ) ) ;
#10763 = CARTESIAN_POINT ( 'NONE',  ( -110.7042636268849094, -25.11831750865088964, 2.876796822534068987 ) ) ;
#10764 = CARTESIAN_POINT ( 'NONE',  ( 21.53444271425275858, 6.169869319618734416, 11.49999999999998934 ) ) ;
#10765 = EDGE_CURVE ( 'NONE', #77504, #40376, #15723, .T. ) ;
#10766 = CARTESIAN_POINT ( 'NONE',  ( 22.81105451610979173, -4.772774720514425972, -18.46691820600746681 ) ) ;
#10767 = DIRECTION ( 'NONE',  ( 0.000000000000000000, -1.000000000000000000, 0.000000000000000000 ) ) ;
#10768 = ORIENTED_EDGE ( 'NONE', *, *, #64578, .T. ) ;
#10769 = CARTESIAN_POINT ( 'NONE',  ( -45.55620429048339304, -24.99132157543166599, 2.256160258750668390 ) ) ;
#10770 = CARTESIAN_POINT ( 'NONE',  ( -85.58953762381673869, -24.99132157543083821, 2.256160258750495640 ) ) ;
#10771 = ORIENTED_EDGE ( 'NONE', *, *, #24341, .F. ) ;
#10772 = ORIENTED_EDGE ( 'NONE', *, *, #13099, .F. ) ;
#10773 = EDGE_CURVE ( 'NONE', #85117, #65926, #6023, .T. ) ;
#10774 = CARTESIAN_POINT ( 'NONE',  ( -103.6228709571500701, -24.33832256526969928, 0.1851278514119971963 ) ) ;
#10775 = ORIENTED_EDGE ( 'NONE', *, *, #22983, .T. ) ;
#10776 = DIRECTION ( 'NONE',  ( 0.000000000000000000, -0.9999999999976377785, -2.173523156925979975E-06 ) ) ;
#10777 = CARTESIAN_POINT ( 'NONE',  ( -3.310264809446246570, -21.00426241492911927, -1.500000000000002220 ) ) ;
#10778 = ORIENTED_EDGE ( 'NONE', *, *, #12249, .T. ) ;
#10779 = CARTESIAN_POINT ( 'NONE',  ( -100.4426124108961176, -25.12298712672051337, 7.101635559041870494 ) ) ;
#10780 = CARTESIAN_POINT ( 'NONE',  ( -6.457742198559264679, -20.83860622980983024, 11.49999999999998934 ) ) ;
#10781 = CARTESIAN_POINT ( 'NONE',  ( -52.50174715697038152, -24.15620529776627734, 10.23563542870661180 ) ) ;
#10782 = CARTESIAN_POINT ( 'NONE',  ( 6.830155907162054341, -6.376774720514427841, 21.76451523534627341 ) ) ;
#10783 = FACE_OUTER_BOUND ( 'NONE', #6077, .T. ) ;
#10784 = CARTESIAN_POINT ( 'NONE',  ( 21.76694381678408519, 2.417257996116004115, -1.500000000000002220 ) ) ;
#10785 = CARTESIAN_POINT ( 'NONE',  ( -66.62287095715005592, -24.65952944569304606, 1.056160979905696573 ) ) ;
#10786 = ORIENTED_EDGE ( 'NONE', *, *, #12585, .F. ) ;
#10787 = CARTESIAN_POINT ( 'NONE',  ( 25.53193795238742325, 4.590426722874489940, -10.98904603773835476 ) ) ;
#10788 = CARTESIAN_POINT ( 'NONE',  ( -85.58736961604824955, -24.63419186844611275, 9.035850630976915099 ) ) ;
#10789 = VECTOR ( 'NONE', #38948, 1000.000000000000000 ) ;
#10790 = ORIENTED_EDGE ( 'NONE', *, *, #86927, .T. ) ;
#10791 = CARTESIAN_POINT ( 'NONE',  ( 32.98733314340959311, 0.3587747205144265483, 2.074222136288530027 ) ) ;
#10792 = ORIENTED_EDGE ( 'NONE', *, *, #19017, .T. ) ;
#10793 = FACE_OUTER_BOUND ( 'NONE', #43817, .T. ) ;
#10794 = CARTESIAN_POINT ( 'NONE',  ( -31.24388727629347073, -25.31501645218191143, 6.103840189645985070 ) ) ;
#10795 = CARTESIAN_POINT ( 'NONE',  ( -3.247986963444697395, 20.98610878802851332, 11.49999999999998934 ) ) ;
#10796 = DIRECTION ( 'NONE',  ( 0.000000000000000000, 1.000000000000000000, 0.000000000000000000 ) ) ;
#10797 = CARTESIAN_POINT ( 'NONE',  ( -130.5728709571500588, -24.93418366566758948, 8.369064737642425200 ) ) ;
#10798 = CARTESIAN_POINT ( 'NONE',  ( -100.4426124108961176, -25.12298712672051337, 7.101635559041870494 ) ) ;
#10799 = CARTESIAN_POINT ( 'NONE',  ( -68.59250847563207287, -24.15543982623907127, -0.2315651400026649820 ) ) ;
#10800 = CARTESIAN_POINT ( 'NONE',  ( 13.61561175257155298, 13.87280521877887018, -1.500000000000002220 ) ) ;
#10801 = CARTESIAN_POINT ( 'NONE',  ( -45.60108961187481214, -24.15503026093915651, -0.2815557561904415418 ) ) ;
#10802 = ORIENTED_EDGE ( 'NONE', *, *, #96644, .T. ) ;
#10803 = CARTESIAN_POINT ( 'NONE',  ( -13.79594968651775666, -13.80015156857029268, 11.49999999999999645 ) ) ;
#10804 = CARTESIAN_POINT ( 'NONE',  ( -5.314757719055156038, -6.376774720514411854, 19.55912026249540858 ) ) ;
#10805 = CARTESIAN_POINT ( 'NONE',  ( -68.52287095715006160, -24.64898659630528854, 1.056161002820824368 ) ) ;
#10806 = ORIENTED_EDGE ( 'NONE', *, *, #37843, .F. ) ;
#10807 = CARTESIAN_POINT ( 'NONE',  ( 1.999999999999999112, 18.50000000000000000, 0.000000000000000000 ) ) ;
#10808 = FACE_OUTER_BOUND ( 'NONE', #65025, .T. ) ;
#10809 = AXIS2_PLACEMENT_3D ( 'NONE', #54266, #99413, #85194 ) ;
#10810 = CARTESIAN_POINT ( 'NONE',  ( -51.55620429048339304, -23.48783264082478084, -1.443836473390070152 ) ) ;
#10811 = CARTESIAN_POINT ( 'NONE',  ( -80.89908437845683409, -25.03156050640678743, 7.516075442759441394 ) ) ;
#10812 = CARTESIAN_POINT ( 'NONE',  ( -15.16924259816527609, 12.53091941037558854, 11.49999999999998934 ) ) ;
#10813 = VERTEX_POINT ( 'NONE', #96664 ) ;
#10814 = DIRECTION ( 'NONE',  ( 0.000000000000000000, -1.000000000000000000, 0.000000000000000000 ) ) ;
#10815 = CARTESIAN_POINT ( 'NONE',  ( 19.36532470938277228, 12.59445105952145738, -1.500000000000002220 ) ) ;
#10816 = AXIS2_PLACEMENT_3D ( 'NONE', #54874, #68590, #44758 ) ;
#10817 = SECURITY_CLASSIFICATION_LEVEL ( 'unclassified' ) ;
#10818 = ORIENTED_EDGE ( 'NONE', *, *, #63163, .T. ) ;
#10819 = FACE_OUTER_BOUND ( 'NONE', #60993, .T. ) ;
#10820 = CARTESIAN_POINT ( 'NONE',  ( -1.845912073933368536, -6.376774720514408301, 19.53740760792477360 ) ) ;
#10821 = CARTESIAN_POINT ( 'NONE',  ( -92.62287095715009855, -23.73907113216991505, -1.053371485793224371 ) ) ;
#10822 = CARTESIAN_POINT ( 'NONE',  ( -105.6228709571499991, -24.63345952396255711, 9.038047939301501188 ) ) ;
#10823 = CARTESIAN_POINT ( 'NONE',  ( 32.50838937279095120, 2.682774720514426559, -10.74666623472941218 ) ) ;
#10824 = AXIS2_PLACEMENT_3D ( 'NONE', #12368, #81893, #27614 ) ;
#10825 = EDGE_CURVE ( 'NONE', #37448, #71104, #13423, .T. ) ;
#10826 = AXIS2_PLACEMENT_3D ( 'NONE', #64211, #26629, #25623 ) ;
#10827 = LINE ( 'NONE', #58018, #39233 ) ;
#10828 = CARTESIAN_POINT ( 'NONE',  ( -73.52287095715013265, -24.33832256527049154, 0.1851278514138621212 ) ) ;
#10829 = CARTESIAN_POINT ( 'NONE',  ( 16.79105032741591330, -10.77411451815220822, -1.500000000000002220 ) ) ;
#10830 = EDGE_CURVE ( 'NONE', #22614, #72334, #89061, .T. ) ;
#10831 = CARTESIAN_POINT ( 'NONE',  ( -47.52287095715006160, -29.50248528299804818, 1.056150453629033370 ) ) ;
#10832 = CARTESIAN_POINT ( 'NONE',  ( 12.47747183659840786, 15.48776231947736015, -1.500000000000002220 ) ) ;
#10833 = EDGE_LOOP ( 'NONE', ( #95535, #18876, #14621, #19864 ) ) ;
#10834 = AXIS2_PLACEMENT_3D ( 'NONE', #48544, #34805, #33802 ) ;
#10835 = CARTESIAN_POINT ( 'NONE',  ( -89.81226385320383088, -25.27367468601175204, 3.993462154588550916 ) ) ;
#10836 = ADVANCED_FACE ( 'NONE', ( #25145 ), #6837, .T. ) ;
#10837 = ADVANCED_FACE ( 'NONE', ( #21519 ), #58611, .T. ) ;
#10838 = DIRECTION ( 'NONE',  ( 3.773278334444166432E-23, -1.000000000000000000, 0.000000000000000000 ) ) ;
#10839 = LINE ( 'NONE', #98428, #94928 ) ;
#10840 = CARTESIAN_POINT ( 'NONE',  ( -80.57997149293382222, -25.00182538069147142, 7.747789668545041586 ) ) ;
#10841 = CARTESIAN_POINT ( 'NONE',  ( -11.59579830748209517, 17.24510332420730663, 11.49999999999999645 ) ) ;
#10842 = FACE_OUTER_BOUND ( 'NONE', #10992, .T. ) ;
#10843 = EDGE_CURVE ( 'NONE', #77757, #79556, #84734, .T. ) ;
#10844 = DIRECTION ( 'NONE',  ( -1.000000000000000000, 0.000000000000000000, -0.000000000000000000 ) ) ;
#10845 = CARTESIAN_POINT ( 'NONE',  ( -19.58686714514938387, 11.73587220785771379, 11.49999999999999645 ) ) ;
#10846 = ORIENTED_EDGE ( 'NONE', *, *, #64012, .T. ) ;
#10847 = LINE ( 'NONE', #57538, #25195 ) ;
#10848 = CYLINDRICAL_SURFACE ( 'NONE', #41981, 3.500000000000000000 ) ;
#10849 = ORIENTED_EDGE ( 'NONE', *, *, #94370, .T. ) ;
#10850 = CARTESIAN_POINT ( 'NONE',  ( 14.48468284575590204, 14.13777120147990729, -1.500000000000002220 ) ) ;
#10851 = CARTESIAN_POINT ( 'NONE',  ( -106.5228709571501469, -23.96177878511310055, 10.65340807706329507 ) ) ;
#10852 = CARTESIAN_POINT ( 'NONE',  ( 12.16765770914787304, 5.965225279485572685, -27.57618308014988173 ) ) ;
#10853 = VECTOR ( 'NONE', #96492, 1000.000000000000114 ) ;
#10854 = EDGE_CURVE ( 'NONE', #31528, #7274, #7275, .T. ) ;
#10855 = CARTESIAN_POINT ( 'NONE',  ( -50.55620429048339304, -23.48786465467240703, 11.44779295918255357 ) ) ;
#10856 = ORIENTED_EDGE ( 'NONE', *, *, #15829, .F. ) ;
#10857 = CARTESIAN_POINT ( 'NONE',  ( -105.6228709571500559, -23.47596703998600631, 11.44779298504227860 ) ) ;
#10858 = CARTESIAN_POINT ( 'NONE',  ( -10.12789510953808758, 4.109924279452578766, 30.41617935552199370 ) ) ;
#10859 = CARTESIAN_POINT ( 'NONE',  ( 18.25133680241413359, 8.160682379734268466, -1.500000000000002220 ) ) ;
#10860 = CARTESIAN_POINT ( 'NONE',  ( 15.04517842881462819, -14.58609674458608829, 11.49999999999999645 ) ) ;
#10861 = AXIS2_PLACEMENT_3D ( 'NONE', #39857, #22122, #76903 ) ;
#10862 = CARTESIAN_POINT ( 'NONE',  ( -28.07643796139391057, -24.68838396948798319, 8.218772173470371811 ) ) ;
#10863 = CARTESIAN_POINT ( 'NONE',  ( -93.52287095715006160, -23.48786465467241769, 11.44779295918254292 ) ) ;
#10864 = CARTESIAN_POINT ( 'NONE',  ( 7.103389721457689099, 20.86620700561973862, 11.49999999999998934 ) ) ;
#10865 = CARTESIAN_POINT ( 'NONE',  ( -39.78092788824959314, -25.27806063382736568, 4.883081681052058975 ) ) ;
#10866 = EDGE_LOOP ( 'NONE', ( #79703, #91468, #23348, #59026 ) ) ;
#10867 = CARTESIAN_POINT ( 'NONE',  ( -8.349999999999971223, 27.69999999999999574, 2.100000000000000089 ) ) ;
#10868 = CARTESIAN_POINT ( 'NONE',  ( -88.62287095715004170, -29.50248528299804818, 1.056150453629040253 ) ) ;
#10869 = LINE ( 'NONE', #41834, #8951 ) ;
#10870 = ORIENTED_EDGE ( 'NONE', *, *, #87243, .T. ) ;
#10871 = DIRECTION ( 'NONE',  ( 3.773278334444167608E-23, -1.000000000000000000, 0.000000000000000000 ) ) ;
#10872 = ORIENTED_EDGE ( 'NONE', *, *, #22489, .F. ) ;
#10873 = ORIENTED_EDGE ( 'NONE', *, *, #52594, .T. ) ;
#10874 = DIRECTION ( 'NONE',  ( -0.000000000000000000, -1.000000000000000000, -0.000000000000000000 ) ) ;
#10875 = FACE_OUTER_BOUND ( 'NONE', #96007, .T. ) ;
#10876 = CARTESIAN_POINT ( 'NONE',  ( -91.15361000704997707, -25.26877915520014639, 5.947789088310639904 ) ) ;
#10877 = CARTESIAN_POINT ( 'NONE',  ( 1.819314030819549233, -20.42850443921780013, -1.500000000000002220 ) ) ;
#10878 = ORIENTED_EDGE ( 'NONE', *, *, #76208, .T. ) ;
#10879 = CARTESIAN_POINT ( 'NONE',  ( -49.27932720226401386, -25.25530279399480449, 6.214150124083338333 ) ) ;
#10880 = CARTESIAN_POINT ( 'NONE',  ( -29.49875734969026198, -5.965225279485572685, 7.870022800118625206 ) ) ;
#10881 = PLANE ( 'NONE',  #67476 ) ;
#10882 = CARTESIAN_POINT ( 'NONE',  ( 15.82088602905085750, -15.72875506571707760, 11.49999999999998934 ) ) ;
#10883 = AXIS2_PLACEMENT_3D ( 'NONE', #35006, #64986, #3566 ) ;
#10884 = CARTESIAN_POINT ( 'NONE',  ( 29.70435979725210274, -3.845442984095253536, 28.14021868772163160 ) ) ;
#10885 = CARTESIAN_POINT ( 'NONE',  ( -104.5895376238167245, -24.64898659630529210, 1.056161002820830142 ) ) ;
#10886 = ORIENTED_EDGE ( 'NONE', *, *, #93173, .T. ) ;
#10887 = DIRECTION ( 'NONE',  ( 0.000000000000000000, 0.000000000000000000, -1.000000000000000000 ) ) ;
#10888 = DIRECTION ( 'NONE',  ( 0.000000000000000000, -1.000000000000000000, 0.000000000000000000 ) ) ;
#10889 = CARTESIAN_POINT ( 'NONE',  ( -17.86878485216894319, -10.78119150571587781, -1.500000000000002220 ) ) ;
#10890 = ORIENTED_EDGE ( 'NONE', *, *, #16225, .T. ) ;
#10891 = EDGE_CURVE ( 'NONE', #53605, #68497, #28160, .T. ) ;
#10893 = ORIENTED_EDGE ( 'NONE', *, *, #39107, .F. ) ;
#10892 = DIRECTION ( 'NONE',  ( -3.773278334453079030E-23, 0.9999999999976377785, 2.173523156925979128E-06 ) ) ;
#10894 = AXIS2_PLACEMENT_3D ( 'NONE', #31314, #46547, #39434 ) ;
#10895 = VERTEX_POINT ( 'NONE', #75812 ) ;
#10896 = CARTESIAN_POINT ( 'NONE',  ( 3.421177667410919110, 6.376774720514426953, 28.69411518427638441 ) ) ;
#10897 = CARTESIAN_POINT ( 'NONE',  ( -5.295558097854481616, 20.35707381486366785, -1.500000000000002220 ) ) ;
#10898 = EDGE_CURVE ( 'NONE', #40542, #99855, #48455, .T. ) ;
#10899 = ORIENTED_EDGE ( 'NONE', *, *, #96526, .T. ) ;
#10900 = CARTESIAN_POINT ( 'NONE',  ( -0.02075734969026145696, 6.376774720514426953, -22.78097719988138081 ) ) ;
#10901 = CYLINDRICAL_SURFACE ( 'NONE', #48240, 0.3000000000000016542 ) ;
#10902 = CARTESIAN_POINT ( 'NONE',  ( -120.5896284256728990, -24.52399227489125266, 9.353111116836528183 ) ) ;
#10903 = CIRCLE ( 'NONE', #22246, 2.899999999999999467 ) ;
#10904 = CARTESIAN_POINT ( 'NONE',  ( -101.2262178754702120, -25.03152408370649340, 7.375461323086289767 ) ) ;
#10905 = CARTESIAN_POINT ( 'NONE',  ( -129.6228709571500701, -23.95044443724993144, 10.65354141964649948 ) ) ;
#10906 = CARTESIAN_POINT ( 'NONE',  ( 18.84366469573077296, 10.75509914293975555, -1.500000000000002220 ) ) ;
#10907 = CARTESIAN_POINT ( 'NONE',  ( -80.94627791849588050, -25.24759782953908527, 7.000535489368433062 ) ) ;
#10909 = ORIENTED_EDGE ( 'NONE', *, *, #69008, .T. ) ;
#10908 = CARTESIAN_POINT ( 'NONE',  ( 7.309977242446557888, -21.02818303981469583, 11.49999999999999645 ) ) ;
#10910 = CARTESIAN_POINT ( 'NONE',  ( -51.19842764437002813, -25.24728787901509008, 5.493892441256813974 ) ) ;
#10911 = FACE_OUTER_BOUND ( 'NONE', #94296, .T. ) ;
#10912 = EDGE_CURVE ( 'NONE', #11878, #39724, #37267, .T. ) ;
#10913 = CARTESIAN_POINT ( 'NONE',  ( -70.41980003698678559, -25.30157081653178608, 5.314949076439312137 ) ) ;
#10914 = EDGE_LOOP ( 'NONE', ( #90232, #23730, #66386, #33483 ) ) ;
#10916 = VERTEX_POINT ( 'NONE', #12422 ) ;
#10915 = LINE ( 'NONE', #57105, #53908 ) ;
#10917 = ORIENTED_EDGE ( 'NONE', *, *, #89712, .F. ) ;
#10918 = CARTESIAN_POINT ( 'NONE',  ( 30.32108885906865936, -5.356774720514427379, 3.274824222184972822 ) ) ;
#10919 = PRODUCT_DEFINITION ( 'UNKNOWN', '', #96051, #21544 ) ;
#10920 = DIRECTION ( 'NONE',  ( -0.000000000000000000, 1.000000000000000000, -0.000000000000000000 ) ) ;
#10921 = LINE ( 'NONE', #78915, #73270 ) ;
#10922 = ORIENTED_EDGE ( 'NONE', *, *, #89695, .T. ) ;
#10923 = CARTESIAN_POINT ( 'NONE',  ( -130.5728709571500872, -24.61548261799620363, 0.6545881806958654403 ) ) ;
#10924 = CARTESIAN_POINT ( 'NONE',  ( -11.68221627493902126, 19.09626523228051553, -1.500000000000002220 ) ) ;
#10925 = VERTEX_POINT ( 'NONE', #99145 ) ;
#10926 = CARTESIAN_POINT ( 'NONE',  ( -112.5587162177321972, -23.48786465467241769, 11.44779295918253936 ) ) ;
#10927 = CARTESIAN_POINT ( 'NONE',  ( -101.5603781230100680, -23.48786465467241413, 11.44779295918254469 ) ) ;
#10928 = CARTESIAN_POINT ( 'NONE',  ( -39.44687923781921057, -25.28830591450888221, 4.188173661249233959 ) ) ;
#10929 = AXIS2_PLACEMENT_3D ( 'NONE', #89026, #74294, #90512 ) ;
#10930 = CARTESIAN_POINT ( 'NONE',  ( -54.62287095715005592, -24.64898659630528854, 1.056161002820821038 ) ) ;
#10931 = CARTESIAN_POINT ( 'NONE',  ( -97.25305430158761055, -24.26827793580486059, 9.960784317162948653 ) ) ;
#10932 = CARTESIAN_POINT ( 'NONE',  ( 14.99095386781537975, 12.61000069877385421, -1.500000000000002220 ) ) ;
#10933 = B_SPLINE_SURFACE_WITH_KNOTS ( 'NONE', 3, 3, ( 
 ( #67236, #76801, #45392, #51998 ),
 ( #98149, #28163, #37764, #68721 ),
 ( #37270, #68222, #66748, #99149 ),
 ( #53509, #98651, #61115, #29649 ),
 ( #82436, #21029, #99639, #82929 ),
 ( #45886, #75318, #13417, #5813 ),
 ( #60122, #60623, #36276, #84432 ) ),
 .UNSPECIFIED., .F., .F., .F.,
 ( 4, 3, 4 ),
 ( 4, 4 ),
 ( 0.7945040050992252523, 0.8970133687736511208, 0.9995227324480769893 ),
 ( 0.9697404217223760670, 0.9712008428071842170 ),
 .UNSPECIFIED. ) ;
#10934 = DIRECTION ( 'NONE',  ( -0.06486421869277853025, 0.000000000000000000, 0.9978940991575085961 ) ) ;
#10935 = ORIENTED_EDGE ( 'NONE', *, *, #29623, .F. ) ;
#10936 = CARTESIAN_POINT ( 'NONE',  ( -5.740839400147730309, 20.75665450205591966, -1.500000000000002220 ) ) ;
#10937 = AXIS2_PLACEMENT_3D ( 'NONE', #49505, #65248, #26150 ) ;
#10938 = CARTESIAN_POINT ( 'NONE',  ( -128.5213307013914630, -24.65952944569305316, 1.056160979905708341 ) ) ;
#10940 = CARTESIAN_POINT ( 'NONE',  ( -71.30218710724507503, -25.12218970343873536, 6.299238622824248068 ) ) ;
#10939 = B_SPLINE_CURVE_WITH_KNOTS ( 'NONE', 3,
 ( #8649, #77640, #93877, #53331, #99477, #45215, #77139, #76141 ),
 .UNSPECIFIED., .F., .F.,
 ( 4, 2, 2, 4 ),
 ( 6.391158118962920407E-06, 0.002007136338672923116, 0.003007508928949902995, 0.004007881519226883307 ),
 .UNSPECIFIED. ) ;
#10941 = CARTESIAN_POINT ( 'NONE',  ( -63.55620429048339304, -24.66019654487199020, 8.947790411086131712 ) ) ;
#10943 = B_SPLINE_CURVE_WITH_KNOTS ( 'NONE', 3,
 ( #73595, #36019, #4085, #74581, #43152, #68968, #83183, #46141 ),
 .UNSPECIFIED., .F., .F.,
 ( 4, 2, 2, 4 ),
 ( 6.391158118963016122E-06, 0.002007136338672923983, 0.003007508928949904729, 0.004007881519226885042 ),
 .UNSPECIFIED. ) ;
#10942 = CARTESIAN_POINT ( 'NONE',  ( -82.52287095715006160, -24.65952944569304606, 1.056160979905698794 ) ) ;
#10944 = CARTESIAN_POINT ( 'NONE',  ( 22.25235761598246143, -5.642936543268669780, -1.500000000000002220 ) ) ;
#10945 = COORDINATED_UNIVERSAL_TIME_OFFSET ( 0, 0, .AHEAD. ) ;
#10946 = LINE ( 'NONE', #17553, #67753 ) ;
#10947 = CARTESIAN_POINT ( 'NONE',  ( -49.51416547925957445, -23.73766607897670156, -1.055555164236457566 ) ) ;
#10948 = CARTESIAN_POINT ( 'NONE',  ( -5.826506878040391690, 19.21762618028343184, 11.49999999999999645 ) ) ;
#10949 = CARTESIAN_POINT ( 'NONE',  ( -110.0261373028301080, -25.10927401252845925, 2.855322574578669670 ) ) ;
#10950 = CARTESIAN_POINT ( 'NONE',  ( -19.80875734969026425, -0.3587747205144265483, 31.02402280011862246 ) ) ;
#10951 = CYLINDRICAL_SURFACE ( 'NONE', #6856, 0.8160000000000007248 ) ;
#10952 = CARTESIAN_POINT ( 'NONE',  ( -113.6228709571500417, -23.48783264082479150, -1.443836473390060160 ) ) ;
#10953 = DIRECTION ( 'NONE',  ( 1.000000000000000000, 0.000000000000000000, 0.000000000000000000 ) ) ;
#10954 = CARTESIAN_POINT ( 'NONE',  ( -18.24533751216517885, 7.751685665592884078, -1.500000000000002220 ) ) ;
#10955 = CARTESIAN_POINT ( 'NONE',  ( 0.000000000000000000, 0.000000000000000000, 2.100000000000000089 ) ) ;
#10956 = CARTESIAN_POINT ( 'NONE',  ( -16.05533900033903549, 11.45903963230415101, -1.500000000000002220 ) ) ;
#10957 = VECTOR ( 'NONE', #70467, 1000.000000000000000 ) ;
#10958 = CARTESIAN_POINT ( 'NONE',  ( 0.2450472757604422180, -5.405843919193447533, 9.000000000000000000 ) ) ;
#10959 = DATE_AND_TIME ( #33796, #5139 ) ;
#10960 = EDGE_CURVE ( 'NONE', #73137, #42999, #51005, .T. ) ;
#10961 = CARTESIAN_POINT ( 'NONE',  ( 14.43441819135840376, 3.316774720514426456, -28.36222020317694970 ) ) ;
#10962 = CARTESIAN_POINT ( 'NONE',  ( 3.296033061219842519, -6.376774720514406525, 18.71226942120119574 ) ) ;
#10963 = CARTESIAN_POINT ( 'NONE',  ( 19.85042311639309531, 5.490197614093233369, 11.49999999999999645 ) ) ;
#10964 = ADVANCED_FACE ( 'NONE', ( #22014 ), #59615, .T. ) ;
#10965 = VECTOR ( 'NONE', #65934, 1000.000000000000000 ) ;
#10966 = CARTESIAN_POINT ( 'NONE',  ( 15.58962545129235799, 6.475225279485573360, -26.91365498785467025 ) ) ;
#10967 = CARTESIAN_POINT ( 'NONE',  ( -6.441999407266626676, 21.70310835763521595, 11.49999999999999645 ) ) ;
#10968 = VERTEX_POINT ( 'NONE', #51995 ) ;
#10969 = CARTESIAN_POINT ( 'NONE',  ( -69.70298246041917878, -25.12219101354323669, 6.901994799867971153 ) ) ;
#10970 = CARTESIAN_POINT ( 'NONE',  ( -97.51896588966310730, -23.73766607897671221, -1.055555164236451793 ) ) ;
#10971 = VECTOR ( 'NONE', #64615, 1000.000000000000114 ) ;
#10972 = EDGE_CURVE ( 'NONE', #34090, #40854, #89595, .T. ) ;
#10973 = CARTESIAN_POINT ( 'NONE',  ( -27.55559746109228669, -24.93063634460818889, 8.249644825981562235 ) ) ;
#10974 = CARTESIAN_POINT ( 'NONE',  ( -2.732037236150805626, -6.376774720514411854, 19.78976258633487717 ) ) ;
#10975 = B_SPLINE_CURVE_WITH_KNOTS ( 'NONE', 3,
 ( #26697, #71880, #87088, #41935, #95207, #72379 ),
 .UNSPECIFIED., .F., .F.,
 ( 4, 2, 4 ),
 ( 0.000000000000000000, 0.001380901958385388545, 0.002761803916770777089 ),
 .UNSPECIFIED. ) ;
#10976 = ORIENTED_EDGE ( 'NONE', *, *, #21336, .T. ) ;
#10977 = CARTESIAN_POINT ( 'NONE',  ( -79.34772585426964042, -25.31596430212281135, 5.924311783118726638 ) ) ;
#10978 = CARTESIAN_POINT ( 'NONE',  ( -15.12447472116105729, 17.10960193589383849, 11.49999999999998934 ) ) ;
#10979 = DIRECTION ( 'NONE',  ( 0.000000000000000000, -1.000000000000000000, 0.000000000000000000 ) ) ;
#10980 = FACE_OUTER_BOUND ( 'NONE', #20904, .T. ) ;
#10981 = CARTESIAN_POINT ( 'NONE',  ( -82.63662447401794964, -23.96169478059713143, 10.65365249895718414 ) ) ;
#10982 = CARTESIAN_POINT ( 'NONE',  ( 21.16529133594374557, -7.503415950508986576, 11.49999999999999645 ) ) ;
#10983 = ORIENTED_EDGE ( 'NONE', *, *, #97084, .F. ) ;
#10984 = CARTESIAN_POINT ( 'NONE',  ( -36.52287095715006870, -23.47596703998600631, 11.44779298504229281 ) ) ;
#10985 = CARTESIAN_POINT ( 'NONE',  ( 15.04091035147580335, -15.99806323810862274, -1.500000000000002220 ) ) ;
#10986 = CARTESIAN_POINT ( 'NONE',  ( -127.4336609825043070, -25.40057329150818077, 4.607792141311833234 ) ) ;
#10987 = CARTESIAN_POINT ( 'NONE',  ( -44.61594382116558677, -23.48786465467240347, 11.44779295918255180 ) ) ;
#10988 = CARTESIAN_POINT ( 'NONE',  ( -118.5228709571501184, -23.48783264082477373, -1.443836473390083475 ) ) ;
#10989 = ORIENTED_EDGE ( 'NONE', *, *, #84718, .T. ) ;
#10990 = CARTESIAN_POINT ( 'NONE',  ( 13.91401389203221406, 3.316774720514426456, 158.0376437107427137 ) ) ;
#10991 = CARTESIAN_POINT ( 'NONE',  ( -111.6228709571500559, -23.72747288104441665, -1.053458166803660889 ) ) ;
#10992 = EDGE_LOOP ( 'NONE', ( #69818, #63675, #36079, #61795 ) ) ;
#10993 = CARTESIAN_POINT ( 'NONE',  ( -45.52287095715004739, -24.82558206586142902, 1.605769216559445933 ) ) ;
#10994 = CARTESIAN_POINT ( 'NONE',  ( 7.908618202329199320, -18.92053725880622039, -1.500000000000002220 ) ) ;
#10995 = APPLICATION_CONTEXT ( 'configuration controlled 3d designs of mechanical parts and assemblies' ) ;
#10996 = ORIENTED_EDGE ( 'NONE', *, *, #73543, .T. ) ;
#10997 = ORIENTED_EDGE ( 'NONE', *, *, #32029, .T. ) ;
#10998 = ORIENTED_EDGE ( 'NONE', *, *, #26175, .T. ) ;
#10999 = CARTESIAN_POINT ( 'NONE',  ( -61.62287095715004881, -29.50247984919015209, -1.443849546365056913 ) ) ;
#11000 = CARTESIAN_POINT ( 'NONE',  ( 11.81885653190370888, -19.86314957129924608, 11.49999999999998934 ) ) ;
#11001 = CARTESIAN_POINT ( 'NONE',  ( -50.30128366834752995, -25.12097252146865145, 2.835025266119492571 ) ) ;
#11002 = CARTESIAN_POINT ( 'NONE',  ( 12.41260344771940360, 16.11316662856288318, -1.500000000000002220 ) ) ;
#11003 = ORIENTED_EDGE ( 'NONE', *, *, #33105, .T. ) ;
#11004 = VECTOR ( 'NONE', #23870, 1000.000000000000000 ) ;
#11005 = CARTESIAN_POINT ( 'NONE',  ( -43.52287095715007581, -23.47593901973090169, -1.443836447538997092 ) ) ;
#11006 = CARTESIAN_POINT ( 'NONE',  ( -29.65134514979727953, -23.88619203586730677, 10.65365256123546978 ) ) ;
#11007 = EDGE_CURVE ( 'NONE', #70027, #96494, #3707, .T. ) ;
#11008 = CARTESIAN_POINT ( 'NONE',  ( -105.5507901751989692, -24.52300882791530512, 0.6510814631126371488 ) ) ;
#11009 = CARTESIAN_POINT ( 'NONE',  ( 8.971512145086528278, -9.528487854913501920, 6.500000000000001776 ) ) ;
#11010 = ORIENTED_EDGE ( 'NONE', *, *, #76556, .T. ) ;
#11011 = CARTESIAN_POINT ( 'NONE',  ( -29.13856514152708499, -25.21531959831865066, 3.662308989302375029 ) ) ;
#11012 = CARTESIAN_POINT ( 'NONE',  ( -49.35320922236618912, -25.31573769575033594, 4.652611179520380169 ) ) ;
#11013 = ORIENTED_EDGE ( 'NONE', *, *, #80739, .F. ) ;
#11014 = CARTESIAN_POINT ( 'NONE',  ( -0.3852054317258338245, -20.75737367715079174, 11.49999999999998934 ) ) ;
#11016 = EDGE_CURVE ( 'NONE', #57584, #76588, #45389, .T. ) ;
#11015 = ORIENTED_EDGE ( 'NONE', *, *, #80822, .T. ) ;
#11018 = ORIENTED_EDGE ( 'NONE', *, *, #55162, .T. ) ;
#11017 = CARTESIAN_POINT ( 'NONE',  ( -125.5899157922687692, -24.40034930558991633, 0.3402023900116222244 ) ) ;
#11019 = B_SPLINE_SURFACE_WITH_KNOTS ( 'NONE', 3, 3, ( 
 ( #73202, #80807, #96523, #51355 ),
 ( #4185, #74678, #5668, #59467 ),
 ( #4685, #36127, #90408, #20883 ),
 ( #97024, #51857, #82790, #12274 ),
 ( #42271, #5172, #49875, #13270 ),
 ( #44246, #66608, #27523, #82295 ),
 ( #3690, #50365, #18894, #27019 ),
 ( #74192, #36618, #19888, #12773 ),
 ( #67587, #75174, #58973, #57985 ),
 ( #98504, #50862, #88422, #81301 ),
 ( #43743, #11786, #42756, #81799 ),
 ( #43252, #35633, #97518, #89912 ),
 ( #45732, #77663, #85286, #60478 ),
 ( #6662, #15774, #83286, #99499 ),
 ( #61967, #14264, #92393, #38109 ),
 ( #21375, #15270, #23371, #7667 ),
 ( #52847, #29995, #21871, #69065 ),
 ( #8171, #14766, #53852, #91394 ),
 ( #7160, #60969, #31000, #99990 ),
 ( #75663, #76656, #83786, #57 ),
 ( #6164, #45240, #91894, #84784 ),
 ( #30498, #22369, #92894, #61470 ),
 ( #37116, #22867, #76163, #54354 ),
 ( #68076, #37616, #53354, #46230 ),
 ( #39113, #70066, #38615, #99001 ) ),
 .UNSPECIFIED., .F., .F., .F.,
 ( 4, 3, 3, 3, 3, 3, 3, 3, 4 ),
 ( 4, 4 ),
 ( -9.884131503357096650E-16, 0.1249999999999991812, 0.1874999999999992784, 0.2499999999999993616, 0.4999999999999997224, 0.7500000000000001110, 0.8125000000000002220, 0.8750000000000002220, 1.000000000000000444 ),
 ( 0.000000000000000000, 1.000000000000000000 ),
 .UNSPECIFIED. ) ;
#11020 = DIRECTION ( 'NONE',  ( 0.000000000000000000, 0.000000000000000000, -1.000000000000000000 ) ) ;
#11021 = FACE_OUTER_BOUND ( 'NONE', #63830, .T. ) ;
#11022 = ORIENTED_EDGE ( 'NONE', *, *, #42355, .T. ) ;
#11023 = VERTEX_POINT ( 'NONE', #90054 ) ;
#11024 = B_SPLINE_CURVE_WITH_KNOTS ( 'NONE', 3,
 ( #64780, #21545, #44914, #12939, #20063, #4357, #59643, #60642 ),
 .UNSPECIFIED., .F., .F.,
 ( 4, 2, 2, 4 ),
 ( 0.000000000000000000, 0.002001079623178227563, 0.003001619434767338959, 0.004002159246356450789 ),
 .UNSPECIFIED. ) ;
#11025 = CARTESIAN_POINT ( 'NONE',  ( -78.62287095715005592, -24.34917612406838217, 0.1852690917426633999 ) ) ;
#11026 = CARTESIAN_POINT ( 'NONE',  ( 5.109298100548420152, 3.316774720514426456, -27.55941679637948383 ) ) ;
#11027 = CARTESIAN_POINT ( 'NONE',  ( -70.82359880940848029, -25.24515063934281400, 5.413474252732282110 ) ) ;
#11029 = ORIENTED_EDGE ( 'NONE', *, *, #78604, .F. ) ;
#11028 = CARTESIAN_POINT ( 'NONE',  ( 6.148021820315829444, -21.18842874637755358, 11.49999999999999645 ) ) ;
#11030 = B_SPLINE_CURVE_WITH_KNOTS ( 'NONE', 3,
 ( #25923, #19305, #25424, #55892, #64021, #2107, #65520, #40151, #48782, #10706, #50272, #71107, #79705, #18317, #41671, #11202, #49286, #63509, #24915 ),
 .UNSPECIFIED., .F., .F.,
 ( 4, 1, 1, 1, 1, 1, 1, 1, 1, 1, 1, 1, 1, 1, 1, 1, 4 ),
 ( 0.000000000000000000, 0.06113791491562318298, 0.1199938438512138800, 0.1782253215076183839, 0.2362564202618999687, 0.2949293769549112820, 0.3547157488097555933, 0.4167296639241647727, 0.4806644084708298625, 0.5458317702108677061, 0.6097581054261674849, 0.6729712284742227490, 0.7360168691676642894, 0.7998393981920319806, 0.8647753566655687063, 0.9310876232725688872, 1.000000000000000000 ),
 .UNSPECIFIED. ) ;
#11031 = CARTESIAN_POINT ( 'NONE',  ( -101.6228709571500701, -23.47596703998600631, 11.44779298504227683 ) ) ;
#11032 = CARTESIAN_POINT ( 'NONE',  ( -15.94491270116497184, -16.04792668696150315, -1.500000000000002220 ) ) ;
#11033 = AXIS2_PLACEMENT_3D ( 'NONE', #58134, #28663, #43403 ) ;
#11035 = EDGE_LOOP ( 'NONE', ( #72039, #94090, #55209, #65559 ) ) ;
#11034 = CARTESIAN_POINT ( 'NONE',  ( -24.90875734969025501, 6.376774720514426953, 26.43402280011862615 ) ) ;
#11036 = ORIENTED_EDGE ( 'NONE', *, *, #22488, .T. ) ;
#11037 = PLANE ( 'NONE',  #100045 ) ;
#11038 = EDGE_CURVE ( 'NONE', #45187, #50718, #20526, .T. ) ;
#11039 = AXIS2_PLACEMENT_3D ( 'NONE', #45820, #54937, #23451 ) ;
#11040 = CC_DESIGN_DATE_AND_TIME_ASSIGNMENT ( #51012, #81948, ( #68385 ) ) ;
#11041 = DIRECTION ( 'NONE',  ( 0.000000000000000000, 1.000000000000000000, -0.000000000000000000 ) ) ;
#11042 = EDGE_LOOP ( 'NONE', ( #12826, #44946, #32367, #16472 ) ) ;
#11043 = CARTESIAN_POINT ( 'NONE',  ( -6.524719417830534773, 20.15472526627327454, -1.500000000000002220 ) ) ;
#11044 = CARTESIAN_POINT ( 'NONE',  ( -78.95422500253870624, -25.27791675628532531, 6.195240761392555306 ) ) ;
#11045 = VECTOR ( 'NONE', #79963, 1000.000000000000114 ) ;
#11046 = CARTESIAN_POINT ( 'NONE',  ( -125.6228709571500843, -24.51163499207175533, 0.6490370598554157100 ) ) ;
#11047 = CARTESIAN_POINT ( 'NONE',  ( -39.58953762381673158, -23.47593901973091235, -1.443836447539011525 ) ) ;
#11048 = CARTESIAN_POINT ( 'NONE',  ( 22.14152233036116257, 1.636640089565777334, -1.500000000000002220 ) ) ;
#11049 = CARTESIAN_POINT ( 'NONE',  ( -49.25033725972690490, -25.13941398251548875, 7.108518452791937392 ) ) ;
#11050 = VERTEX_POINT ( 'NONE', #46878 ) ;
#11051 = LINE ( 'NONE', #63362, #75684 ) ;
#11052 = CARTESIAN_POINT ( 'NONE',  ( 2.750000000000001332, 26.59999999999999432, 0.000000000000000000 ) ) ;
#11053 = EDGE_CURVE ( 'NONE', #81664, #90864, #2448, .T. ) ;
#11054 = CARTESIAN_POINT ( 'NONE',  ( -24.90875734969025501, -5.356774720514425603, 27.45402280011862572 ) ) ;
#11055 = DIRECTION ( 'NONE',  ( -1.000000000000000000, 0.000000000000000000, 5.238131417152343399E-15 ) ) ;
#11057 = VECTOR ( 'NONE', #3724, 1000.000000000000000 ) ;
#11056 = CARTESIAN_POINT ( 'NONE',  ( 4.731349760756693890, 18.90081699332259646, -1.500000000000002220 ) ) ;
#11058 = CARTESIAN_POINT ( 'NONE',  ( -20.52298544035203776, 6.160189734329080125, 11.49999999999998934 ) ) ;
#11059 = CARTESIAN_POINT ( 'NONE',  ( -0.6735982426299428338, -6.376774720514411854, 19.16400979764068069 ) ) ;
#11060 = DIRECTION ( 'NONE',  ( -3.773278334453079030E-23, 0.9999999999976377785, 2.173523156925979128E-06 ) ) ;
#11061 = CARTESIAN_POINT ( 'NONE',  ( -77.51696571866160923, -23.73766607897670156, -1.055555164236459564 ) ) ;
#11062 = CARTESIAN_POINT ( 'NONE',  ( -9.230423729802735622, -20.81519635545753033, -1.500000000000002220 ) ) ;
#11063 = CARTESIAN_POINT ( 'NONE',  ( 0.000000000000000000, 0.000000000000000000, 0.000000000000000000 ) ) ;
#11064 = CARTESIAN_POINT ( 'NONE',  ( -102.6362846996450173, -23.48783264082478439, -1.443836473390064601 ) ) ;
#11065 = DIRECTION ( 'NONE',  ( -1.000000000000000000, -0.000000000000000000, -0.000000000000000000 ) ) ;
#11066 = CARTESIAN_POINT ( 'NONE',  ( 14.98761344906185577, -13.09354923471379983, 11.49999999999999645 ) ) ;
#11067 = DIRECTION ( 'NONE',  ( 3.773278334444166432E-23, -1.000000000000000000, 0.000000000000000000 ) ) ;
#11068 = CARTESIAN_POINT ( 'NONE',  ( -89.23534077628077910, -25.27880950044346164, 5.947789066509455935 ) ) ;
#11069 = DIRECTION ( 'NONE',  ( 0.000000000000000000, -1.000000000000000000, 0.000000000000000000 ) ) ;
#11070 = EDGE_CURVE ( 'NONE', #45914, #71192, #47380, .T. ) ;
#11071 = EDGE_LOOP ( 'NONE', ( #87359, #98959, #85884, #25926 ) ) ;
#11072 = LINE ( 'NONE', #26298, #16941 ) ;
#11073 = CARTESIAN_POINT ( 'NONE',  ( -37.52287095715006870, -29.50248528299804818, 1.056150453629031594 ) ) ;
#11074 = CARTESIAN_POINT ( 'NONE',  ( 16.98214085172422827, 13.50221961261776293, -1.500000000000002220 ) ) ;
#11075 = CARTESIAN_POINT ( 'NONE',  ( -93.55620429048339304, -24.65952944569304606, 1.056160979905701902 ) ) ;
#11076 = CARTESIAN_POINT ( 'NONE',  ( 2.510080532074158377, -19.39449211012750496, -1.500000000000002220 ) ) ;
#11077 = FACE_OUTER_BOUND ( 'NONE', #91033, .T. ) ;
#11078 = ORIENTED_EDGE ( 'NONE', *, *, #5798, .T. ) ;
#11079 = CONTEXT_DEPENDENT_SHAPE_REPRESENTATION ( #16173, #73355 ) ;
#11080 = CARTESIAN_POINT ( 'NONE',  ( -69.86226385320381382, -29.50248914370730091, 2.832395270851967073 ) ) ;
#11081 = CARTESIAN_POINT ( 'NONE',  ( 17.75789855128238770, 10.12834119215567164, 11.49999999999999645 ) ) ;
#11082 = CARTESIAN_POINT ( 'NONE',  ( -85.55620429048340725, -23.47593901973091235, -1.443836447539002865 ) ) ;
#11083 = ADVANCED_FACE ( 'NONE', ( #61112 ), #15911, .F. ) ;
#11084 = FACE_OUTER_BOUND ( 'NONE', #49818, .T. ) ;
#11085 = ORIENTED_EDGE ( 'NONE', *, *, #78638, .T. ) ;
#11086 = PLANE ( 'NONE',  #99367 ) ;
#11087 = CARTESIAN_POINT ( 'NONE',  ( -84.62287095715005592, -29.50250243563736774, 8.947779886222141599 ) ) ;
#11088 = DIRECTION ( 'NONE',  ( -0.9685340172660600322, 0.000000000000000000, 0.2488812114211667037 ) ) ;
#11089 = EDGE_CURVE ( 'NONE', #53102, #85507, #8309, .T. ) ;
#11090 = DIRECTION ( 'NONE',  ( -0.8246584009594636333, -1.974890369949422540E-15, 0.5656310827093757876 ) ) ;
#11091 = ORIENTED_EDGE ( 'NONE', *, *, #40629, .F. ) ;
#11092 = CARTESIAN_POINT ( 'NONE',  ( -42.58953762381671737, -24.65952944569304250, 1.056160979905689024 ) ) ;
#11093 = CIRCLE ( 'NONE', #74327, 27.94799999999999685 ) ;
#11094 = CARTESIAN_POINT ( 'NONE',  ( 13.56796309060646166, -18.52494293750034871, 11.49999999999999645 ) ) ;
#11095 = CARTESIAN_POINT ( 'NONE',  ( 16.48639501038195121, -15.69157857782056276, 11.49999999999998934 ) ) ;
#11096 = CARTESIAN_POINT ( 'NONE',  ( -110.5518226189701494, -24.52399227489124556, 9.353111116836533512 ) ) ;
#11097 = CARTESIAN_POINT ( 'NONE',  ( -75.62287095715007013, -24.15516710230293995, 10.28746687063726384 ) ) ;
#11098 = CARTESIAN_POINT ( 'NONE',  ( 10.11708146329084457, 0.6683258531633596844, 18.35000000000000142 ) ) ;
#11099 = CARTESIAN_POINT ( 'NONE',  ( -54.52287095715005449, -24.34917612406836795, 0.1852690917426491890 ) ) ;
#11100 = CARTESIAN_POINT ( 'NONE',  ( -86.62287095715001328, -23.47596703998600631, 11.44779298504227683 ) ) ;
#11101 = CARTESIAN_POINT ( 'NONE',  ( -4.983756199382824548, -21.29032736245130053, 11.49999999999998934 ) ) ;
#11102 = CARTESIAN_POINT ( 'NONE',  ( -69.49771156051228616, -24.51419770103157347, 9.386484678747178734 ) ) ;
#11103 = CARTESIAN_POINT ( 'NONE',  ( -26.11680270647584479, -24.94521091305072957, 4.366544573346394564 ) ) ;
#11104 = CARTESIAN_POINT ( 'NONE',  ( -28.52287095715005805, -24.48836230353387222, 1.056161703005638719 ) ) ;
#11105 = CARTESIAN_POINT ( 'NONE',  ( -47.92287095715006018, -23.47593901973090169, -1.443836447538997980 ) ) ;
#11106 = ORIENTED_EDGE ( 'NONE', *, *, #74234, .F. ) ;
#11107 = VECTOR ( 'NONE', #16071, 1000.000000000000000 ) ;
#11108 = CARTESIAN_POINT ( 'NONE',  ( -13.80512455850298714, -15.04058748057734896, 11.49999999999998934 ) ) ;
#11109 = ORIENTED_EDGE ( 'NONE', *, *, #15364, .T. ) ;
#11110 = VERTEX_POINT ( 'NONE', #92042 ) ;
#11111 = ORIENTED_EDGE ( 'NONE', *, *, #6485, .F. ) ;
#11112 = CARTESIAN_POINT ( 'NONE',  ( 14.87233727408824713, -17.56007624320114857, 11.49999999999998934 ) ) ;
#11113 = DIRECTION ( 'NONE',  ( 0.000000000000000000, 0.000000000000000000, 1.000000000000000000 ) ) ;
#11114 = CARTESIAN_POINT ( 'NONE',  ( 17.97931717627152182, 9.192180251422895410, -1.500000000000002220 ) ) ;
#11115 = ORIENTED_EDGE ( 'NONE', *, *, #51635, .F. ) ;
#11116 = CARTESIAN_POINT ( 'NONE',  ( -0.02075734969026423599, -6.376774720514426953, -28.03397719988137382 ) ) ;
#11117 = CARTESIAN_POINT ( 'NONE',  ( -48.52287095715006870, -23.73934037231757088, 11.05740245334328620 ) ) ;
#11118 = CARTESIAN_POINT ( 'NONE',  ( -77.62287095715005592, -29.50248528299804818, 1.056150453629038477 ) ) ;
#11119 = CARTESIAN_POINT ( 'NONE',  ( -53.52206042989558199, -23.48786465467240703, 11.44779295918255002 ) ) ;
#11120 = AXIS2_PLACEMENT_3D ( 'NONE', #19937, #42804, #95572 ) ;
#11122 = ORIENTED_EDGE ( 'NONE', *, *, #21262, .T. ) ;
#11121 = CARTESIAN_POINT ( 'NONE',  ( -15.06583839362908961, -15.15408912208086534, 11.49999999999999645 ) ) ;
#11123 = CARTESIAN_POINT ( 'NONE',  ( 6.555906488453394410, -5.876774720514426065, 21.46941147007026274 ) ) ;
#11124 = ORIENTED_EDGE ( 'NONE', *, *, #94048, .T. ) ;
#11125 = CARTESIAN_POINT ( 'NONE',  ( 21.15429367616652101, -6.912965584596229895, -1.500000000000002220 ) ) ;
#11126 = CARTESIAN_POINT ( 'NONE',  ( -20.51892249978613236, 2.527598752449112585, 11.49999999999998934 ) ) ;
#11127 = B_SPLINE_CURVE_WITH_KNOTS ( 'NONE', 3,
 ( #69204, #39247, #78302, #92531, #45386, #85931 ),
 .UNSPECIFIED., .F., .F.,
 ( 4, 2, 4 ),
 ( 6.391158118964603462E-06, 0.001387004593080780291, 0.002767618028042595924 ),
 .UNSPECIFIED. ) ;
#11128 = B_SPLINE_CURVE_WITH_KNOTS ( 'NONE', 3,
 ( #99867, #55238, #24755, #53730 ),
 .UNSPECIFIED., .F., .F.,
 ( 4, 4 ),
 ( 0.000000000000000000, 1.000000000000000000 ),
 .UNSPECIFIED. ) ;
#11129 = ORIENTED_EDGE ( 'NONE', *, *, #25739, .T. ) ;
#11130 = EDGE_CURVE ( 'NONE', #91517, #6225, #54487, .T. ) ;
#11131 = CARTESIAN_POINT ( 'NONE',  ( -6.020540257910568904, -5.876774720514411854, 19.49847411603315095 ) ) ;
#11132 = DIRECTION ( 'NONE',  ( -3.773278334453079030E-23, 0.9999999999976377785, 2.173523156925979128E-06 ) ) ;
#11133 = ORIENTED_EDGE ( 'NONE', *, *, #49549, .T. ) ;
#11134 = CARTESIAN_POINT ( 'NONE',  ( -129.5228709571500758, -24.33832256527049154, 0.1851278514138698372 ) ) ;
#11135 = ORIENTED_EDGE ( 'NONE', *, *, #81727, .T. ) ;
#11136 = CARTESIAN_POINT ( 'NONE',  ( 5.097264368844749427, -3.316774720514425567, -27.56135813788841560 ) ) ;
#11137 = CARTESIAN_POINT ( 'NONE',  ( -8.544475976622297964, 19.10969517993760292, -1.500000000000002220 ) ) ;
#11138 = CARTESIAN_POINT ( 'NONE',  ( -6.542779104410481494, 20.88585256366161502, 11.49999999999999645 ) ) ;
#11139 = CARTESIAN_POINT ( 'NONE',  ( -73.62362711126294812, -24.66019654487200441, 8.947790411086119278 ) ) ;
#11140 = CARTESIAN_POINT ( 'NONE',  ( -5.125883829288005344, 21.89707322345674712, 11.49999999999998934 ) ) ;
#11141 = CARTESIAN_POINT ( 'NONE',  ( 11.32296221242833667, -17.63459971646239310, -1.500000000000002220 ) ) ;
#11142 = LINE ( 'NONE', #42115, #40047 ) ;
#11143 = DIRECTION ( 'NONE',  ( 0.000000000000000000, -1.000000000000000000, 0.000000000000000000 ) ) ;
#11144 = CARTESIAN_POINT ( 'NONE',  ( -82.62287095715005592, -23.48786465467241413, 11.44779295918254647 ) ) ;
#11145 = ORIENTED_EDGE ( 'NONE', *, *, #14850, .F. ) ;
#11146 = ORIENTED_EDGE ( 'NONE', *, *, #45361, .F. ) ;
#11147 = ORIENTED_EDGE ( 'NONE', *, *, #86871, .T. ) ;
#11148 = DIRECTION ( 'NONE',  ( -0.000000000000000000, 1.000000000000000000, -0.000000000000000000 ) ) ;
#11149 = VERTEX_POINT ( 'NONE', #31638 ) ;
#11150 = EDGE_CURVE ( 'NONE', #15127, #57287, #62310, .T. ) ;
#11151 = CARTESIAN_POINT ( 'NONE',  ( 4.431377227695222132, -20.94745169971119481, -1.500000000000002220 ) ) ;
#11152 = ORIENTED_EDGE ( 'NONE', *, *, #17456, .T. ) ;
#11153 = CARTESIAN_POINT ( 'NONE',  ( 0.3910256410256394144, -6.376774720514411854, 19.63681891025641235 ) ) ;
#11154 = EDGE_CURVE ( 'NONE', #37020, #72403, #55866, .T. ) ;
#11155 = CARTESIAN_POINT ( 'NONE',  ( 20.24497096899912307, 5.935080660949433096, -1.500000000000002220 ) ) ;
#11156 = CARTESIAN_POINT ( 'NONE',  ( -30.43335359600822798, -24.47651708652394831, 9.440108529385041081 ) ) ;
#11157 = CARTESIAN_POINT ( 'NONE',  ( 2.627412086454235851, -6.376774720514420736, 20.59155478446653831 ) ) ;
#11159 = CARTESIAN_POINT ( 'NONE',  ( -50.53932727748372145, -24.52399227489126687, 9.353111116836522854 ) ) ;
#11158 = VECTOR ( 'NONE', #5740, 1000.000000000000000 ) ;
#11160 = LINE ( 'NONE', #87792, #26462 ) ;
#11161 = CARTESIAN_POINT ( 'NONE',  ( -129.6235275842055614, -24.51419770103158058, 9.386484678747178734 ) ) ;
#11162 = CARTESIAN_POINT ( 'NONE',  ( 15.63414672909509839, 15.54323407889855879, -1.500000000000002220 ) ) ;
#11163 = EDGE_LOOP ( 'NONE', ( #21112, #2245, #61927, #34709 ) ) ;
#11164 = CARTESIAN_POINT ( 'NONE',  ( -65.63884284507189193, -24.40133493613049964, 9.663955038902800609 ) ) ;
#11165 = B_SPLINE_CURVE_WITH_KNOTS ( 'NONE', 3,
 ( #3996, #34937, #27822, #11591 ),
 .UNSPECIFIED., .F., .F.,
 ( 4, 4 ),
 ( 0.2199429803762241731, 0.2289494116483397346 ),
 .UNSPECIFIED. ) ;
#11166 = CYLINDRICAL_SURFACE ( 'NONE', #36809, 3.500000000000000000 ) ;
#11167 = CARTESIAN_POINT ( 'NONE',  ( -63.62287095715004881, -23.47593901973091235, -1.443836447539007972 ) ) ;
#11168 = ADVANCED_FACE ( 'NONE', ( #196 ), #61150, .T. ) ;
#11169 = AXIS2_PLACEMENT_3D ( 'NONE', #3523, #12112, #43085 ) ;
#11170 = EDGE_CURVE ( 'NONE', #45447, #34154, #8553, .T. ) ;
#11171 = CARTESIAN_POINT ( 'NONE',  ( -26.96874452920905085, -24.58296376597837707, 8.290116722409051064 ) ) ;
#11172 = CARTESIAN_POINT ( 'NONE',  ( 32.25249349869195470, -1.682774720514426114, -12.65342752644894553 ) ) ;
#11173 = ADVANCED_FACE ( 'NONE', ( #83256 ), #89877, .T. ) ;
#11175 = DIRECTION ( 'NONE',  ( 0.000000000000000000, 1.000000000000000000, 0.000000000000000000 ) ) ;
#11174 = CIRCLE ( 'NONE', #67897, 24.00000000000000000 ) ;
#11176 = CARTESIAN_POINT ( 'NONE',  ( 21.32124590881793225, -1.116183810207903804, -1.500000000000002220 ) ) ;
#11177 = CARTESIAN_POINT ( 'NONE',  ( -92.52287095715006160, -23.47596703998600631, 11.44779298504228393 ) ) ;
#11178 = CARTESIAN_POINT ( 'NONE',  ( -34.62287095715005592, -23.47593901973091235, -1.443836447539013301 ) ) ;
#11179 = DIRECTION ( 'NONE',  ( 1.000000000000000000, 3.773278334444166432E-23, 8.201307841325785021E-29 ) ) ;
#11180 = CARTESIAN_POINT ( 'NONE',  ( 0.2746452767749877344, 3.927610442141366676, 1.700000000000008615 ) ) ;
#11181 = CARTESIAN_POINT ( 'NONE',  ( 10.27952223434480494, 20.12118371629609470, -1.500000000000002220 ) ) ;
#11182 = CARTESIAN_POINT ( 'NONE',  ( 8.160000000000000142, -10.15233964170348457, 0.003711184059992174607 ) ) ;
#11183 = ORIENTED_EDGE ( 'NONE', *, *, #49168, .T. ) ;
#11184 = DIRECTION ( 'NONE',  ( 0.000000000000000000, 0.000000000000000000, 1.000000000000000000 ) ) ;
#11185 = CARTESIAN_POINT ( 'NONE',  ( -79.60526328347016545, -23.48783264082476308, -1.443836473390096575 ) ) ;
#11186 = CARTESIAN_POINT ( 'NONE',  ( 15.11087362536062173, -12.71848776332401521, 11.49999999999999645 ) ) ;
#11187 = FACE_BOUND ( 'NONE', #74900, .T. ) ;
#11188 = CARTESIAN_POINT ( 'NONE',  ( -96.58953762381672448, -23.47593901973091235, -1.443836447539001089 ) ) ;
#11189 = EDGE_CURVE ( 'NONE', #50453, #40343, #71465, .T. ) ;
#11190 = EDGE_LOOP ( 'NONE', ( #24962, #4404, #10736, #22824 ) ) ;
#11191 = CARTESIAN_POINT ( 'NONE',  ( -117.5895376238167103, -24.65952944569305316, 1.056160979905702790 ) ) ;
#11192 = LINE ( 'NONE', #20281, #33486 ) ;
#11193 = CARTESIAN_POINT ( 'NONE',  ( -100.5528973737291238, -25.12268565405453913, 7.099974650722071345 ) ) ;
#11194 = CARTESIAN_POINT ( 'NONE',  ( 17.58597629297885589, -12.55149374826878272, 11.49999999999998934 ) ) ;
#11195 = CARTESIAN_POINT ( 'NONE',  ( -71.62287095715005592, -23.47596703998600631, 11.44779298504227683 ) ) ;
#11196 = CARTESIAN_POINT ( 'NONE',  ( -66.52287095715010423, -24.51387760970724727, 9.387446482453405849 ) ) ;
#11197 = DIRECTION ( 'NONE',  ( -0.000000000000000000, -1.000000000000000000, -0.000000000000000000 ) ) ;
#11198 = CARTESIAN_POINT ( 'NONE',  ( -118.5562042904833930, -24.64965694238575367, 8.947790433994192938 ) ) ;
#11199 = CARTESIAN_POINT ( 'NONE',  ( -16.30015253881794379, -11.17962500214296639, -1.500000000000002220 ) ) ;
#11200 = ORIENTED_EDGE ( 'NONE', *, *, #29130, .T. ) ;
#11201 = CARTESIAN_POINT ( 'NONE',  ( -15.58492919356500650, -12.95507736684500699, 11.49999999999999645 ) ) ;
#11202 = CARTESIAN_POINT ( 'NONE',  ( 6.273728352332436309, -5.876774720514416295, 20.10092598260902008 ) ) ;
#11203 = EDGE_CURVE ( 'NONE', #80239, #96754, #714, .T. ) ;
#11204 = EDGE_CURVE ( 'NONE', #83628, #45754, #22339, .T. ) ;
#11205 = ORIENTED_EDGE ( 'NONE', *, *, #66550, .F. ) ;
#11206 = CARTESIAN_POINT ( 'NONE',  ( -40.58953762381673158, -23.47593901973091235, -1.443836447539011525 ) ) ;
#11207 = DIRECTION ( 'NONE',  ( 1.000000000000000000, -0.000000000000000000, 0.000000000000000000 ) ) ;
#11208 = DIRECTION ( 'NONE',  ( -1.000000000000000000, -1.232047923278981953E-16, 0.000000000000000000 ) ) ;
#11209 = CARTESIAN_POINT ( 'NONE',  ( -82.62287095715005592, -23.94994826722566117, -0.6494450866342736939 ) ) ;
#11210 = CARTESIAN_POINT ( 'NONE',  ( -39.62287095715008434, -24.51283580621364777, 0.6167428607019764808 ) ) ;
#11211 = CARTESIAN_POINT ( 'NONE',  ( -96.52287095715006160, -24.51283580621364422, 0.6167428607019779241 ) ) ;
#11212 = CARTESIAN_POINT ( 'NONE',  ( 19.28819943863484454, -5.468471092112969778, -1.500000000000002220 ) ) ;
#11213 = EDGE_CURVE ( 'NONE', #98513, #63968, #66623, .T. ) ;
#11214 = FACE_OUTER_BOUND ( 'NONE', #19629, .T. ) ;
#11215 = ORIENTED_EDGE ( 'NONE', *, *, #82072, .F. ) ;
#11216 = EDGE_CURVE ( 'NONE', #16993, #6143, #31543, .T. ) ;
#11217 = EDGE_CURVE ( 'NONE', #14515, #54685, #94446, .T. ) ;
#11218 = DIRECTION ( 'NONE',  ( -0.1311553622875928082, 6.454799914155188842E-16, -0.9913618264504692190 ) ) ;
#11219 = CARTESIAN_POINT ( 'NONE',  ( -33.62287095715007013, -24.51283580621364422, 0.6167428607019749265 ) ) ;
#11220 = CARTESIAN_POINT ( 'NONE',  ( -63.58953762381672448, -24.64965694238575011, 8.947790433994200043 ) ) ;
#11221 = CARTESIAN_POINT ( 'NONE',  ( -23.59123376470063960, -5.356774720514425603, 24.50402280011862288 ) ) ;
#11222 = CARTESIAN_POINT ( 'NONE',  ( -103.5228709571501184, -24.51283580621365843, 0.6167428607019787012 ) ) ;
#11223 = CARTESIAN_POINT ( 'NONE',  ( 14.97568007497113385, 3.504021928054863899, -28.39450375387846748 ) ) ;
#11224 = CARTESIAN_POINT ( 'NONE',  ( -51.54161239871793043, -25.23256535379771037, 6.480020017899467355 ) ) ;
#11225 = VERTEX_POINT ( 'NONE', #53504 ) ;
#11226 = AXIS2_PLACEMENT_3D ( 'NONE', #22062, #100168, #37314 ) ;
#11227 = CARTESIAN_POINT ( 'NONE',  ( -19.79944955726156763, -4.570829099900970860, -1.500000000000002220 ) ) ;
#11228 = ORIENTED_EDGE ( 'NONE', *, *, #79879, .F. ) ;
#11229 = CARTESIAN_POINT ( 'NONE',  ( -4.681240387505234857, -22.43558246840685300, -1.500000000000002220 ) ) ;
#11230 = CARTESIAN_POINT ( 'NONE',  ( 31.63187483939985256, 3.931892516571728446, 27.18445229901795557 ) ) ;
#11231 = CARTESIAN_POINT ( 'NONE',  ( -127.6240570307130611, -24.15620529776628800, 10.23563542870658871 ) ) ;
#11232 = ORIENTED_EDGE ( 'NONE', *, *, #15332, .T. ) ;
#11233 = CARTESIAN_POINT ( 'NONE',  ( -4.621320343559618848, 12.50000000000004974, 0.000000000000000000 ) ) ;
#11234 = CARTESIAN_POINT ( 'NONE',  ( 15.32643653063177958, 3.577630190450218350, -27.14485409495429380 ) ) ;
#11235 = VECTOR ( 'NONE', #45944, 1000.000000000000227 ) ;
#11236 = CARTESIAN_POINT ( 'NONE',  ( -30.47287095715006799, -24.05195403655357111, -0.4597278507670095604 ) ) ;
#11237 = CARTESIAN_POINT ( 'NONE',  ( -15.86343167427570577, 14.10970434637795634, 11.49999999999999645 ) ) ;
#11238 = VECTOR ( 'NONE', #77602, 1000.000000000000000 ) ;
#11239 = CARTESIAN_POINT ( 'NONE',  ( 22.15222936869060177, 0.07132910108538677296, 11.49999999999998934 ) ) ;
#11240 = CARTESIAN_POINT ( 'NONE',  ( 10.54205562766345672, -17.70522803435136083, -1.500000000000002220 ) ) ;
#11242 = ORIENTED_EDGE ( 'NONE', *, *, #13810, .F. ) ;
#11241 = VECTOR ( 'NONE', #58699, 1000.000000000000000 ) ;
#11243 = CARTESIAN_POINT ( 'NONE',  ( -111.5228709571500190, -23.48783264082477018, -1.443836473390084585 ) ) ;
#11244 = EDGE_LOOP ( 'NONE', ( #59487, #28475, #64691, #63639, #78523 ) ) ;
#11245 = CARTESIAN_POINT ( 'NONE',  ( 30.32108885906865936, -4.540774720514427543, 3.274824222184972822 ) ) ;
#11246 = CARTESIAN_POINT ( 'NONE',  ( -10.58858228176428717, -5.965225279485594001, -27.03148018517017093 ) ) ;
#11247 = VERTEX_POINT ( 'NONE', #16917 ) ;
#11248 = EDGE_LOOP ( 'NONE', ( #80145, #45362, #46306, #37498 ) ) ;
#11249 = ORIENTED_EDGE ( 'NONE', *, *, #82364, .F. ) ;
#11250 = DIRECTION ( 'NONE',  ( 0.000000000000000000, 0.000000000000000000, 1.000000000000000000 ) ) ;
#11251 = CARTESIAN_POINT ( 'NONE',  ( -61.24303308397303880, -29.50249942614373921, 7.563164501610022405 ) ) ;
#11252 = CARTESIAN_POINT ( 'NONE',  ( 5.327901167172695907, -5.876774720514418071, 20.73192761314082233 ) ) ;
#11253 = CARTESIAN_POINT ( 'NONE',  ( -9.423985339279758122, -18.44656043379632848, -1.500000000000002220 ) ) ;
#11254 = CARTESIAN_POINT ( 'NONE',  ( 19.97611268498323511, -8.487024919450899318, 11.49999999999999645 ) ) ;
#11255 = ORIENTED_EDGE ( 'NONE', *, *, #40684, .T. ) ;
#11256 = CARTESIAN_POINT ( 'NONE',  ( 8.160000000000000142, -10.15233964170348457, 0.003711184059992174607 ) ) ;
#11257 = DIRECTION ( 'NONE',  ( -0.9952638024365005887, 0.000000000000000000, -0.09721092304694052555 ) ) ;
#11258 = CARTESIAN_POINT ( 'NONE',  ( 11.21425909587273928, 19.38466839394011387, -1.500000000000002220 ) ) ;
#11259 = CARTESIAN_POINT ( 'NONE',  ( -124.5562042904833930, -23.48783264082478794, -1.443836473390058384 ) ) ;
#11260 = CARTESIAN_POINT ( 'NONE',  ( -61.55620429048339304, -24.64965694238573946, 8.947790433994205372 ) ) ;
#11261 = ORIENTED_EDGE ( 'NONE', *, *, #29836, .T. ) ;
#11262 = CARTESIAN_POINT ( 'NONE',  ( 29.77147767949874435, 6.376774720514426953, 26.15915692125051706 ) ) ;
#11263 = CARTESIAN_POINT ( 'NONE',  ( 12.67628326092776803, -4.091305608280291217, -27.97525530010125294 ) ) ;
#11264 = ORIENTED_EDGE ( 'NONE', *, *, #29489, .F. ) ;
#11265 = ORIENTED_EDGE ( 'NONE', *, *, #32838, .T. ) ;
#11266 = CARTESIAN_POINT ( 'NONE',  ( -112.5228709571500616, -24.66019654487200441, 8.947790411086108620 ) ) ;
#11267 = ORIENTED_EDGE ( 'NONE', *, *, #6109, .F. ) ;
#11268 = ADVANCED_FACE ( 'NONE', ( #23508, #63113 ), #32642, .T. ) ;
#11269 = CARTESIAN_POINT ( 'NONE',  ( -15.86343167427570577, 14.10970434637795634, -1.500000000000002220 ) ) ;
#11270 = EDGE_LOOP ( 'NONE', ( #7209, #46255, #25584, #28137 ) ) ;
#11271 = DIRECTION ( 'NONE',  ( -0.000000000000000000, -1.000000000000000000, -0.000000000000000000 ) ) ;
#11272 = ADVANCED_FACE ( 'NONE', ( #47880 ), #85933, .F. ) ;
#11273 = CARTESIAN_POINT ( 'NONE',  ( 3.337383349182757364, -21.60657791699550856, -1.500000000000002220 ) ) ;
#11274 = CARTESIAN_POINT ( 'NONE',  ( -103.6332108804325571, -23.73791477778911840, 11.05961554403170410 ) ) ;
#11275 = DIRECTION ( 'NONE',  ( -0.09721092304694055330, 0.000000000000000000, 0.9952638024365006997 ) ) ;
#11276 = CARTESIAN_POINT ( 'NONE',  ( 5.557675543255346184, -5.876774720514415407, 20.10561748372801461 ) ) ;
#11277 = CARTESIAN_POINT ( 'NONE',  ( 19.92038474643397805, 8.973206291307779026, -1.500000000000002220 ) ) ;
#11278 = CARTESIAN_POINT ( 'NONE',  ( 7.136624701378261548, -5.876774720514419847, 20.99078681144753844 ) ) ;
#11279 = ORIENTED_EDGE ( 'NONE', *, *, #27799, .F. ) ;
#11280 = CARTESIAN_POINT ( 'NONE',  ( 25.03920237757594691, 5.025550379011072266, -9.721825256066050969 ) ) ;
#11281 = LINE ( 'NONE', #43246, #73489 ) ;
#11282 = ADVANCED_FACE ( 'NONE', ( #40263 ), #36802, .T. ) ;
#11283 = ADVANCED_FACE ( 'NONE', ( #55492 ), #86432, .T. ) ;
#11284 = VERTEX_POINT ( 'NONE', #25536 ) ;
#11285 = ADVANCED_FACE ( 'NONE', ( #73219 ), #56505, .T. ) ;
#11286 = CARTESIAN_POINT ( 'NONE',  ( -30.63563248976338826, -23.78419283595092537, 10.96997220532171369 ) ) ;
#11287 = ORIENTED_EDGE ( 'NONE', *, *, #35592, .T. ) ;
#11288 = CARTESIAN_POINT ( 'NONE',  ( 7.858420481369514654, 6.475225279485573360, -27.14867965659404092 ) ) ;
#11289 = EDGE_CURVE ( 'NONE', #90864, #65243, #95044, .T. ) ;
#11290 = DIRECTION ( 'NONE',  ( 0.000000000000000000, 1.000000000000000000, 0.000000000000000000 ) ) ;
#11291 = CARTESIAN_POINT ( 'NONE',  ( -12.29646723538143505, -17.35194501319736560, 11.49999999999998934 ) ) ;
#11292 = DIRECTION ( 'NONE',  ( 0.000000000000000000, 0.9999999999976377785, 2.173523156925979975E-06 ) ) ;
#11293 = FACE_OUTER_BOUND ( 'NONE', #34753, .T. ) ;
#11294 = VECTOR ( 'NONE', #27725, 1000.000000000000114 ) ;
#11295 = PLANE ( 'NONE',  #60002 ) ;
#11296 = CARTESIAN_POINT ( 'NONE',  ( -108.6228709571500417, -23.47596703998600631, 11.44779298504227860 ) ) ;
#11297 = CARTESIAN_POINT ( 'NONE',  ( -13.55963120218723361, -13.89248740512243430, 11.49999999999998934 ) ) ;
#11298 = CARTESIAN_POINT ( 'NONE',  ( 14.43441819135929194, -3.316774720514426456, -28.36222020317710957 ) ) ;
#11299 = ORIENTED_EDGE ( 'NONE', *, *, #74509, .T. ) ;
#11300 = CARTESIAN_POINT ( 'NONE',  ( 19.52168601723349894, 1.684101417132040979, 11.49999999999999645 ) ) ;
#11301 = CARTESIAN_POINT ( 'NONE',  ( 31.63524360068765162, -3.637569336689931543, 27.31569296206930630 ) ) ;
#11302 = CIRCLE ( 'NONE', #51793, 21.24999999999998934 ) ;
#11303 = DIRECTION ( 'NONE',  ( 0.000000000000000000, 0.000000000000000000, 1.000000000000000000 ) ) ;
#11304 = ADVANCED_FACE ( 'NONE', ( #48380 ), #75671, .T. ) ;
#11305 = VERTEX_POINT ( 'NONE', #49392 ) ;
#11306 = CARTESIAN_POINT ( 'NONE',  ( 8.160000000000000142, -8.603846352786376883, -0.6978360589526751978 ) ) ;
#11307 = DIRECTION ( 'NONE',  ( 0.000000000000000000, 2.173523156925980399E-06, -0.9999999999976378895 ) ) ;
#11308 = AXIS2_PLACEMENT_3D ( 'NONE', #23610, #47975, #16005 ) ;
#11309 = CARTESIAN_POINT ( 'NONE',  ( 27.53860345374936713, 4.772774720514425972, -5.064153531141387918E-12 ) ) ;
#11310 = DIRECTION ( 'NONE',  ( -3.773278334453080206E-23, 0.9999999999976377785, 2.173523156925979975E-06 ) ) ;
#11312 = EDGE_CURVE ( 'NONE', #62112, #46432, #52036, .T. ) ;
#11311 = CARTESIAN_POINT ( 'NONE',  ( 15.21843288076463629, 12.49332292251147614, -1.500000000000002220 ) ) ;
#11313 = CIRCLE ( 'NONE', #24279, 129.7684398600581517 ) ;
#11314 = VERTEX_POINT ( 'NONE', #65125 ) ;
#11315 = AXIS2_PLACEMENT_3D ( 'NONE', #29543, #15311, #36663 ) ;
#11316 = CARTESIAN_POINT ( 'NONE',  ( -78.52287095715006160, -24.65952944569304606, 1.056160979905698794 ) ) ;
#11317 = DIRECTION ( 'NONE',  ( -3.773278334444167608E-23, 1.000000000000000000, 0.000000000000000000 ) ) ;
#11318 = EDGE_CURVE ( 'NONE', #75985, #64522, #80827, .T. ) ;
#11319 = VECTOR ( 'NONE', #36751, 1000.000000000000114 ) ;
#11320 = APPROVAL_DATE_TIME ( #9304, #85348 ) ;
#11321 = VERTEX_POINT ( 'NONE', #42291 ) ;
#11322 = CARTESIAN_POINT ( 'NONE',  ( -6.660000000000001030, -6.553980293839118509, 7.335060089566987962 ) ) ;
#11323 = CARTESIAN_POINT ( 'NONE',  ( 32.66876533700882845, 5.965225279485572685, -12.58926540598385557 ) ) ;
#11324 = FACE_OUTER_BOUND ( 'NONE', #38483, .T. ) ;
#11325 = CARTESIAN_POINT ( 'NONE',  ( -29.52287095715006515, -23.64153651536914680, 11.05761042422066787 ) ) ;
#11326 = CARTESIAN_POINT ( 'NONE',  ( -78.92430620016367016, -25.33009845126374415, 4.495758016894969344 ) ) ;
#11327 = DIRECTION ( 'NONE',  ( 3.773278334444167608E-23, -1.000000000000000000, 0.000000000000000000 ) ) ;
#11328 = CARTESIAN_POINT ( 'NONE',  ( 2.899999999999999023, 33.29999999999999716, 2.100000000000000089 ) ) ;
#11329 = CARTESIAN_POINT ( 'NONE',  ( -12.66726347749767179, -15.43046242340049545, 11.49999999999998934 ) ) ;
#11330 = DIRECTION ( 'NONE',  ( -0.000000000000000000, 1.000000000000000000, -0.000000000000000000 ) ) ;
#11331 = CARTESIAN_POINT ( 'NONE',  ( 17.57725459251073019, -9.329341740261039462, -1.500000000000002220 ) ) ;
#11332 = ORIENTED_EDGE ( 'NONE', *, *, #1041, .T. ) ;
#11333 = CARTESIAN_POINT ( 'NONE',  ( -122.5228709571500474, -23.95044443724993144, 10.65354141964648882 ) ) ;
#11334 = EDGE_CURVE ( 'NONE', #99120, #10131, #42357, .T. ) ;
#11335 = CARTESIAN_POINT ( 'NONE',  ( -29.52287095715006160, -23.40102634903646717, 11.44779303447556629 ) ) ;
#11336 = FACE_OUTER_BOUND ( 'NONE', #45222, .T. ) ;
#11337 = CARTESIAN_POINT ( 'NONE',  ( 19.92439739378097840, -5.974006126113303949, 11.49999999999999645 ) ) ;
#11338 = MANIFOLD_SOLID_BREP ( 'Kes-Ekstr\X2\00fc\X0\zyon27', #80877 ) ;
#11339 = LINE ( 'NONE', #3739, #59736 ) ;
#11340 = EDGE_CURVE ( 'NONE', #64814, #100208, #7093, .T. ) ;
#11341 = LINE ( 'NONE', #72250, #19814 ) ;
#11342 = CARTESIAN_POINT ( 'NONE',  ( -18.69919181139871966, -13.08804974640095686, 11.49999999999999645 ) ) ;
#11343 = ORIENTED_EDGE ( 'NONE', *, *, #81141, .F. ) ;
#11344 = CARTESIAN_POINT ( 'NONE',  ( -43.52287095715006160, -24.64898659630528854, 1.056161002820819261 ) ) ;
#11345 = FACE_OUTER_BOUND ( 'NONE', #13829, .T. ) ;
#11346 = ORIENTED_EDGE ( 'NONE', *, *, #17394, .F. ) ;
#11347 = CARTESIAN_POINT ( 'NONE',  ( 12.36038202409810438, -16.04522380935875248, -1.500000000000002220 ) ) ;
#11348 = ADVANCED_FACE ( 'NONE', ( #61869 ), #7568, .F. ) ;
#11349 = CARTESIAN_POINT ( 'NONE',  ( 7.072045900997899537, -6.376774720514427841, 21.62824307385093192 ) ) ;
#11350 = CARTESIAN_POINT ( 'NONE',  ( 14.52511747680497933, 5.965225279485572685, -27.86035006098926559 ) ) ;
#11351 = B_SPLINE_CURVE_WITH_KNOTS ( 'NONE', 3,
 ( #33346, #65341, #26744, #87140, #25744, #17629 ),
 .UNSPECIFIED., .F., .F.,
 ( 4, 2, 4 ),
 ( 0.000000000000000000, 0.001380764517854764966, 0.002761529035709529931 ),
 .UNSPECIFIED. ) ;
#11352 = CARTESIAN_POINT ( 'NONE',  ( -100.6228709571500701, -23.85196035786901447, -0.8779234886474918120 ) ) ;
#11353 = B_SPLINE_CURVE_WITH_KNOTS ( 'NONE', 3,
 ( #1093, #93930, #22893, #32036, #53882, #69605 ),
 .UNSPECIFIED., .F., .F.,
 ( 4, 2, 4 ),
 ( 1.570755371634395932E-05, 0.001396183895866091006, 0.002776660238015837747 ),
 .UNSPECIFIED. ) ;
#11354 = ORIENTED_EDGE ( 'NONE', *, *, #32774, .T. ) ;
#11355 = CARTESIAN_POINT ( 'NONE',  ( -79.35175030129791196, -25.28818030286010909, 5.821563397865827660 ) ) ;
#11356 = CARTESIAN_POINT ( 'NONE',  ( -10.36589631659242627, 6.376774720514426065, 27.85486277704324110 ) ) ;
#11357 = CARTESIAN_POINT ( 'NONE',  ( -7.287290609967129740, 18.71191762695291771, -1.500000000000002220 ) ) ;
#11358 = CARTESIAN_POINT ( 'NONE',  ( 11.68726034403320746, 17.49698133428071145, 11.49999999999999645 ) ) ;
#11359 = CARTESIAN_POINT ( 'NONE',  ( 32.16024265030974050, -0.3587747205144265483, 14.03360796525321774 ) ) ;
#11360 = CARTESIAN_POINT ( 'NONE',  ( -93.52287095715006160, -24.35013146730204525, 9.818937971375095941 ) ) ;
#11361 = CARTESIAN_POINT ( 'NONE',  ( 8.687672273659204691, 20.25853876245846408, 11.49999999999998934 ) ) ;
#11362 = AXIS2_PLACEMENT_3D ( 'NONE', #60558, #76734, #62543 ) ;
#11363 = DIRECTION ( 'NONE',  ( -0.1311553622875919756, -6.845827386180409975E-16, -0.9913618264504692190 ) ) ;
#11364 = DIRECTION ( 'NONE',  ( 0.000000000000000000, -1.000000000000000000, 0.000000000000000000 ) ) ;
#11365 = CARTESIAN_POINT ( 'NONE',  ( 0.000000000000000000, 1.826774720514426464, 0.000000000000000000 ) ) ;
#11366 = CARTESIAN_POINT ( 'NONE',  ( -90.70649462243461869, -25.27880950044346164, 5.947789066509452383 ) ) ;
#11367 = CARTESIAN_POINT ( 'NONE',  ( -86.55620429048336462, -24.65952944569304606, 1.056160979905700348 ) ) ;
#11368 = VERTEX_POINT ( 'NONE', #44264 ) ;
#11369 = ORIENTED_EDGE ( 'NONE', *, *, #27890, .T. ) ;
#11370 = CARTESIAN_POINT ( 'NONE',  ( -65.05438548721848235, -3.316774720514426456, 27.45402280011862572 ) ) ;
#11371 = CARTESIAN_POINT ( 'NONE',  ( -4.300916688315937542, -6.376774720514410077, 19.43951662020192828 ) ) ;
#11372 = CARTESIAN_POINT ( 'NONE',  ( -108.6228709571500559, -29.50250786944525672, 11.44777988621622988 ) ) ;
#11373 = CARTESIAN_POINT ( 'NONE',  ( -17.34406541665444124, 10.97931167347951842, -1.500000000000002220 ) ) ;
#11374 = ORIENTED_EDGE ( 'NONE', *, *, #88853, .F. ) ;
#11375 = DIRECTION ( 'NONE',  ( -3.491481338843133355E-15, 1.000000000000000000, -2.352173255807804438E-16 ) ) ;
#11376 = LINE ( 'NONE', #3778, #93663 ) ;
#11377 = DIRECTION ( 'NONE',  ( 0.000000000000000000, 0.000000000000000000, 1.000000000000000000 ) ) ;
#11378 = CARTESIAN_POINT ( 'NONE',  ( 2.183928509170398602, -22.20744181112294413, -1.500000000000002220 ) ) ;
#11379 = CARTESIAN_POINT ( 'NONE',  ( 32.15269211224249091, -4.540774720514427543, 3.401810532325273417 ) ) ;
#11380 = CARTESIAN_POINT ( 'NONE',  ( -124.6228709571500417, -24.65952944569304606, 1.056160979905705011 ) ) ;
#11381 = VERTEX_POINT ( 'NONE', #75194 ) ;
#11382 = CARTESIAN_POINT ( 'NONE',  ( -31.66446019296014569, -24.86181185134534388, 1.747789972853592833 ) ) ;
#11383 = LINE ( 'NONE', #43344, #23127 ) ;
#11384 = VECTOR ( 'NONE', #33447, 1000.000000000000000 ) ;
#11385 = CARTESIAN_POINT ( 'NONE',  ( -20.60679684081203789, -3.318877370925724879, -1.500000000000002220 ) ) ;
#11386 = VERTEX_POINT ( 'NONE', #4701 ) ;
#11388 = ORIENTED_EDGE ( 'NONE', *, *, #7671, .F. ) ;
#11387 = CARTESIAN_POINT ( 'NONE',  ( -39.11412362507491025, -25.24269817073092170, 3.764647656015266186 ) ) ;
#11389 = ORIENTED_EDGE ( 'NONE', *, *, #21138, .F. ) ;
#11390 = AXIS2_PLACEMENT_3D ( 'NONE', #57874, #74569, #81188 ) ;
#11391 = CARTESIAN_POINT ( 'NONE',  ( -33.52287095715006160, -23.47593901973090169, -1.443836447538997314 ) ) ;
#11392 = CARTESIAN_POINT ( 'NONE',  ( -3.607955376466517095, 20.77440192976073519, -1.500000000000002220 ) ) ;
#11393 = ADVANCED_FACE ( 'NONE', ( #35652 ), #90925, .F. ) ;
#11394 = AXIS2_PLACEMENT_3D ( 'NONE', #31829, #63804, #46553 ) ;
#11395 = ORIENTED_EDGE ( 'NONE', *, *, #76437, .F. ) ;
#11396 = LINE ( 'NONE', #58090, #98086 ) ;
#11398 = ADVANCED_FACE ( 'NONE', ( #67605 ), #23276, .T. ) ;
#11397 = CARTESIAN_POINT ( 'NONE',  ( -48.91478977402367434, -25.27868427054752587, 5.813191968676703958 ) ) ;
#11399 = CARTESIAN_POINT ( 'NONE',  ( -120.5534771641331133, -24.63419186844610920, 9.035850630976920428 ) ) ;
#11400 = EDGE_CURVE ( 'NONE', #86526, #21106, #91920, .T. ) ;
#11401 = CARTESIAN_POINT ( 'NONE',  ( -76.58462478488942793, -24.51419770103157347, 9.386484678747176957 ) ) ;
#11402 = CARTESIAN_POINT ( 'NONE',  ( 7.107139210497321002, -6.376774720514413630, 19.78447747620696617 ) ) ;
#11403 = CARTESIAN_POINT ( 'NONE',  ( -11.49108604648090548, 18.38894055434275643, -1.500000000000002220 ) ) ;
#11404 = CARTESIAN_POINT ( 'NONE',  ( -80.48900664166535535, -25.12224392042292820, 7.101635560657246771 ) ) ;
#11406 = VERTEX_POINT ( 'NONE', #12791 ) ;
#11405 = CARTESIAN_POINT ( 'NONE',  ( -13.70410651198969809, -17.55484038775568933, 11.49999999999999645 ) ) ;
#11407 = CARTESIAN_POINT ( 'NONE',  ( -50.41832839342763606, -25.31441722420615648, 5.198500813728550440 ) ) ;
#11408 = CARTESIAN_POINT ( 'NONE',  ( -92.55620429048336462, -23.47596703998600631, 11.44779298504227683 ) ) ;
#11409 = LINE ( 'NONE', #2812, #24576 ) ;
#11410 = ORIENTED_EDGE ( 'NONE', *, *, #21702, .T. ) ;
#11411 = EDGE_CURVE ( 'NONE', #98033, #84710, #100390, .T. ) ;
#11412 = EDGE_CURVE ( 'NONE', #8902, #65922, #77564, .T. ) ;
#11414 = ORIENTED_EDGE ( 'NONE', *, *, #19882, .T. ) ;
#11413 = DIRECTION ( 'NONE',  ( 1.226388327005079762E-16, 0.000000000000000000, -1.000000000000000000 ) ) ;
#11415 = ORIENTED_EDGE ( 'NONE', *, *, #38917, .F. ) ;
#11416 = DIRECTION ( 'NONE',  ( 0.000000000000000000, -1.000000000000000000, 0.000000000000000000 ) ) ;
#11417 = CARTESIAN_POINT ( 'NONE',  ( -88.62287095715004170, -23.72773821059535848, 11.05748984161097503 ) ) ;
#11418 = CARTESIAN_POINT ( 'NONE',  ( -35.52287095715009713, -24.14321612903113845, -0.2833117244521470290 ) ) ;
#11419 = CARTESIAN_POINT ( 'NONE',  ( 29.73860345376319358, -5.356514366711551567, 19.42370913944100863 ) ) ;
#11420 = ORIENTED_EDGE ( 'NONE', *, *, #21846, .T. ) ;
#11421 = CARTESIAN_POINT ( 'NONE',  ( -130.5728709571500872, -24.82780549326299280, 8.726980033514458057 ) ) ;
#11422 = CARTESIAN_POINT ( 'NONE',  ( 21.16529133594374557, -7.503415950508986576, -1.500000000000002220 ) ) ;
#11423 = ORIENTED_EDGE ( 'NONE', *, *, #94242, .F. ) ;
#11424 = CARTESIAN_POINT ( 'NONE',  ( -98.89667099290487329, -25.25590005895643486, 6.210304623333523288 ) ) ;
#11425 = CARTESIAN_POINT ( 'NONE',  ( -101.5124320122265260, -24.35071581493543746, 9.817618358456027039 ) ) ;
#11426 = CARTESIAN_POINT ( 'NONE',  ( 2.598318274922708060, -5.876774720514414518, 19.68966562063331693 ) ) ;
#11427 = DIRECTION ( 'NONE',  ( 0.000000000000000000, -1.000000000000000000, 0.000000000000000000 ) ) ;
#11428 = CARTESIAN_POINT ( 'NONE',  ( -63.90635909705261497, -25.30558673197061026, 5.002395802403323266 ) ) ;
#11429 = CARTESIAN_POINT ( 'NONE',  ( -3.586273028688536257, -19.27814873881845514, 11.49999999999998934 ) ) ;
#11430 = CARTESIAN_POINT ( 'NONE',  ( -65.05438548721848235, 5.356774720514425603, 27.45402280011862572 ) ) ;
#11431 = VERTEX_POINT ( 'NONE', #81820 ) ;
#11432 = CARTESIAN_POINT ( 'NONE',  ( 7.253797376210795456, 20.28272692992397808, -1.500000000000002220 ) ) ;
#11433 = CARTESIAN_POINT ( 'NONE',  ( -128.5895405319625695, -24.51314013834317862, 0.6176544820404316072 ) ) ;
#11434 = CARTESIAN_POINT ( 'NONE',  ( -114.5228709571500900, -24.33832256527049864, 0.1851278514138636755 ) ) ;
#11435 = CARTESIAN_POINT ( 'NONE',  ( -101.0641960954074534, -25.14446816578130850, 2.968297954937114458 ) ) ;
#11436 = AXIS2_PLACEMENT_3D ( 'NONE', #87900, #78759, #85005 ) ;
#11437 = CARTESIAN_POINT ( 'NONE',  ( -77.62287095715002749, -24.51387760970723662, 9.387446482453407626 ) ) ;
#11438 = CARTESIAN_POINT ( 'NONE',  ( -3.094460115123966570, -22.75893099265358188, -1.500000000000002220 ) ) ;
#11439 = PERSON_AND_ORGANIZATION ( #70597, #27821 ) ;
#11440 = CARTESIAN_POINT ( 'NONE',  ( -6.499999999999992895, 2.239999999999997105, 2.100000000000000977 ) ) ;
#11441 = CARTESIAN_POINT ( 'NONE',  ( -53.49130680602832655, -24.51314013834315730, 0.6176544820404108460 ) ) ;
#11442 = CARTESIAN_POINT ( 'NONE',  ( 18.99975792849237877, 6.539580213093530325, 11.49999999999999645 ) ) ;
#11443 = DIRECTION ( 'NONE',  ( 0.000000000000000000, 0.000000000000000000, 1.000000000000000000 ) ) ;
#11444 = CARTESIAN_POINT ( 'NONE',  ( -32.53164638043851653, -24.51419770103159834, 9.386484678747182286 ) ) ;
#11445 = PLANE ( 'NONE',  #19811 ) ;
#11446 = FACE_OUTER_BOUND ( 'NONE', #9413, .T. ) ;
#11447 = LINE ( 'NONE', #19055, #20265 ) ;
#11448 = CARTESIAN_POINT ( 'NONE',  ( -2.735935421901279696, -19.66989661884619522, -1.500000000000002220 ) ) ;
#11449 = FACE_OUTER_BOUND ( 'NONE', #87517, .T. ) ;
#11450 = CARTESIAN_POINT ( 'NONE',  ( 19.16472379399037251, -4.548241762842377689, -1.500000000000002220 ) ) ;
#11451 = EDGE_CURVE ( 'NONE', #55557, #77754, #97981, .T. ) ;
#11452 = CARTESIAN_POINT ( 'NONE',  ( -42.61653805103011905, -23.48783264082477373, -1.443836473390076147 ) ) ;
#11453 = VECTOR ( 'NONE', #16909, 1000.000000000000000 ) ;
#11454 = APPROVAL_STATUS ( 'not_yet_approved' ) ;
#11456 = UNCERTAINTY_MEASURE_WITH_UNIT (LENGTH_MEASURE( 1.000000000000000082E-05 ), #10639, 'distance_accuracy_value', 'NONE');
#11455 =( GEOMETRIC_REPRESENTATION_CONTEXT ( 3 ) GLOBAL_UNCERTAINTY_ASSIGNED_CONTEXT ( ( #11456 ) ) GLOBAL_UNIT_ASSIGNED_CONTEXT ( ( #10639, #9637, #41601 ) ) REPRESENTATION_CONTEXT ( 'NONE', 'WORKASPACE' ) );
#11457 = DIRECTION ( 'NONE',  ( 1.000000000000000000, 0.000000000000000000, 0.000000000000000000 ) ) ;
#11458 = CYLINDRICAL_SURFACE ( 'NONE', #47499, 24.00000000000000000 ) ;
#11459 = CARTESIAN_POINT ( 'NONE',  ( 18.80685554986811070, -8.408966509905500430, 11.49999999999999645 ) ) ;
#11460 = EDGE_CURVE ( 'NONE', #22752, #21356, #43419, .T. ) ;
#11461 = CARTESIAN_POINT ( 'NONE',  ( -42.62287095715007013, -23.73907113216990084, -1.053371485793237250 ) ) ;
#11462 = CARTESIAN_POINT ( 'NONE',  ( 8.854694546379761277, 20.84150027139232364, 11.49999999999999645 ) ) ;
#11463 = VERTEX_POINT ( 'NONE', #28036 ) ;
#11464 = EDGE_CURVE ( 'NONE', #69290, #97480, #61560, .T. ) ;
#11465 = CARTESIAN_POINT ( 'NONE',  ( -99.62287095715005592, -29.50248528299804818, 1.056150453629042030 ) ) ;
#11466 = CARTESIAN_POINT ( 'NONE',  ( -50.80821443252320080, -25.31060262516012926, 4.652599235852771464 ) ) ;
#11467 = CARTESIAN_POINT ( 'NONE',  ( -26.35953173686715800, -24.61459992720930501, 7.694642789483244094 ) ) ;
#11468 = FACE_OUTER_BOUND ( 'NONE', #22052, .T. ) ;
#11469 = EDGE_LOOP ( 'NONE', ( #90461, #89530, #100281, #57501 ) ) ;
#11470 = ORIENTED_EDGE ( 'NONE', *, *, #9377, .T. ) ;
#11471 = CARTESIAN_POINT ( 'NONE',  ( -99.77787996869076892, -25.14990886459445107, 6.942063247122693070 ) ) ;
#11472 = CARTESIAN_POINT ( 'NONE',  ( -21.29394331855728240, -8.360804490491451801, -1.500000000000002220 ) ) ;
#11473 = CARTESIAN_POINT ( 'NONE',  ( -110.4715243189340299, -25.18566208650414140, 3.299076066840834098 ) ) ;
#11474 = CARTESIAN_POINT ( 'NONE',  ( -25.92875734969026169, 3.316774720514426456, 26.43402280011862615 ) ) ;
#11475 = CARTESIAN_POINT ( 'NONE',  ( -76.62287095715007013, -23.48786465467241058, 11.44779295918254469 ) ) ;
#11476 = CARTESIAN_POINT ( 'NONE',  ( -15.53634343318938704, 16.32316209468629253, 11.49999999999999645 ) ) ;
#11477 = ORIENTED_EDGE ( 'NONE', *, *, #78539, .F. ) ;
#11478 = CARTESIAN_POINT ( 'NONE',  ( -89.81226385320383088, -25.13785473458314712, 7.104038777044550557 ) ) ;
#11479 = CARTESIAN_POINT ( 'NONE',  ( -18.59763704738199408, -11.70098744416181979, 11.49999999999998934 ) ) ;
#11480 = DIRECTION ( 'NONE',  ( 0.000000000000000000, 0.000000000000000000, -1.000000000000000000 ) ) ;
#11481 = CARTESIAN_POINT ( 'NONE',  ( -29.17238308422418669, -24.79699977470989936, 6.041340515266470312 ) ) ;
#11482 = ORIENTED_EDGE ( 'NONE', *, *, #29490, .F. ) ;
#11483 = DIRECTION ( 'NONE',  ( -3.773278334453079030E-23, 0.9999999999976377785, 2.173523156925979128E-06 ) ) ;
#11484 = LINE ( 'NONE', #49068, #90002 ) ;
#11485 = ORIENTED_EDGE ( 'NONE', *, *, #32476, .T. ) ;
#11486 = CARTESIAN_POINT ( 'NONE',  ( -9.278253834636473130, -5.876774720514426953, 18.21871304725684482 ) ) ;
#11487 = CARTESIAN_POINT ( 'NONE',  ( 20.06376955418885899, 4.186446014007643157, 11.49999999999998934 ) ) ;
#11488 = ORIENTED_EDGE ( 'NONE', *, *, #95820, .F. ) ;
#11489 = ORIENTED_EDGE ( 'NONE', *, *, #70993, .F. ) ;
#11490 = ORIENTED_EDGE ( 'NONE', *, *, #97076, .F. ) ;
#11491 = PLANE ( 'NONE',  #98782 ) ;
#11492 = CARTESIAN_POINT ( 'NONE',  ( -3.594920434497504758, 22.80983129501555950, -1.500000000000002220 ) ) ;
#11493 = CARTESIAN_POINT ( 'NONE',  ( -64.22287095715006444, -23.47596703998600631, 11.44779298504227683 ) ) ;
#11494 = CARTESIAN_POINT ( 'NONE',  ( -8.236308187080631171, 18.58821751820538637, -1.500000000000002220 ) ) ;
#11495 = ORIENTED_EDGE ( 'NONE', *, *, #31472, .T. ) ;
#11496 = DIRECTION ( 'NONE',  ( -0.000000000000000000, 1.000000000000000000, -0.000000000000000000 ) ) ;
#11497 = CARTESIAN_POINT ( 'NONE',  ( -29.57134449316367864, -23.40477069770800966, 11.44779303447556806 ) ) ;
#11498 = EDGE_CURVE ( 'NONE', #8268, #65583, #44670, .T. ) ;
#11499 = CARTESIAN_POINT ( 'NONE',  ( -105.5884215510445046, -24.63355581998386157, 0.9682620441943899925 ) ) ;
#11500 = CARTESIAN_POINT ( 'NONE',  ( -70.40598983096596442, -25.03149849373329872, 7.561209383477862644 ) ) ;
#11501 = ORIENTED_EDGE ( 'NONE', *, *, #36459, .T. ) ;
#11502 = CARTESIAN_POINT ( 'NONE',  ( -112.6228709571500701, -23.48786465467241769, 11.44779295918254114 ) ) ;
#11503 = CARTESIAN_POINT ( 'NONE',  ( -86.55620429048337883, -23.48786465467241058, 11.44779295918254292 ) ) ;
#11504 = ORIENTED_EDGE ( 'NONE', *, *, #40878, .F. ) ;
#11505 = CARTESIAN_POINT ( 'NONE',  ( -13.51810693421681719, -15.76408947421354156, -1.500000000000002220 ) ) ;
#11506 = AXIS2_PLACEMENT_3D ( 'NONE', #46493, #24146, #92651 ) ;
#11507 = ORIENTED_EDGE ( 'NONE', *, *, #18065, .T. ) ;
#11509 = EDGE_LOOP ( 'NONE', ( #66343, #55027, #6189, #94328 ) ) ;
#11508 = DIRECTION ( 'NONE',  ( -0.000000000000000000, 1.000000000000000000, -0.000000000000000000 ) ) ;
#11510 = CARTESIAN_POINT ( 'NONE',  ( -41.61685852264373864, -23.48786465467240347, 11.44779295918255180 ) ) ;
#11511 = CARTESIAN_POINT ( 'NONE',  ( 8.971512145086531831, -9.528487854913505473, -6.499999999999998224 ) ) ;
#11512 = ORIENTED_EDGE ( 'NONE', *, *, #100, .T. ) ;
#11513 = ORIENTED_EDGE ( 'NONE', *, *, #60898, .F. ) ;
#11514 = DIRECTION ( 'NONE',  ( 0.000000000000000000, 0.000000000000000000, 1.000000000000000000 ) ) ;
#11515 = ADVANCED_FACE ( 'NONE', ( #78061 ), #87193, .T. ) ;
#11516 = DIRECTION ( 'NONE',  ( -0.000000000000000000, 1.000000000000000000, -0.000000000000000000 ) ) ;
#11517 = CARTESIAN_POINT ( 'NONE',  ( -43.56067035728424486, -23.73791477778911130, 11.05961554403171121 ) ) ;
#11519 = ORIENTED_EDGE ( 'NONE', *, *, #16702, .F. ) ;
#11518 = CARTESIAN_POINT ( 'NONE',  ( -4.445301477617020325, 21.63612927058290936, 11.49999999999999645 ) ) ;
#11520 = CARTESIAN_POINT ( 'NONE',  ( -103.5929782930063681, -23.96119346886881019, -0.6495511937832079141 ) ) ;
#11521 = ADVANCED_FACE ( 'NONE', ( #69967 ), #18182, .T. ) ;
#11522 = CARTESIAN_POINT ( 'NONE',  ( -20.05226876979747530, -10.47825485868949613, 11.49999999999998934 ) ) ;
#11523 = EDGE_CURVE ( 'NONE', #5853, #21581, #95308, .T. ) ;
#11525 = ORIENTED_EDGE ( 'NONE', *, *, #70001, .F. ) ;
#11524 = DIRECTION ( 'NONE',  ( -3.773278334453079030E-23, 0.9999999999976377785, 2.173523156925979128E-06 ) ) ;
#11526 = CIRCLE ( 'NONE', #40715, 28.96799999999999642 ) ;
#11527 = EDGE_CURVE ( 'NONE', #9990, #91541, #63384, .T. ) ;
#11528 = ORIENTED_EDGE ( 'NONE', *, *, #2203, .F. ) ;
#11529 = AXIS2_PLACEMENT_3D ( 'NONE', #50624, #65876, #25785 ) ;
#11530 = ADVANCED_FACE ( 'NONE', ( #1972 ), #93292, .T. ) ;
#11531 = CARTESIAN_POINT ( 'NONE',  ( -1.358974358974357921, -6.376774720514420736, 20.75510817307693046 ) ) ;
#11532 = CARTESIAN_POINT ( 'NONE',  ( 32.40199294184733247, 6.475225279485576024, -12.82361242714783245 ) ) ;
#11533 = ORIENTED_EDGE ( 'NONE', *, *, #50356, .F. ) ;
#11534 = CARTESIAN_POINT ( 'NONE',  ( -9.521469661382619520, 18.92286876745961166, -1.500000000000002220 ) ) ;
#11535 = CARTESIAN_POINT ( 'NONE',  ( -7.312991930324885814, -6.376774720514413630, 20.02088365235844947 ) ) ;
#11536 = CARTESIAN_POINT ( 'NONE',  ( -39.55620429048340014, -23.47593901973091235, -1.443836447539011525 ) ) ;
#11537 = CARTESIAN_POINT ( 'NONE',  ( 22.08996893241407378, 3.065900275835479860, -1.500000000000002220 ) ) ;
#11538 = CARTESIAN_POINT ( 'NONE',  ( 3.176458874063931681, 0.3587747205143967943, -28.85257003503889806 ) ) ;
#11539 = EDGE_CURVE ( 'NONE', #56847, #77894, #70979, .T. ) ;
#11540 = VERTEX_POINT ( 'NONE', #47144 ) ;
#11541 = CARTESIAN_POINT ( 'NONE',  ( -5.576923076923076650, -6.376774720514418959, 20.44941907051282470 ) ) ;
#11542 = DIRECTION ( 'NONE',  ( 0.000000000000000000, 0.000000000000000000, -1.000000000000000000 ) ) ;
#11543 = CARTESIAN_POINT ( 'NONE',  ( -36.60104952365126962, -23.96169478059712432, 10.65365249895718591 ) ) ;
#11544 = CARTESIAN_POINT ( 'NONE',  ( 29.73860345376319358, 1.477225279485574028, 7.190646357373898680E-15 ) ) ;
#11545 = CARTESIAN_POINT ( 'NONE',  ( 5.544562197198338538, -18.70016399976332977, -1.500000000000002220 ) ) ;
#11546 = CARTESIAN_POINT ( 'NONE',  ( 14.05358622956002357, 16.19628355576825385, -1.500000000000002220 ) ) ;
#11547 = CARTESIAN_POINT ( 'NONE',  ( -1.064504969004270052, -6.376774720514410077, 19.35667676486395905 ) ) ;
#11548 = DIRECTION ( 'NONE',  ( 0.000000000000000000, 0.000000000000000000, 1.000000000000000000 ) ) ;
#11549 = FACE_OUTER_BOUND ( 'NONE', #22566, .T. ) ;
#11550 = CARTESIAN_POINT ( 'NONE',  ( -22.17926634000774655, 4.976981427743210951, -1.500000000000002220 ) ) ;
#11551 = DIRECTION ( 'NONE',  ( 0.000000000000000000, 0.000000000000000000, 1.000000000000000000 ) ) ;
#11552 = CARTESIAN_POINT ( 'NONE',  ( -98.54805141098935906, -24.51314013834315020, 0.6176544820404104019 ) ) ;
#11553 = DIRECTION ( 'NONE',  ( 0.000000000000000000, -0.3081562241202470687, -0.9513357669802772199 ) ) ;
#11554 = CARTESIAN_POINT ( 'NONE',  ( 5.901097582950029619, 19.04237314665466485, 11.49999999999999645 ) ) ;
#11555 = DIRECTION ( 'NONE',  ( -0.000000000000000000, 2.173523156925979552E-06, -0.9999999999976378895 ) ) ;
#11556 = CARTESIAN_POINT ( 'NONE',  ( 3.421177667410916001, -5.965225279485572685, 28.69411518427638441 ) ) ;
#11557 = DIRECTION ( 'NONE',  ( 3.773278334444166432E-23, -1.000000000000000000, 0.000000000000000000 ) ) ;
#11558 = ORIENTED_EDGE ( 'NONE', *, *, #73559, .F. ) ;
#11559 = CARTESIAN_POINT ( 'NONE',  ( 0.1645010273463760886, 1.417169167140627462, -0.3687607960183705846 ) ) ;
#11560 = ADVANCED_FACE ( 'NONE', ( #54759 ), #16677, .F. ) ;
#11561 = CARTESIAN_POINT ( 'NONE',  ( -33.00279783456706895, -25.16370864782812689, 7.203858152271859439 ) ) ;
#11562 = CARTESIAN_POINT ( 'NONE',  ( 19.61570337458852364, 9.273991169892711994, 11.49999999999998934 ) ) ;
#11563 = CARTESIAN_POINT ( 'NONE',  ( -56.56717682641941991, -23.48786465467241058, 11.44779295918254647 ) ) ;
#11564 = CARTESIAN_POINT ( 'NONE',  ( -17.64752530894654470, 8.349842952099315596, -1.500000000000002220 ) ) ;
#11565 = DIRECTION ( 'NONE',  ( 0.000000000000000000, 0.000000000000000000, 1.000000000000000000 ) ) ;
#11566 = ADVANCED_FACE ( 'NONE', ( #23787 ), #55764, .F. ) ;
#11567 = COORDINATED_UNIVERSAL_TIME_OFFSET ( 0, 0, .AHEAD. ) ;
#11568 = CARTESIAN_POINT ( 'NONE',  ( -60.62287095715004881, -25.00182538069145011, 7.747789668545098429 ) ) ;
#11569 = CARTESIAN_POINT ( 'NONE',  ( -20.44062828730913139, -1.133067592104922694, 11.49999999999999645 ) ) ;
#11570 = CARTESIAN_POINT ( 'NONE',  ( 16.04662828278931741, 3.608091531752042780, -27.86986495919489215 ) ) ;
#11571 = CIRCLE ( 'NONE', #24529, 1.500000000000001332 ) ;
#11572 = EDGE_CURVE ( 'NONE', #77700, #69513, #5643, .T. ) ;
#11573 = CARTESIAN_POINT ( 'NONE',  ( -39.62287095715005592, -23.72773821059535493, 11.05748984161097503 ) ) ;
#11574 = B_SPLINE_CURVE_WITH_KNOTS ( 'NONE', 3,
 ( #2841, #49513, #4332, #80447 ),
 .UNSPECIFIED., .F., .F.,
 ( 4, 4 ),
 ( 0.000000000000000000, 9.999999999998897304E-05 ),
 .UNSPECIFIED. ) ;
#11575 = ORIENTED_EDGE ( 'NONE', *, *, #32926, .T. ) ;
#11576 = EDGE_CURVE ( 'NONE', #65436, #31334, #41079, .T. ) ;
#11577 = DIRECTION ( 'NONE',  ( -1.000000000000000000, -0.000000000000000000, -0.000000000000000000 ) ) ;
#11578 = FACE_OUTER_BOUND ( 'NONE', #61923, .T. ) ;
#11579 = CARTESIAN_POINT ( 'NONE',  ( -4.926336369345162502, -0.3587747205143967943, -28.61095484066305161 ) ) ;
#11580 = CARTESIAN_POINT ( 'NONE',  ( -49.28110964179429487, -25.25138858776646700, 6.053971624764486137 ) ) ;
#11581 = CARTESIAN_POINT ( 'NONE',  ( -109.6292162128046499, -23.96119346886880663, -0.6495511937832053606 ) ) ;
#11582 = VERTEX_POINT ( 'NONE', #86691 ) ;
#11583 = CARTESIAN_POINT ( 'NONE',  ( -81.62287095715005592, -23.48783264082478794, -1.443836473390065711 ) ) ;
#11584 = AXIS2_PLACEMENT_3D ( 'NONE', #21294, #82206, #42672 ) ;
#11585 = CARTESIAN_POINT ( 'NONE',  ( 22.09143763772896918, 6.410036269187016522, 11.49999999999999645 ) ) ;
#11586 = CARTESIAN_POINT ( 'NONE',  ( -7.854035805165779927, 21.33931789143995417, -1.500000000000002220 ) ) ;
#11587 = CARTESIAN_POINT ( 'NONE',  ( -110.5132562145541470, -24.63419186844610920, 9.035850630976920428 ) ) ;
#11588 = DIRECTION ( 'NONE',  ( -3.773278334453079030E-23, 0.9999999999976377785, 2.173523156925979128E-06 ) ) ;
#11589 = CARTESIAN_POINT ( 'NONE',  ( -90.52212989865935810, -23.48783264082477018, -1.443836473390091690 ) ) ;
#11590 = LOCAL_TIME ( 0, 54, 15.00000000000000000, #68346 ) ;
#11591 = CARTESIAN_POINT ( 'NONE',  ( -53.52287095715008292, -23.47593901973090169, -1.443836447538997092 ) ) ;
#11592 = CARTESIAN_POINT ( 'NONE',  ( -89.52287095715006160, -24.65952944569304606, 1.056160979905700570 ) ) ;
#11593 = CARTESIAN_POINT ( 'NONE',  ( -21.85961425739535358, 0.8689724601130633941, 11.49999999999998934 ) ) ;
#11594 = CC_DESIGN_DATE_AND_TIME_ASSIGNMENT ( #48893, #56009, ( #29568 ) ) ;
#11595 = CARTESIAN_POINT ( 'NONE',  ( -77.52287095715006160, -29.50250243563736774, 8.947779886222141599 ) ) ;
#11596 = CARTESIAN_POINT ( 'NONE',  ( -7.999999999999996447, -5.876774720514426953, 17.50000000000000000 ) ) ;
#11597 = LINE ( 'NONE', #27828, #48496 ) ;
#11598 = DIRECTION ( 'NONE',  ( -0.7071067811865436870, 0.7071067811865514585, 0.000000000000000000 ) ) ;
#11599 = EDGE_LOOP ( 'NONE', ( #11135, #5137, #23571, #45095 ) ) ;
#11600 = CARTESIAN_POINT ( 'NONE',  ( -4.163110563111144913, -19.98234244090558320, 11.49999999999998934 ) ) ;
#11601 = VERTEX_POINT ( 'NONE', #2467 ) ;
#11602 = ORIENTED_EDGE ( 'NONE', *, *, #70748, .T. ) ;
#11603 = ORIENTED_EDGE ( 'NONE', *, *, #46001, .T. ) ;
#11604 = ORIENTED_EDGE ( 'NONE', *, *, #55396, .T. ) ;
#11605 = CARTESIAN_POINT ( 'NONE',  ( 20.85440106035463970, 9.703512019146668166, 11.49999999999998934 ) ) ;
#11606 = LINE ( 'NONE', #57316, #72966 ) ;
#11607 = CARTESIAN_POINT ( 'NONE',  ( 1.109688723463823301, -20.12803150795971874, -1.500000000000002220 ) ) ;
#11608 = VERTEX_POINT ( 'NONE', #79072 ) ;
#11609 = PLANE ( 'NONE',  #49387 ) ;
#11610 = CYLINDRICAL_SURFACE ( 'NONE', #64450, 4.300000000000000711 ) ;
#11611 = CARTESIAN_POINT ( 'NONE',  ( -95.50802337316835633, -24.52300882791530512, 0.6510814631126408125 ) ) ;
#11612 = CARTESIAN_POINT ( 'NONE',  ( -123.5228709571500474, -23.47593901973090524, -1.443836447538996204 ) ) ;
#11614 = ORIENTED_EDGE ( 'NONE', *, *, #45777, .T. ) ;
#11613 = CARTESIAN_POINT ( 'NONE',  ( -1.242826169824672977, 21.35102975155811222, 11.49999999999999645 ) ) ;
#11615 = CARTESIAN_POINT ( 'NONE',  ( 6.697025426467099862, -5.876774720514423400, 21.43052570396496037 ) ) ;
#11616 = ORIENTED_EDGE ( 'NONE', *, *, #87582, .F. ) ;
#11617 = CARTESIAN_POINT ( 'NONE',  ( -12.31279356157217109, -18.55646752483835016, 11.49999999999998934 ) ) ;
#11618 = B_SPLINE_CURVE_WITH_KNOTS ( 'NONE', 3,
 ( #80377, #65678, #57059, #41318 ),
 .UNSPECIFIED., .F., .F.,
 ( 4, 4 ),
 ( 0.000000000000000000, 9.999999999998206125E-05 ),
 .UNSPECIFIED. ) ;
#11619 = CARTESIAN_POINT ( 'NONE',  ( -20.66316395829706209, -0.6310838753663271516, -1.500000000000002220 ) ) ;
#11620 = EDGE_LOOP ( 'NONE', ( #22443, #94601, #60277, #25483 ) ) ;
#11621 = AXIS2_PLACEMENT_3D ( 'NONE', #5039, #44604, #45607 ) ;
#11622 = CARTESIAN_POINT ( 'NONE',  ( 3.296033061219842519, -5.876774720514407413, 18.71226942120119574 ) ) ;
#11623 = ORIENTED_EDGE ( 'NONE', *, *, #3167, .F. ) ;
#11624 = DIRECTION ( 'NONE',  ( 0.000000000000000000, 0.000000000000000000, -1.000000000000000000 ) ) ;
#11625 = ORIENTED_EDGE ( 'NONE', *, *, #50802, .F. ) ;
#11626 = CARTESIAN_POINT ( 'NONE',  ( -50.04601614386864838, -25.10935134884508813, 2.868514420169689494 ) ) ;
#11627 = CARTESIAN_POINT ( 'NONE',  ( 17.97375762979478253, -10.76934015532128797, -1.500000000000002220 ) ) ;
#11628 = EDGE_CURVE ( 'NONE', #49235, #88649, #10566, .T. ) ;
#11629 = CARTESIAN_POINT ( 'NONE',  ( 3.414333255021221092, 21.62243999391013105, 11.49999999999999645 ) ) ;
#11630 = CARTESIAN_POINT ( 'NONE',  ( -73.54183095359555011, -24.51419770103157347, 9.386484678747175181 ) ) ;
#11631 = CARTESIAN_POINT ( 'NONE',  ( -11.58057713800463162, -19.31455136971746001, 11.49999999999998934 ) ) ;
#11632 = CARTESIAN_POINT ( 'NONE',  ( -3.961239394588834895, 20.55660451852329018, 11.49999999999998934 ) ) ;
#11633 = CARTESIAN_POINT ( 'NONE',  ( -90.52287095715006160, -29.50248528299804818, 1.056150453629040253 ) ) ;
#11634 = CARTESIAN_POINT ( 'NONE',  ( -80.52287095715006160, -24.99132157543083821, 2.256160258750667502 ) ) ;
#11635 = CARTESIAN_POINT ( 'NONE',  ( -29.62287095715006657, -24.27350855396620943, 9.819127054472291505 ) ) ;
#11636 = DIRECTION ( 'NONE',  ( -1.000000000000000000, 0.000000000000000000, 0.000000000000000000 ) ) ;
#11637 = VERTEX_POINT ( 'NONE', #49157 ) ;
#11638 = EDGE_CURVE ( 'NONE', #82392, #82023, #13192, .T. ) ;
#11639 = ORIENTED_EDGE ( 'NONE', *, *, #47190, .T. ) ;
#11640 = ORIENTED_EDGE ( 'NONE', *, *, #53566, .T. ) ;
#11641 = VECTOR ( 'NONE', #25430, 1000.000000000000000 ) ;
#11642 = ADVANCED_FACE ( 'NONE', ( #62365 ), #50142, .F. ) ;
#11643 = LINE ( 'NONE', #88283, #67644 ) ;
#11644 = ORIENTED_EDGE ( 'NONE', *, *, #56543, .T. ) ;
#11645 = CARTESIAN_POINT ( 'NONE',  ( 21.22668844964908885, 3.412186807495566132, -1.500000000000002220 ) ) ;
#11646 = DIRECTION ( 'NONE',  ( 3.773278334444166432E-23, -1.000000000000000000, 0.000000000000000000 ) ) ;
#11647 = CARTESIAN_POINT ( 'NONE',  ( 20.99878002148846790, -2.064974809011826729, 11.49999999999998934 ) ) ;
#11648 = DIRECTION ( 'NONE',  ( -0.000000000000000000, -1.000000000000000000, -0.000000000000000000 ) ) ;
#11649 = CARTESIAN_POINT ( 'NONE',  ( 2.933277810221831761, -6.376774720514424288, 21.39432064584807947 ) ) ;
#11650 = DIRECTION ( 'NONE',  ( 0.000000000000000000, 0.000000000000000000, 1.000000000000000000 ) ) ;
#11651 = FACE_OUTER_BOUND ( 'NONE', #4029, .T. ) ;
#11652 = CARTESIAN_POINT ( 'NONE',  ( -51.52287095715006870, -23.48786465467241058, 11.44779295918255002 ) ) ;
#11653 = CARTESIAN_POINT ( 'NONE',  ( -9.261969182712835646, 20.05037652441878038, -1.500000000000002220 ) ) ;
#11654 = ORIENTED_EDGE ( 'NONE', *, *, #31225, .F. ) ;
#11655 = CARTESIAN_POINT ( 'NONE',  ( -116.6272965939264594, -23.96119346886881729, -0.6495511937831833782 ) ) ;
#11656 = EDGE_CURVE ( 'NONE', #32849, #67333, #89694, .T. ) ;
#11657 = DIRECTION ( 'NONE',  ( 0.000000000000000000, 0.9999999999976377785, 2.173523156925979975E-06 ) ) ;
#11658 = CARTESIAN_POINT ( 'NONE',  ( -41.64605464260454681, -25.27955944056996884, 4.957686485891340311 ) ) ;
#11659 = FACE_OUTER_BOUND ( 'NONE', #94636, .T. ) ;
#11660 = CIRCLE ( 'NONE', #40860, 3.549999999999999378 ) ;
#11661 = PRODUCT_DEFINITION_FORMATION_WITH_SPECIFIED_SOURCE ( 'ANY', '', #71682, .NOT_KNOWN. ) ;
#11662 = FACE_OUTER_BOUND ( 'NONE', #66953, .T. ) ;
#11663 = CARTESIAN_POINT ( 'NONE',  ( -9.778911232092227124, -18.99720643767551209, -1.500000000000002220 ) ) ;
#11664 = CARTESIAN_POINT ( 'NONE',  ( -69.27983724839798185, -25.13218956900901446, 7.108035130480557129 ) ) ;
#11665 = CARTESIAN_POINT ( 'NONE',  ( -66.62287095715009855, -24.50216790748205753, 0.6166512839542495072 ) ) ;
#11666 = CARTESIAN_POINT ( 'NONE',  ( -64.63656984362181390, -24.15620529776628445, 10.23563542870660115 ) ) ;
#11667 = LINE ( 'NONE', #97410, #24852 ) ;
#11668 = CARTESIAN_POINT ( 'NONE',  ( -3.649967738973055376, -22.27025559232234642, -1.500000000000002220 ) ) ;
#11669 = CARTESIAN_POINT ( 'NONE',  ( -65.55620429048339304, -24.99156044556201905, 7.747789690856173195 ) ) ;
#11670 = VERTEX_POINT ( 'NONE', #26795 ) ;
#11671 = CARTESIAN_POINT ( 'NONE',  ( 4.518955212990007908, -5.876774720514422512, 20.94857968174986951 ) ) ;
#11672 = CARTESIAN_POINT ( 'NONE',  ( -18.76583335001664565, 6.068782795689376286, 11.49999999999999645 ) ) ;
#11673 = CARTESIAN_POINT ( 'NONE',  ( -59.62287095715004881, -23.48783264082478794, -1.443836473390069042 ) ) ;
#11674 = CARTESIAN_POINT ( 'NONE',  ( -32.07722060962682775, -24.86441978397624553, 8.247789967200544581 ) ) ;
#11675 = ADVANCED_FACE ( 'NONE', ( #20666 ), #42039, .T. ) ;
#11676 = VERTEX_POINT ( 'NONE', #72983 ) ;
#11677 = LINE ( 'NONE', #3098, #49052 ) ;
#11678 = CARTESIAN_POINT ( 'NONE',  ( -29.74701180552300883, -25.26026767148650265, 3.841291294183602378 ) ) ;
#11679 = LINE ( 'NONE', #42662, #15632 ) ;
#11680 = CARTESIAN_POINT ( 'NONE',  ( -16.54959454218438708, 13.92943311328891554, 11.49999999999998934 ) ) ;
#11681 = CARTESIAN_POINT ( 'NONE',  ( -20.77875734969026311, 6.143225279485574397, 29.49402280011862487 ) ) ;
#11682 = CARTESIAN_POINT ( 'NONE',  ( -1.480291460309441920, -19.30061035156251847, -1.500000000000002220 ) ) ;
#11683 = CARTESIAN_POINT ( 'NONE',  ( 1.305682803664691249, -5.965225279485572685, 29.57950906855421991 ) ) ;
#11684 = CARTESIAN_POINT ( 'NONE',  ( -97.52287095715006160, -23.47596703998600631, 11.44779298504228215 ) ) ;
#11685 = CARTESIAN_POINT ( 'NONE',  ( -16.86558833231006460, 10.32443627698238409, -1.500000000000002220 ) ) ;
#11686 = ADVANCED_FACE ( 'NONE', ( #66378 ), #72483, .T. ) ;
#11687 = ORIENTED_EDGE ( 'NONE', *, *, #15552, .T. ) ;
#11688 = CARTESIAN_POINT ( 'NONE',  ( 0.7435384974594729801, 20.27106041150680937, 11.49999999999999645 ) ) ;
#11689 = CARTESIAN_POINT ( 'NONE',  ( 7.553089130262996775, 6.316227684668181297, -25.84264253713260828 ) ) ;
#11690 = ADVANCED_FACE ( 'NONE', ( #82570 ), #2976, .T. ) ;
#11691 = B_SPLINE_CURVE_WITH_KNOTS ( 'NONE', 3,
 ( #163, #22974, #53964, #68684 ),
 .UNSPECIFIED., .F., .F.,
 ( 4, 4 ),
 ( 0.4901359185396870766, 0.4991423498118026658 ),
 .UNSPECIFIED. ) ;
#11692 = ADVANCED_FACE ( 'NONE', ( #50632 ), #81084, .T. ) ;
#11693 = VECTOR ( 'NONE', #62722, 1000.000000000000114 ) ;
#11694 = VERTEX_POINT ( 'NONE', #11559 ) ;
#11695 = CARTESIAN_POINT ( 'NONE',  ( 29.80070917940689412, 6.475225279485573360, 27.39560796525321607 ) ) ;
#11696 = CARTESIAN_POINT ( 'NONE',  ( 13.86067930680217586, -3.316774720512323693, -28.23766061184436538 ) ) ;
#11697 = DIRECTION ( 'NONE',  ( -4.251773225433346808E-15, 0.000000000000000000, 1.000000000000000000 ) ) ;
#11698 = CARTESIAN_POINT ( 'NONE',  ( -44.55620429048339304, -24.64965694238574656, 8.947790433994203596 ) ) ;
#11699 = CARTESIAN_POINT ( 'NONE',  ( -96.52287095715010423, -23.48783264082477018, -1.443836473390086139 ) ) ;
#11700 = CARTESIAN_POINT ( 'NONE',  ( 11.39338536883839659, -16.50304575528446804, -1.500000000000002220 ) ) ;
#11701 = B_SPLINE_CURVE_WITH_KNOTS ( 'NONE', 3,
 ( #80722, #27929, #89828, #51269 ),
 .UNSPECIFIED., .F., .F.,
 ( 4, 4 ),
 ( 1.387778780781445521E-17, 9.999999999997510880E-05 ),
 .UNSPECIFIED. ) ;
#11702 = DIRECTION ( 'NONE',  ( 0.000000000000000000, 0.000000000000000000, -1.000000000000000000 ) ) ;
#11703 = ORIENTED_EDGE ( 'NONE', *, *, #32936, .T. ) ;
#11704 = CARTESIAN_POINT ( 'NONE',  ( -50.38822539166533687, -25.26258885410247856, 4.736250640224078268 ) ) ;
#11705 = AXIS2_PLACEMENT_3D ( 'NONE', #21042, #97677, #98665 ) ;
#11706 = CARTESIAN_POINT ( 'NONE',  ( -127.5228709571500900, -24.50216790748205398, 0.6166512839542636071 ) ) ;
#11707 = CARTESIAN_POINT ( 'NONE',  ( -23.31187512739357359, -6.376774720514425177, -17.31005501743528541 ) ) ;
#11708 = AXIS2_PLACEMENT_3D ( 'NONE', #94570, #2240, #47907 ) ;
#11709 = DIRECTION ( 'NONE',  ( -1.000000000000000000, 0.000000000000000000, 0.000000000000000000 ) ) ;
#11710 = CARTESIAN_POINT ( 'NONE',  ( -73.50728567005882041, -24.15543982623907127, -0.2315651400026654816 ) ) ;
#11711 = EDGE_CURVE ( 'NONE', #79539, #83635, #73473, .T. ) ;
#11712 = FACE_OUTER_BOUND ( 'NONE', #16184, .T. ) ;
#11713 = LINE ( 'NONE', #66041, #93882 ) ;
#11714 = EDGE_LOOP ( 'NONE', ( #96887, #74365, #98346, #41545 ) ) ;
#11715 = EDGE_CURVE ( 'NONE', #7781, #36610, #47741, .T. ) ;
#11716 = CARTESIAN_POINT ( 'NONE',  ( -19.77321833943668850, 4.698914572609424134, 11.49999999999998934 ) ) ;
#11717 = ORIENTED_EDGE ( 'NONE', *, *, #40787, .T. ) ;
#11718 = CARTESIAN_POINT ( 'NONE',  ( -18.54830753475928518, 13.48922247889305837, -1.500000000000002220 ) ) ;
#11719 = CARTESIAN_POINT ( 'NONE',  ( -32.57079420858853780, -23.48783264082477729, -1.443836473390076147 ) ) ;
#11721 = ORIENTED_EDGE ( 'NONE', *, *, #93676, .F. ) ;
#11720 = EDGE_CURVE ( 'NONE', #29710, #647, #95802, .T. ) ;
#11722 = CARTESIAN_POINT ( 'NONE',  ( -108.5228709571500616, -23.48786465467241769, 11.44779295918253936 ) ) ;
#11723 = EDGE_CURVE ( 'NONE', #56850, #4364, #11072, .T. ) ;
#11724 = LINE ( 'NONE', #50806, #9708 ) ;
#11725 = CIRCLE ( 'NONE', #68457, 6.594667762285749468 ) ;
#11726 = LINE ( 'NONE', #97949, #80431 ) ;
#11727 = CARTESIAN_POINT ( 'NONE',  ( -20.47598858559898716, 5.595549388561865456, 11.49999999999999645 ) ) ;
#11728 = CC_DESIGN_SECURITY_CLASSIFICATION ( #19830, ( #96051 ) ) ;
#11729 = CARTESIAN_POINT ( 'NONE',  ( 13.47465251475156656, -17.59220275312388182, 11.49999999999998934 ) ) ;
#11730 = CARTESIAN_POINT ( 'NONE',  ( 1.582324178664715975, -20.54890914157308401, -1.500000000000002220 ) ) ;
#11731 = ORIENTED_EDGE ( 'NONE', *, *, #54621, .F. ) ;
#11732 = CARTESIAN_POINT ( 'NONE',  ( -41.52202774044425126, -23.48783264082477729, -1.443836473390076147 ) ) ;
#11734 = ORIENTED_EDGE ( 'NONE', *, *, #98456, .F. ) ;
#11733 = VECTOR ( 'NONE', #4456, 1000.000000000000114 ) ;
#11735 = FACE_OUTER_BOUND ( 'NONE', #36249, .T. ) ;
#11736 = CARTESIAN_POINT ( 'NONE',  ( -77.55620429048342146, -23.47593901973091235, -1.443836447539004642 ) ) ;
#11737 = VERTEX_POINT ( 'NONE', #65884 ) ;
#11738 = EDGE_LOOP ( 'NONE', ( #23072, #55116, #97609, #74471 ) ) ;
#11739 = VERTEX_POINT ( 'NONE', #96806 ) ;
#11740 = VECTOR ( 'NONE', #11524, 1000.000000000000114 ) ;
#11741 = CARTESIAN_POINT ( 'NONE',  ( -77.52287095715007581, -23.73934037231757088, 11.05740245334329330 ) ) ;
#11742 = LINE ( 'NONE', #96484, #48687 ) ;
#11743 = CARTESIAN_POINT ( 'NONE',  ( 14.74567117936146943, -4.687674228468594606, -27.80582190761124650 ) ) ;
#11744 = CARTESIAN_POINT ( 'NONE',  ( 15.70846742882596025, 13.54617332914617478, -1.500000000000002220 ) ) ;
#11745 = EDGE_CURVE ( 'NONE', #54720, #100399, #27298, .T. ) ;
#11746 = CARTESIAN_POINT ( 'NONE',  ( -12.78816955685674372, 17.57309652720472570, 11.49999999999999645 ) ) ;
#11747 = ORIENTED_EDGE ( 'NONE', *, *, #91909, .F. ) ;
#11748 = CARTESIAN_POINT ( 'NONE',  ( -2.899999999999996803, 31.80000000000000071, 2.100000000000000089 ) ) ;
#11749 = CARTESIAN_POINT ( 'NONE',  ( -115.5883540308789037, -24.73486907724917927, 1.287355809206966573 ) ) ;
#11750 = CARTESIAN_POINT ( 'NONE',  ( -20.38924965233672282, -9.335317855073830273, 11.49999999999998934 ) ) ;
#11751 = DIRECTION ( 'NONE',  ( 0.000000000000000000, 0.000000000000000000, 1.000000000000000000 ) ) ;
#11752 = CARTESIAN_POINT ( 'NONE',  ( -104.5228709571500758, -29.50250786944525672, 11.44777988621623166 ) ) ;
#11753 = ORIENTED_EDGE ( 'NONE', *, *, #96875, .T. ) ;
#11754 = CARTESIAN_POINT ( 'NONE',  ( -31.52287095715006160, -29.50250786944525672, 11.44777988621624409 ) ) ;
#11755 = CARTESIAN_POINT ( 'NONE',  ( -129.6228709571500417, -24.64898659630367916, 1.056161002820834804 ) ) ;
#11756 = B_SPLINE_SURFACE_WITH_KNOTS ( 'NONE', 3, 1, ( 
 ( #15233, #78119 ),
 ( #31966, #93351 ),
 ( #77121, #46191 ),
 ( #38577, #54815 ),
 ( #61428, #38070 ),
 ( #99952, #7121 ),
 ( #92356, #39073 ),
 ( #99460, #53309 ),
 ( #70530, #8135 ),
 ( #22826, #84242 ),
 ( #30463, #93857 ),
 ( #23843, #54317 ),
 ( #53813, #14728 ),
 ( #69026, #512 ),
 ( #77622, #30959 ) ),
 .UNSPECIFIED., .F., .F., .F.,
 ( 4, 1, 1, 1, 1, 1, 1, 1, 1, 1, 1, 1, 4 ),
 ( 2, 2 ),
 ( 0.000000000000000000, 0.09870219630615274797, 0.1956723088106625263, 0.2924224265079539697, 0.3913425437998249712, 0.4444624406718897247, 0.5042287754493163243, 0.5703523379946782157, 0.6425457530977494169, 0.7222875053440166448, 0.8079211226827099912, 0.9004695379850130577, 1.000000000000000000 ),
 ( 0.000000000000000000, 1.000000000000000000 ),
 .UNSPECIFIED. ) ;
#11757 = VERTEX_POINT ( 'NONE', #73970 ) ;
#11758 = VERTEX_POINT ( 'NONE', #18673 ) ;
#11760 = EDGE_CURVE ( 'NONE', #13388, #71512, #9618, .T. ) ;
#11759 = DIRECTION ( 'NONE',  ( 1.000000000000000000, 0.000000000000000000, 0.000000000000000000 ) ) ;
#11761 = ORIENTED_EDGE ( 'NONE', *, *, #81530, .T. ) ;
#11762 = VECTOR ( 'NONE', #36257, 1000.000000000000114 ) ;
#11763 = CARTESIAN_POINT ( 'NONE',  ( 9.569808575145499319, 19.01914523534739132, -1.500000000000002220 ) ) ;
#11764 = ADVANCED_FACE ( 'NONE', ( #61753 ), #92672, .T. ) ;
#11765 = ORIENTED_EDGE ( 'NONE', *, *, #27573, .F. ) ;
#11766 = CARTESIAN_POINT ( 'NONE',  ( -100.7772468432415707, -25.12925546383932840, 7.065654974209207850 ) ) ;
#11767 = PRODUCT_DEFINITION_SHAPE ( 'NONE', 'NONE',  #100427 ) ;
#11768 = CARTESIAN_POINT ( 'NONE',  ( 19.17057494584436839, 10.47865234463220396, 11.49999999999998934 ) ) ;
#11769 = CARTESIAN_POINT ( 'NONE',  ( -68.62287095715005592, -29.50248528299804818, 1.056150453629036701 ) ) ;
#11770 = CARTESIAN_POINT ( 'NONE',  ( -2.225104987405961854, -22.55768739424384606, -1.500000000000002220 ) ) ;
#11771 = B_SPLINE_CURVE_WITH_KNOTS ( 'NONE', 3,
 ( #3910, #98222, #49582, #89134 ),
 .UNSPECIFIED., .F., .F.,
 ( 4, 4 ),
 ( 0.000000000000000000, 8.203125000004474199E-05 ),
 .UNSPECIFIED. ) ;
#11772 = CARTESIAN_POINT ( 'NONE',  ( -41.24137195392557942, -25.18430942371155723, 3.620794074174289445 ) ) ;
#11773 = DIRECTION ( 'NONE',  ( 0.000000000000000000, -1.000000000000000000, 0.000000000000000000 ) ) ;
#11774 = CARTESIAN_POINT ( 'NONE',  ( -16.30586240431254197, 14.59307310709210626, -1.500000000000002220 ) ) ;
#11775 = CARTESIAN_POINT ( 'NONE',  ( 6.996935307331598075, -5.876774720514423400, 21.22729008382901128 ) ) ;
#11776 = ORIENTED_EDGE ( 'NONE', *, *, #38663, .T. ) ;
#11777 = CARTESIAN_POINT ( 'NONE',  ( -57.62287095715004881, -23.48783264082478794, -1.443836473390068820 ) ) ;
#11778 = PLANE ( 'NONE',  #42725 ) ;
#11779 = EDGE_CURVE ( 'NONE', #8368, #27242, #39793, .T. ) ;
#11780 = ADVANCED_FACE ( 'NONE', ( #68851 ), #99769, .F. ) ;
#11781 = ORIENTED_EDGE ( 'NONE', *, *, #7617, .F. ) ;
#11782 = CARTESIAN_POINT ( 'NONE',  ( -30.63575758404999760, -23.78094912398190885, -0.9704635207981300304 ) ) ;
#11783 = VERTEX_POINT ( 'NONE', #22153 ) ;
#11784 = AXIS2_PLACEMENT_3D ( 'NONE', #90933, #28048, #14298 ) ;
#11785 = CARTESIAN_POINT ( 'NONE',  ( -43.52287095715006160, -29.50248528299804818, 1.056150453629031594 ) ) ;
#11786 = CARTESIAN_POINT ( 'NONE',  ( -20.39836507935772403, -24.35390822839723768, 2.712351064733613537 ) ) ;
#11787 = CARTESIAN_POINT ( 'NONE',  ( -3.310264809446246570, -21.00426241492911927, -1.500000000000002220 ) ) ;
#11788 = DIRECTION ( 'NONE',  ( 0.000000000000000000, 1.478457507934778393E-16, -1.000000000000000000 ) ) ;
#11789 = CARTESIAN_POINT ( 'NONE',  ( -26.36141581567544989, -24.75186187578922414, 3.275178188152123582 ) ) ;
#11790 = CARTESIAN_POINT ( 'NONE',  ( -85.50610730149335836, -24.40034930558991277, 0.3402023900116044608 ) ) ;
#11791 = CARTESIAN_POINT ( 'NONE',  ( -68.51606564171095215, -23.73766607897670156, -1.055555164236458232 ) ) ;
#11792 = CARTESIAN_POINT ( 'NONE',  ( -39.62287095715005592, -23.96177878511307568, 10.65340807706330395 ) ) ;
#11793 = VERTEX_POINT ( 'NONE', #28789 ) ;
#11794 = CARTESIAN_POINT ( 'NONE',  ( -6.365771329251782795, -18.49506561991874065, 11.49999999999999645 ) ) ;
#11795 = CARTESIAN_POINT ( 'NONE',  ( -66.62287095715005592, -24.66019654487199020, 8.947790411086131712 ) ) ;
#11796 = CARTESIAN_POINT ( 'NONE',  ( -28.59333068889780449, -24.76832095785427157, 8.029868342524341784 ) ) ;
#11797 = EDGE_LOOP ( 'NONE', ( #38353, #95631, #77279, #57961 ) ) ;
#11798 = DIRECTION ( 'NONE',  ( 0.000000000000000000, -2.173523156925979552E-06, 0.9999999999976378895 ) ) ;
#11799 = CARTESIAN_POINT ( 'NONE',  ( -99.53504363246379683, -25.25095857004948385, 5.566583656979581463 ) ) ;
#11800 = CARTESIAN_POINT ( 'NONE',  ( -8.160000000000000142, -10.15233964170348457, 0.003711184059992174607 ) ) ;
#11801 = VECTOR ( 'NONE', #23277, 1000.000000000000114 ) ;
#11802 = CARTESIAN_POINT ( 'NONE',  ( -81.73829046040381741, -25.24813826291026686, 6.803917685027681905 ) ) ;
#11803 = EDGE_CURVE ( 'NONE', #60161, #9998, #19317, .T. ) ;
#11804 = CARTESIAN_POINT ( 'NONE',  ( 17.66836560233463516, 8.693963128369697202, -1.500000000000002220 ) ) ;
#11806 = ORIENTED_EDGE ( 'NONE', *, *, #68557, .T. ) ;
#11805 = LOCAL_TIME ( 0, 54, 15.00000000000000000, #50035 ) ;
#11807 = B_SPLINE_CURVE_WITH_KNOTS ( 'NONE', 3,
 ( #21256, #4564, #4060, #90287 ),
 .UNSPECIFIED., .F., .F.,
 ( 4, 4 ),
 ( 0.000000000000000000, 0.002094050480769230060 ),
 .UNSPECIFIED. ) ;
#11808 = DIRECTION ( 'NONE',  ( 0.000000000000000000, -2.173523156925980399E-06, 0.9999999999976378895 ) ) ;
#11809 = CARTESIAN_POINT ( 'NONE',  ( 32.59332756141815679, 0.6027747205144262654, -11.41404606144462086 ) ) ;
#11810 = AXIS2_PLACEMENT_3D ( 'NONE', #95314, #72488, #20175 ) ;
#11811 = APPROVAL_ROLE ( '' ) ;
#11812 = EDGE_LOOP ( 'NONE', ( #14673, #47595, #11264, #73112 ) ) ;
#11813 = CARTESIAN_POINT ( 'NONE',  ( -54.52287095715006870, -23.47596703998600631, 11.44779298504229104 ) ) ;
#11814 = PLANE ( 'NONE',  #53950 ) ;
#11815 = CARTESIAN_POINT ( 'NONE',  ( -47.59345066694555015, -24.15543982623907127, -0.2315651400026536022 ) ) ;
#11816 = CARTESIAN_POINT ( 'NONE',  ( 5.550000000000004263, -2.000000000000001776, 19.19609335255483984 ) ) ;
#11817 = CARTESIAN_POINT ( 'NONE',  ( -105.5228709571500616, -25.00158670708909980, 2.256160236439166411 ) ) ;
#11818 = DIRECTION ( 'NONE',  ( -0.9978940991575084851, 0.000000000000000000, -0.06486421869277853025 ) ) ;
#11819 = AXIS2_PLACEMENT_3D ( 'NONE', #90631, #21107, #82024 ) ;
#11820 = CARTESIAN_POINT ( 'NONE',  ( -50.62287095715005592, -24.99132157543083821, 2.256160258750667502 ) ) ;
#11821 = CARTESIAN_POINT ( 'NONE',  ( 11.38277053702107899, 16.36964821499295653, 11.49999999999998934 ) ) ;
#11822 = CARTESIAN_POINT ( 'NONE',  ( -0.006913265320916323065, -22.96050234768690856, 3.564872121755937151 ) ) ;
#11823 = CARTESIAN_POINT ( 'NONE',  ( 8.615496892348360802, 17.92367856960711947, -1.500000000000002220 ) ) ;
#11824 = EDGE_LOOP ( 'NONE', ( #26752, #48864, #94096, #11346 ) ) ;
#11825 = CARTESIAN_POINT ( 'NONE',  ( -74.52287095715007581, -24.64898659630528854, 1.056161002820824368 ) ) ;
#11826 = DIRECTION ( 'NONE',  ( -3.773278334453079030E-23, 0.9999999999976377785, 2.173523156925979128E-06 ) ) ;
#11827 = CARTESIAN_POINT ( 'NONE',  ( 9.818046095181445665, -6.376774720513919803, -28.04791983960493695 ) ) ;
#11828 = CARTESIAN_POINT ( 'NONE',  ( -72.62287095715004170, -23.48786465467241058, 11.44779295918254647 ) ) ;
#11829 = LINE ( 'NONE', #81848, #28933 ) ;
#11830 = DIRECTION ( 'NONE',  ( -1.000000000000000000, 0.000000000000000000, -0.000000000000000000 ) ) ;
#11832 = ADVANCED_FACE ( 'NONE', ( #75444 ), #83055, .F. ) ;
#11831 = ORIENTED_EDGE ( 'NONE', *, *, #12988, .T. ) ;
#11833 = B_SPLINE_SURFACE_WITH_KNOTS ( 'NONE', 3, 3, ( 
 ( #47877, #79309, #88437, #94036 ),
 ( #18910, #63109, #49891, #40261 ),
 ( #78796, #72216, #9805, #64629 ),
 ( #2708, #24521, #34156, #65123 ),
 ( #57000, #80824, #18420, #71211 ),
 ( #1706, #10307, #55489, #49389 ),
 ( #33650, #86925, #79809, #80318 ) ),
 .UNSPECIFIED., .F., .F., .F.,
 ( 4, 3, 4 ),
 ( 4, 4 ),
 ( 0.0004766839783839991324, 0.1029713700210907190, 0.2054660560637974476 ),
 ( 0.4095981920303961021, 0.4107999044396243304 ),
 .UNSPECIFIED. ) ;
#11834 = CARTESIAN_POINT ( 'NONE',  ( -62.62287095715004881, -24.64898659630528854, 1.056161002820822592 ) ) ;
#11835 = CARTESIAN_POINT ( 'NONE',  ( -127.6236467198321805, -24.51314013834317151, 0.6176544820404252789 ) ) ;
#11836 = VERTEX_POINT ( 'NONE', #22649 ) ;
#11837 = CARTESIAN_POINT ( 'NONE',  ( -2.479824388263708990, 20.08073137130260122, 11.49999999999998934 ) ) ;
#11838 = CARTESIAN_POINT ( 'NONE',  ( 7.478911390063968767, -5.876774720514422512, 20.82112274756839199 ) ) ;
#11839 = CARTESIAN_POINT ( 'NONE',  ( -112.6228709571500559, -29.50247984919015209, -1.443849546365048253 ) ) ;
#11840 = VECTOR ( 'NONE', #71417, 1000.000000000000114 ) ;
#11841 = ADVANCED_FACE ( 'NONE', ( #14553 ), #60255, .T. ) ;
#11842 = EDGE_CURVE ( 'NONE', #16998, #48696, #99090, .T. ) ;
#11843 = CARTESIAN_POINT ( 'NONE',  ( -109.6228709571500559, -24.64898659630368627, 1.056161002820831474 ) ) ;
#11844 = ADVANCED_FACE ( 'NONE', ( #53641 ), #99287, .F. ) ;
#11845 = ORIENTED_EDGE ( 'NONE', *, *, #17500, .F. ) ;
#11846 = CARTESIAN_POINT ( 'NONE',  ( -46.62287095715004170, -23.72773821059535138, 11.05748984161097503 ) ) ;
#11847 = CARTESIAN_POINT ( 'NONE',  ( -2.243088942307695177, -6.376774720514408301, 19.14743589743590491 ) ) ;
#11848 = CARTESIAN_POINT ( 'NONE',  ( -6.237196068801617699, -19.06703463882530158, -1.500000000000002220 ) ) ;
#11849 = AXIS2_PLACEMENT_3D ( 'NONE', #18564, #28184, #4358 ) ;
#11850 = CARTESIAN_POINT ( 'NONE',  ( -6.845587600281468177, 19.88882266644084496, 11.49999999999999645 ) ) ;
#11851 = EDGE_CURVE ( 'NONE', #27461, #82473, #6451, .T. ) ;
#11852 = CARTESIAN_POINT ( 'NONE',  ( 9.948453975742596711, 5.965225279485574461, -28.04422933552663366 ) ) ;
#11853 = CARTESIAN_POINT ( 'NONE',  ( -70.55922311016780668, -23.85049219812685806, 10.88485053497527311 ) ) ;
#11854 = CARTESIAN_POINT ( 'NONE',  ( 11.82310115920509830, 18.66461490495635545, 11.49999999999998934 ) ) ;
#11855 = CARTESIAN_POINT ( 'NONE',  ( -40.11299260137283795, -25.27806099098225090, 5.047402397866858514 ) ) ;
#11856 = DIRECTION ( 'NONE',  ( -3.773278334453079618E-23, 0.9999999999976377785, 2.173523156925979975E-06 ) ) ;
#11857 = CARTESIAN_POINT ( 'NONE',  ( -0.02075734969026423599, -5.965225279485572685, -28.54397719988136828 ) ) ;
#11858 = FACE_OUTER_BOUND ( 'NONE', #35810, .T. ) ;
#11859 = DIRECTION ( 'NONE',  ( -0.000000000000000000, -1.000000000000000000, -0.000000000000000000 ) ) ;
#11860 = ORIENTED_EDGE ( 'NONE', *, *, #7905, .T. ) ;
#11861 = ORIENTED_EDGE ( 'NONE', *, *, #77949, .T. ) ;
#11862 = DIRECTION ( 'NONE',  ( -0.000000000000000000, 1.000000000000000000, -0.000000000000000000 ) ) ;
#11863 = B_SPLINE_CURVE_WITH_KNOTS ( 'NONE', 3,
 ( #52273, #36536, #19806, #89338 ),
 .UNSPECIFIED., .F., .F.,
 ( 4, 4 ),
 ( 0.4308076291828551452, 0.4398140604549706789 ),
 .UNSPECIFIED. ) ;
#11864 = CYLINDRICAL_SURFACE ( 'NONE', #21055, 0.8500000000000017542 ) ;
#11865 = LINE ( 'NONE', #57565, #32533 ) ;
#11866 = CARTESIAN_POINT ( 'NONE',  ( 18.80685554986811070, -8.408966509905500430, -1.500000000000002220 ) ) ;
#11867 = EDGE_CURVE ( 'NONE', #98373, #68666, #61255, .T. ) ;
#11868 = CARTESIAN_POINT ( 'NONE',  ( 21.48638754631891246, 1.654510534108022179, 11.49999999999999645 ) ) ;
#11869 = VERTEX_POINT ( 'NONE', #21654 ) ;
#11870 = DIRECTION ( 'NONE',  ( 0.000000000000000000, -0.9999999999976377785, -2.173523156925979128E-06 ) ) ;
#11871 = DIRECTION ( 'NONE',  ( -0.000000000000000000, -1.000000000000000000, -0.000000000000000000 ) ) ;
#11872 = CARTESIAN_POINT ( 'NONE',  ( -28.98875734969026041, -0.3587747205144262708, 23.37402280011862743 ) ) ;
#11873 = CARTESIAN_POINT ( 'NONE',  ( -2.938769918389303459, -22.12206158279486345, 11.49999999999998934 ) ) ;
#11875 = CARTESIAN_POINT ( 'NONE',  ( 29.71114493364435916, -4.339464138238508184, 27.93491297891351621 ) ) ;
#11874 = VECTOR ( 'NONE', #78078, 1000.000000000000000 ) ;
#11876 = CARTESIAN_POINT ( 'NONE',  ( 26.14999174255633463, -4.132774720517320866, -11.56127575336603286 ) ) ;
#11877 = EDGE_CURVE ( 'NONE', #79347, #97718, #55645, .T. ) ;
#11878 = VERTEX_POINT ( 'NONE', #77937 ) ;
#11879 = CARTESIAN_POINT ( 'NONE',  ( -101.6228709571500701, -23.96127896941631619, -0.6493128931037793761 ) ) ;
#11880 = CARTESIAN_POINT ( 'NONE',  ( 3.206569032998081603, -5.876774720514424288, 21.19686455982786200 ) ) ;
#11881 = CARTESIAN_POINT ( 'NONE',  ( 4.135342931496230001, -20.44547621892628797, -1.500000000000002220 ) ) ;
#11882 = ORIENTED_EDGE ( 'NONE', *, *, #51604, .T. ) ;
#11885 = EDGE_LOOP ( 'NONE', ( #38242, #60679, #35838, #14510 ) ) ;
#11884 = EDGE_CURVE ( 'NONE', #17017, #91742, #9946, .T. ) ;
#11883 = CARTESIAN_POINT ( 'NONE',  ( -39.08733197973624840, -25.25129735365466388, 3.851328594451885134 ) ) ;
#11886 = ORIENTED_EDGE ( 'NONE', *, *, #65677, .T. ) ;
#11887 = AXIS2_PLACEMENT_3D ( 'NONE', #5708, #4724, #67135 ) ;
#11888 = CARTESIAN_POINT ( 'NONE',  ( -50.65607660699232895, -25.30191415566046587, 4.703207432804873633 ) ) ;
#11889 = CARTESIAN_POINT ( 'NONE',  ( 13.75562813033083742, -15.94169299924578453, -1.500000000000002220 ) ) ;
#11890 = EDGE_LOOP ( 'NONE', ( #75611, #59678 ) ) ;
#11891 = CARTESIAN_POINT ( 'NONE',  ( -114.6228709571500559, -24.64965695001469115, 8.947790433994176951 ) ) ;
#11892 = PLANE ( 'NONE',  #19032 ) ;
#11893 = CARTESIAN_POINT ( 'NONE',  ( -120.5539051758846085, -24.52399227489125266, 9.353111116836528183 ) ) ;
#11894 = AXIS2_PLACEMENT_3D ( 'NONE', #55990, #31123, #17408 ) ;
#11895 = CARTESIAN_POINT ( 'NONE',  ( -81.42380231474228935, -25.30401792888237011, 5.197789011716578145 ) ) ;
#11896 = FACE_OUTER_BOUND ( 'NONE', #29518, .T. ) ;
#11897 = CARTESIAN_POINT ( 'NONE',  ( -18.02536786162489335, -12.12045427182966861, -1.500000000000002220 ) ) ;
#11898 = LINE ( 'NONE', #5282, #72473 ) ;
#11900 = VERTEX_POINT ( 'NONE', #17054 ) ;
#11899 = CARTESIAN_POINT ( 'NONE',  ( -19.27636426328722763, -11.15942449563467775, 11.49999999999999645 ) ) ;
#11901 = CARTESIAN_POINT ( 'NONE',  ( -72.62287095715004170, -23.48786465467241058, 11.44779295918254647 ) ) ;
#11902 = B_SPLINE_CURVE_WITH_KNOTS ( 'NONE', 3,
 ( #21389, #83804, #14284, #61486, #31017, #37631, #13783, #99513, #69080, #68094, #52867, #67601, #68589, #44260, #75189, #84297, #52366, #77177 ),
 .UNSPECIFIED., .F., .F.,
 ( 4, 2, 2, 2, 2, 2, 2, 2, 4 ),
 ( 0.000000000000000000, 0.0002613877182136167495, 0.0005227754364272334990, 0.0007841631546408503028, 0.001045550872854466998, 0.001306938591068083693, 0.001568326309281700606, 0.001829714027495317301, 0.002091101745708933996 ),
 .UNSPECIFIED. ) ;
#11903 = DIRECTION ( 'NONE',  ( -0.000000000000000000, -1.000000000000000000, -0.000000000000000000 ) ) ;
#11904 = LINE ( 'NONE', #67708, #40809 ) ;
#11906 = ORIENTED_EDGE ( 'NONE', *, *, #50651, .T. ) ;
#11905 = EDGE_CURVE ( 'NONE', #52201, #11694, #42973, .T. ) ;
#11907 = EDGE_CURVE ( 'NONE', #90367, #95277, #86571, .T. ) ;
#11909 = VERTEX_POINT ( 'NONE', #62248 ) ;
#11908 = CARTESIAN_POINT ( 'NONE',  ( -40.62287095715008434, -24.92579138211018730, 1.929029949965663349 ) ) ;
#11910 = VERTEX_POINT ( 'NONE', #1846 ) ;
#11911 = CARTESIAN_POINT ( 'NONE',  ( -75.52287095715007581, -24.83602698348160942, 1.605859176311265069 ) ) ;
#11912 = B_SPLINE_CURVE_WITH_KNOTS ( 'NONE', 3,
 ( #46674, #40056, #22307, #24322, #93836, #7598, #77597, #53285, #8101, #38550, #39050, #78094, #8608, #39553 ),
 .UNSPECIFIED., .F., .F.,
 ( 4, 2, 2, 2, 2, 2, 4 ),
 ( 0.000000000000000000, 0.0001870305922025326481, 0.0003740611844050652961, 0.0007481223688101111850, 0.001122183553215157182, 0.001309214145417679585, 0.001496244737620201770 ),
 .UNSPECIFIED. ) ;
#11913 = CARTESIAN_POINT ( 'NONE',  ( -64.52287095715006160, -24.64898659630528854, 1.056161002820822592 ) ) ;
#11914 = B_SPLINE_CURVE_WITH_KNOTS ( 'NONE', 3,
 ( #1517, #61034, #91965, #40578 ),
 .UNSPECIFIED., .F., .F.,
 ( 4, 4 ),
 ( 0.000000000000000000, 9.999999999998897304E-05 ),
 .UNSPECIFIED. ) ;
#11915 = CARTESIAN_POINT ( 'NONE',  ( 31.55507366846311967, 4.132774720514426292, -2.076992067079099336 ) ) ;
#11916 = CARTESIAN_POINT ( 'NONE',  ( 2.246611357655420083, 0.1632191352058106337, 0.1632191352058112166 ) ) ;
#11917 = ORIENTED_EDGE ( 'NONE', *, *, #99818, .F. ) ;
#11918 = CARTESIAN_POINT ( 'NONE',  ( -130.5728709571501156, -24.38618449965941082, 9.939220798225495201 ) ) ;
#11919 = CARTESIAN_POINT ( 'NONE',  ( 1.585521478320181865, 22.38520322874704149, -1.500000000000002220 ) ) ;
#11920 = VERTEX_POINT ( 'NONE', #85566 ) ;
#11921 = DIRECTION ( 'NONE',  ( 0.000000000000000000, 0.000000000000000000, -1.000000000000000000 ) ) ;
#11923 = CARTESIAN_POINT ( 'NONE',  ( -101.5932190732468712, -23.96169478059713853, 10.65365249895717881 ) ) ;
#11922 = VECTOR ( 'NONE', #75025, 1000.000000000000000 ) ;
#11924 = CARTESIAN_POINT ( 'NONE',  ( 10.73283225829863952, 3.316774720511335595, -27.03068772560423838 ) ) ;
#11925 = CARTESIAN_POINT ( 'NONE',  ( 13.36367879947601445, -5.876774720514426953, 20.00000000000000355 ) ) ;
#11926 = CARTESIAN_POINT ( 'NONE',  ( -130.5728709571500588, -24.66513809378597344, 8.909134979017300893 ) ) ;
#11927 = CARTESIAN_POINT ( 'NONE',  ( -5.058734511472819051, -18.94576116945722788, -1.500000000000002220 ) ) ;
#11928 = VECTOR ( 'NONE', #74382, 1000.000000000000000 ) ;
#11929 = DIRECTION ( 'NONE',  ( 0.000000000000000000, 1.478457507934778393E-16, -1.000000000000000000 ) ) ;
#11930 = VERTEX_POINT ( 'NONE', #48528 ) ;
#11931 = CARTESIAN_POINT ( 'NONE',  ( 15.50980990363467882, 14.95361599516425244, 11.49999999999998934 ) ) ;
#11932 = CARTESIAN_POINT ( 'NONE',  ( 12.16765770914787304, -5.965225279485572685, -27.57618308014988173 ) ) ;
#11933 = CARTESIAN_POINT ( 'NONE',  ( -71.23336565260535735, -25.12219025383727455, 6.552467362938464213 ) ) ;
#11934 = CARTESIAN_POINT ( 'NONE',  ( -32.99388727629348494, -29.50248914092071928, 2.831113219569932227 ) ) ;
#11935 = DIRECTION ( 'NONE',  ( -3.773278334453079618E-23, 0.9999999999976377785, 2.173523156925978705E-06 ) ) ;
#11936 = CARTESIAN_POINT ( 'NONE',  ( 22.97298546869389568, 1.202750762487129199, -1.500000000000002220 ) ) ;
#11937 = PERSON_AND_ORGANIZATION_ROLE ( 'design_supplier' ) ;
#11938 = DIRECTION ( 'NONE',  ( 0.000000000000000000, 0.000000000000000000, -1.000000000000000000 ) ) ;
#11939 = CARTESIAN_POINT ( 'NONE',  ( -49.61440498689717060, -23.48783264082477018, -1.443836473390093911 ) ) ;
#11940 = CARTESIAN_POINT ( 'NONE',  ( -4.889416449700032530, -19.50743224814450016, 11.49999999999999645 ) ) ;
#11941 = CARTESIAN_POINT ( 'NONE',  ( 5.088854283150510582, 3.311779300275201177, -27.56292346345011524 ) ) ;
#11942 = LINE ( 'NONE', #58626, #32272 ) ;
#11943 = DIRECTION ( 'NONE',  ( 1.084136044942898696E-16, 0.000000000000000000, -1.000000000000000000 ) ) ;
#11944 = DIRECTION ( 'NONE',  ( -3.773278334444166432E-23, 1.000000000000000000, 0.000000000000000000 ) ) ;
#11945 = DIRECTION ( 'NONE',  ( -1.000000000000000000, -3.773278334444166432E-23, -8.201307841325785021E-29 ) ) ;
#11946 = CARTESIAN_POINT ( 'NONE',  ( -13.56193660873917395, -14.51407242162769151, -1.500000000000002220 ) ) ;
#11947 = CARTESIAN_POINT ( 'NONE',  ( -113.5154190852081797, -24.51314013834315375, 0.6176544820404169522 ) ) ;
#11948 = CARTESIAN_POINT ( 'NONE',  ( -9.502044936771568473, -17.27029980899984452, -1.500000000000002220 ) ) ;
#11949 = CARTESIAN_POINT ( 'NONE',  ( -91.12544711349063675, -25.37321702313245453, 5.213201572634361014 ) ) ;
#11950 = APPROVAL_DATE_TIME ( #94686, #36350 ) ;
#11951 = FACE_OUTER_BOUND ( 'NONE', #62292, .T. ) ;
#11952 = CARTESIAN_POINT ( 'NONE',  ( -79.52287095715006160, -24.64965694238575011, 8.947790433994198267 ) ) ;
#11953 = CARTESIAN_POINT ( 'NONE',  ( -0.003042231299257275486, -20.61035990087709635, 11.49999999999999645 ) ) ;
#11954 = DIRECTION ( 'NONE',  ( -1.000000000000000000, 0.000000000000000000, -0.000000000000000000 ) ) ;
#11955 = AXIS2_PLACEMENT_3D ( 'NONE', #3467, #3960, #51628 ) ;
#11956 = CARTESIAN_POINT ( 'NONE',  ( -16.08347380570801377, -15.98036338121420030, 11.49999999999999645 ) ) ;
#11957 = ORIENTED_EDGE ( 'NONE', *, *, #40647, .F. ) ;
#11958 = CARTESIAN_POINT ( 'NONE',  ( 10.86264265030973952, -0.3587747205144257157, -28.64597719988137570 ) ) ;
#11959 = B_SPLINE_CURVE_WITH_KNOTS ( 'NONE', 3,
 ( #86208, #48670, #94815, #70489, #62378, #70994, #71998 ),
 .UNSPECIFIED., .F., .F.,
 ( 4, 1, 1, 1, 4 ),
 ( 0.3452202732246780759, 0.4949101844912719983, 0.6446000957578658097, 0.7942900070244596211, 0.9439799182910535436 ),
 .UNSPECIFIED. ) ;
#11961 = EDGE_CURVE ( 'NONE', #77504, #28708, #78445, .T. ) ;
#11960 = CARTESIAN_POINT ( 'NONE',  ( 30.60862754225505000, 4.127879075750807480, 27.06827100787837992 ) ) ;
#11962 = VECTOR ( 'NONE', #43631, 1000.000000000000000 ) ;
#11963 = EDGE_CURVE ( 'NONE', #66746, #65800, #8344, .T. ) ;
#11964 = CARTESIAN_POINT ( 'NONE',  ( -26.98635835925963633, -24.93063604734380689, 8.112878671671195363 ) ) ;
#11965 = EDGE_CURVE ( 'NONE', #69536, #9262, #16800, .T. ) ;
#11966 = CARTESIAN_POINT ( 'NONE',  ( -104.6228709571500559, -29.50248528299804818, 1.056150453629042030 ) ) ;
#11967 = EDGE_CURVE ( 'NONE', #73710, #88129, #40404, .T. ) ;
#11968 = ORIENTED_EDGE ( 'NONE', *, *, #15557, .F. ) ;
#11969 = ADVANCED_FACE ( 'NONE', ( #47521 ), #7942, .T. ) ;
#11970 = ORIENTED_EDGE ( 'NONE', *, *, #1033, .T. ) ;
#11971 = CARTESIAN_POINT ( 'NONE',  ( 0.3910256410256418569, -6.376774720514420736, 20.67377804487180271 ) ) ;
#11972 = CARTESIAN_POINT ( 'NONE',  ( 18.61037501828884189, -13.27421459584354579, 11.49999999999998934 ) ) ;
#11973 = CARTESIAN_POINT ( 'NONE',  ( 13.91401389203221406, -5.965225279485572685, 158.0376437107427137 ) ) ;
#11974 = CARTESIAN_POINT ( 'NONE',  ( 21.29926025483437257, -3.289820829717503337, -1.500000000000002220 ) ) ;
#11975 = LINE ( 'NONE', #26706, #77146 ) ;
#11976 = CARTESIAN_POINT ( 'NONE',  ( 5.202077965628057576, -7.402934475628873363E-15, 2.038091937962834166 ) ) ;
#11977 = CARTESIAN_POINT ( 'NONE',  ( -21.69688529672534827, 6.072505851105969299, 11.49999999999999645 ) ) ;
#11978 = VERTEX_POINT ( 'NONE', #33278 ) ;
#11979 = LINE ( 'NONE', #94714, #59490 ) ;
#11980 = CARTESIAN_POINT ( 'NONE',  ( 3.092608977599853315, -21.74436839971096802, -1.500000000000002220 ) ) ;
#11981 = DIRECTION ( 'NONE',  ( -0.000000000000000000, 1.000000000000000000, -0.000000000000000000 ) ) ;
#11982 = DIRECTION ( 'NONE',  ( 0.000000000000000000, -0.9999999999976377785, -2.173523156925979975E-06 ) ) ;
#11983 = VERTEX_POINT ( 'NONE', #70857 ) ;
#11984 = CARTESIAN_POINT ( 'NONE',  ( -28.62287095715004881, -23.31957264754183967, 11.44779298504227860 ) ) ;
#11985 = CARTESIAN_POINT ( 'NONE',  ( 12.92500000000000249, 14.50000000000000000, 24.00000000000000000 ) ) ;
#11986 = ORIENTED_EDGE ( 'NONE', *, *, #11720, .T. ) ;
#11987 = DIRECTION ( 'NONE',  ( 1.000000000000000000, 3.773278334444166432E-23, 8.201307841325785021E-29 ) ) ;
#11988 = VERTEX_POINT ( 'NONE', #94175 ) ;
#11989 = VERTEX_POINT ( 'NONE', #64266 ) ;
#11990 = ORIENTED_EDGE ( 'NONE', *, *, #98220, .T. ) ;
#11991 = DIRECTION ( 'NONE',  ( -0.03244919754393515293, 0.000000000000000000, 0.9994733861282923959 ) ) ;
#11992 = DIRECTION ( 'NONE',  ( -1.000000000000000000, -3.773278334444167608E-23, -8.201307833595939069E-29 ) ) ;
#11993 = CARTESIAN_POINT ( 'NONE',  ( 14.56700794487394290, 4.079493581517789735, -28.22524715676654239 ) ) ;
#11994 = CARTESIAN_POINT ( 'NONE',  ( 13.37706023731332827, -15.40713922116925616, -1.500000000000002220 ) ) ;
#11995 = AXIS2_PLACEMENT_3D ( 'NONE', #55922, #64552, #1123 ) ;
#11996 = ORIENTED_EDGE ( 'NONE', *, *, #46800, .F. ) ;
#11997 = CARTESIAN_POINT ( 'NONE',  ( -70.95580061108532277, -25.06113984836056119, 7.428384239504691067 ) ) ;
#11998 = FACE_OUTER_BOUND ( 'NONE', #45787, .T. ) ;
#11999 = CARTESIAN_POINT ( 'NONE',  ( -105.5186488368198496, -23.85016227208580730, -0.8807180028928328630 ) ) ;
#12000 = CARTESIAN_POINT ( 'NONE',  ( -71.70128661679227378, -25.03149591267348484, 6.373708887022837111 ) ) ;
#12001 = ADVANCED_FACE ( 'NONE', ( #94679 ), #46512, .F. ) ;
#12002 = ORIENTED_EDGE ( 'NONE', *, *, #99846, .F. ) ;
#12003 = CARTESIAN_POINT ( 'NONE',  ( -28.45618646431091392, -25.21531712953401083, 2.526464341324828666 ) ) ;
#12005 = AXIS2_PLACEMENT_3D ( 'NONE', #6734, #83357, #44817 ) ;
#12004 = CARTESIAN_POINT ( 'NONE',  ( -87.62287095715004170, -23.47593901973091235, -1.443836447539002865 ) ) ;
#12006 = ORIENTED_EDGE ( 'NONE', *, *, #14721, .F. ) ;
#12007 = CARTESIAN_POINT ( 'NONE',  ( -8.830788454959730416, 18.81286502489961876, 11.49999999999998934 ) ) ;
#12008 = B_SPLINE_CURVE_WITH_KNOTS ( 'NONE', 3,
 ( #6800, #5807, #99142, #44888, #53501, #43389 ),
 .UNSPECIFIED., .F., .F.,
 ( 4, 2, 4 ),
 ( 0.07707475098329773233, 0.07906619944496928731, 0.08105764790664082842 ),
 .UNSPECIFIED. ) ;
#12009 = ORIENTED_EDGE ( 'NONE', *, *, #6101, .T. ) ;
#12011 = EDGE_LOOP ( 'NONE', ( #62169, #54783, #96226, #2909 ) ) ;
#12010 = FACE_OUTER_BOUND ( 'NONE', #21465, .T. ) ;
#12012 = CARTESIAN_POINT ( 'NONE',  ( -28.98875734969026041, 0.3587747205144262708, 15.62202280011862321 ) ) ;
#12013 = DIRECTION ( 'NONE',  ( -0.000000000000000000, 1.000000000000000000, -0.000000000000000000 ) ) ;
#12014 = ORIENTED_EDGE ( 'NONE', *, *, #90736, .F. ) ;
#12015 = ORIENTED_EDGE ( 'NONE', *, *, #2752, .F. ) ;
#12016 = PLANE ( 'NONE',  #29944 ) ;
#12017 = CARTESIAN_POINT ( 'NONE',  ( 10.86264265030973952, 5.965225279485574461, -27.62597719988137612 ) ) ;
#12018 = LINE ( 'NONE', #98241, #11241 ) ;
#12019 = CARTESIAN_POINT ( 'NONE',  ( -70.46019744876114999, -25.24515042775860962, 5.316128055210258552 ) ) ;
#12021 = VERTEX_POINT ( 'NONE', #77441 ) ;
#12020 = CARTESIAN_POINT ( 'NONE',  ( 19.90762846840230083, -9.494064324355022677, 11.49999999999999645 ) ) ;
#12022 = DIRECTION ( 'NONE',  ( -0.000000000000000000, -0.000000000000000000, -1.000000000000000000 ) ) ;
#12023 = CARTESIAN_POINT ( 'NONE',  ( 16.66146196086182130, -15.28366505690825328, 11.49999999999998934 ) ) ;
#12024 = EDGE_CURVE ( 'NONE', #53428, #64023, #66435, .T. ) ;
#12026 = ORIENTED_EDGE ( 'NONE', *, *, #46684, .F. ) ;
#12025 = DIRECTION ( 'NONE',  ( 0.000000000000000000, -0.9999999999976377785, -2.173523156925979128E-06 ) ) ;
#12027 = ORIENTED_EDGE ( 'NONE', *, *, #31718, .T. ) ;
#12028 = CARTESIAN_POINT ( 'NONE',  ( -120.6228709571500417, -29.50250786944525672, 11.44777988621622811 ) ) ;
#12029 = ADVANCED_FACE ( 'NONE', ( #87070 ), #73730, .F. ) ;
#12030 = B_SPLINE_SURFACE_WITH_KNOTS ( 'NONE', 3, 3, ( 
 ( #82562, #13044, #13541, #5441 ),
 ( #75436, #5936, #36892, #67856 ),
 ( #98777, #29277, #91172, #52619 ),
 ( #83555, #53132, #45517, #31271 ),
 ( #99762, #16536, #84557, #39887 ),
 ( #94168, #325, #76932, #62240 ),
 ( #30775, #15542, #30268, #93160 ) ),
 .UNSPECIFIED., .F., .F., .F.,
 ( 4, 3, 4 ),
 ( 4, 4 ),
 ( 0.7945040050992238090, 0.8970133687736498995, 0.9995227324480758790 ),
 ( 0.3395802893024847946, 0.3407497866532611663 ),
 .UNSPECIFIED. ) ;
#12031 = FACE_OUTER_BOUND ( 'NONE', #58687, .T. ) ;
#12032 = VERTEX_POINT ( 'NONE', #47018 ) ;
#12033 = CARTESIAN_POINT ( 'NONE',  ( -3.044128750896296420, -20.94304649679510888, 11.49999999999998934 ) ) ;
#12034 = LINE ( 'NONE', #66352, #70271 ) ;
#12035 = CARTESIAN_POINT ( 'NONE',  ( -1.675486951385420475, 10.82748519320431591, 3.549999999999999822 ) ) ;
#12036 = CARTESIAN_POINT ( 'NONE',  ( 15.88595335714125589, -15.59144682577495189, -1.500000000000002220 ) ) ;
#12037 = CARTESIAN_POINT ( 'NONE',  ( -46.62287095715006302, -24.33832256526968862, 0.1851278514119869822 ) ) ;
#12038 = ORIENTED_EDGE ( 'NONE', *, *, #58278, .T. ) ;
#12039 = CARTESIAN_POINT ( 'NONE',  ( -78.52287095715006160, -23.47593901973090169, -1.443836447538996648 ) ) ;
#12040 = CARTESIAN_POINT ( 'NONE',  ( -96.52287095715006160, -29.50248528299804818, 1.056150453629042030 ) ) ;
#12041 = CARTESIAN_POINT ( 'NONE',  ( -27.61845239340658154, -0.3587747205144057872, -10.37513603161905706 ) ) ;
#12042 = CARTESIAN_POINT ( 'NONE',  ( -45.52287095715006160, -23.47596703998600631, 11.44779298504229104 ) ) ;
#12043 = CARTESIAN_POINT ( 'NONE',  ( -19.43040671759091609, -1.856541507571394467, 11.49999999999998934 ) ) ;
#12044 = CARTESIAN_POINT ( 'NONE',  ( 11.41860910855227829, 18.14899599152127152, -1.500000000000002220 ) ) ;
#12045 = CARTESIAN_POINT ( 'NONE',  ( -26.06135888742384665, -24.92774869473493027, 2.563275193131095087 ) ) ;
#12046 = DIRECTION ( 'NONE',  ( -3.773278334453079618E-23, 0.9999999999976377785, 2.173523156925979975E-06 ) ) ;
#12047 = CARTESIAN_POINT ( 'NONE',  ( -77.55422962360664485, -23.96119346886880663, -0.6495511937832126881 ) ) ;
#12049 = VECTOR ( 'NONE', #29031, 1000.000000000000000 ) ;
#12048 = CARTESIAN_POINT ( 'NONE',  ( 21.14626179850551324, 8.528272852130310611, -1.500000000000002220 ) ) ;
#12050 = CARTESIAN_POINT ( 'NONE',  ( -106.6321266654194631, -23.73791477778912551, 11.05961554403169878 ) ) ;
#12051 = DIRECTION ( 'NONE',  ( -0.6392559695863496705, -6.845827386180411947E-16, -0.7689940216596069522 ) ) ;
#12052 = CARTESIAN_POINT ( 'NONE',  ( -5.841000908416043913, -19.03464889989004050, 11.49999999999999645 ) ) ;
#12053 = DIRECTION ( 'NONE',  ( -1.000000000000000000, -3.773278334444166432E-23, -8.201307841325785021E-29 ) ) ;
#12054 = CARTESIAN_POINT ( 'NONE',  ( -39.53338521000194561, -24.51419770103158413, 9.386484678747189392 ) ) ;
#12055 = CARTESIAN_POINT ( 'NONE',  ( -101.6228709571500559, -24.33832256526968862, 0.1851278514119917562 ) ) ;
#12056 = ORIENTED_EDGE ( 'NONE', *, *, #28018, .T. ) ;
#12057 = DIRECTION ( 'NONE',  ( 0.000000000000000000, 0.000000000000000000, 1.000000000000000000 ) ) ;
#12058 = CARTESIAN_POINT ( 'NONE',  ( -62.62287095715009144, -24.33927499327853994, 9.819080762295820719 ) ) ;
#12059 = VECTOR ( 'NONE', #47578, 1000.000000000000000 ) ;
#12060 = CARTESIAN_POINT ( 'NONE',  ( -4.559408409702599307, -21.23122434433648209, 11.49999999999998934 ) ) ;
#12061 = LINE ( 'NONE', #27794, #59341 ) ;
#12062 = CARTESIAN_POINT ( 'NONE',  ( 3.994393897313025743, -19.14333888664780048, -1.500000000000002220 ) ) ;
#12063 = CYLINDRICAL_SURFACE ( 'NONE', #62014, 11.85241003308276042 ) ;
#12064 = APPROVAL_ROLE ( '' ) ;
#12065 = CARTESIAN_POINT ( 'NONE',  ( -51.55620429048339304, -24.66019654487199020, 8.947790411086133489 ) ) ;
#12066 = CARTESIAN_POINT ( 'NONE',  ( 20.41236503877875563, 1.188189311754236144, 11.49999999999999645 ) ) ;
#12067 = CARTESIAN_POINT ( 'NONE',  ( 9.051621769697627329, -6.475225279485570695, -27.04979394446680274 ) ) ;
#12068 = DIRECTION ( 'NONE',  ( -1.000000000000000000, -3.773278334444167608E-23, -8.201307810031802745E-29 ) ) ;
#12069 = ORIENTED_EDGE ( 'NONE', *, *, #44163, .T. ) ;
#12070 = CARTESIAN_POINT ( 'NONE',  ( 0.4325450954222598288, 2.349999999999997868, 2.877919977996277362E-16 ) ) ;
#12071 = CARTESIAN_POINT ( 'NONE',  ( -53.52287095715006870, -29.50250786944525672, 11.44777988621624054 ) ) ;
#12073 = ADVANCED_FACE ( 'NONE', ( #96193 ), #26173, .T. ) ;
#12072 = PLANE ( 'NONE',  #48491 ) ;
#12074 = CARTESIAN_POINT ( 'NONE',  ( -35.52287095715006870, -29.50248789122583659, 2.256150453626215580 ) ) ;
#12076 = ORIENTED_EDGE ( 'NONE', *, *, #34893, .F. ) ;
#12075 = EDGE_CURVE ( 'NONE', #19028, #8399, #34961, .T. ) ;
#12077 = FACE_OUTER_BOUND ( 'NONE', #8992, .T. ) ;
#12078 = EDGE_CURVE ( 'NONE', #14465, #39424, #11447, .T. ) ;
#12079 = CARTESIAN_POINT ( 'NONE',  ( -16.20615075098634961, 16.30094363606528418, 11.49999999999999645 ) ) ;
#12080 = CARTESIAN_POINT ( 'NONE',  ( -0.9122204482399535186, 22.77315974801211240, 11.49999999999998934 ) ) ;
#12081 = CARTESIAN_POINT ( 'NONE',  ( 4.736659488006659480, -6.376774720514420736, 21.25082490164487581 ) ) ;
#12082 = EDGE_CURVE ( 'NONE', #43735, #58649, #84545, .T. ) ;
#12083 = DIRECTION ( 'NONE',  ( -0.9952638024365006997, 0.000000000000000000, -0.09721092304694052555 ) ) ;
#12084 = DIRECTION ( 'NONE',  ( -3.773278334444166432E-23, 1.000000000000000000, 0.000000000000000000 ) ) ;
#12085 = AXIS2_PLACEMENT_3D ( 'NONE', #62111, #69209, #77797 ) ;
#12086 = CARTESIAN_POINT ( 'NONE',  ( -100.6814946224345846, -25.31267346029541443, 4.736250531364077254 ) ) ;
#12087 = ADVANCED_FACE ( 'NONE', ( #58141 ), #54703, .T. ) ;
#12088 = FACE_OUTER_BOUND ( 'NONE', #15753, .T. ) ;
#12089 = B_SPLINE_CURVE_WITH_KNOTS ( 'NONE', 3,
 ( #12452, #94820, #70998, #74355 ),
 .UNSPECIFIED., .F., .F.,
 ( 4, 4 ),
 ( 0.4490887540585746796, 0.4500895010993400946 ),
 .UNSPECIFIED. ) ;
#12090 = CARTESIAN_POINT ( 'NONE',  ( -20.59625928752216240, -7.366027188055905839, -1.500000000000002220 ) ) ;
#12091 = CARTESIAN_POINT ( 'NONE',  ( -16.89397143409390623, -6.376774720514426953, 16.89397143409405899 ) ) ;
#12092 = CARTESIAN_POINT ( 'NONE',  ( -101.5228709571500758, -24.65952944569304606, 1.056160979905702346 ) ) ;
#12093 = DIRECTION ( 'NONE',  ( 0.9951627101165076983, -0.09824042138329622254, 0.000000000000000000 ) ) ;
#12094 = DIRECTION ( 'NONE',  ( 0.000000000000000000, 0.000000000000000000, -1.000000000000000000 ) ) ;
#12095 = VERTEX_POINT ( 'NONE', #43411 ) ;
#12096 = CARTESIAN_POINT ( 'NONE',  ( -12.60687543931603471, -16.05746371069360379, 11.49999999999998934 ) ) ;
#12097 = ORIENTED_EDGE ( 'NONE', *, *, #91833, .T. ) ;
#12098 = ORIENTED_EDGE ( 'NONE', *, *, #15189, .T. ) ;
#12099 = ORIENTED_EDGE ( 'NONE', *, *, #38903, .T. ) ;
#12101 = ADVANCED_FACE ( 'NONE', ( #41920 ), #26681, .F. ) ;
#12100 = ORIENTED_EDGE ( 'NONE', *, *, #39031, .T. ) ;
#12102 = CARTESIAN_POINT ( 'NONE',  ( 13.09964176094197441, 18.96253433080681106, -1.500000000000002220 ) ) ;
#12103 = CARTESIAN_POINT ( 'NONE',  ( -80.52287095715006160, -24.63287334234178871, 0.9662140553045349689 ) ) ;
#12104 = CARTESIAN_POINT ( 'NONE',  ( 19.72175082351460063, -4.362005935662174316, -1.500000000000002220 ) ) ;
#12105 = VERTEX_POINT ( 'NONE', #80964 ) ;
#12106 = CARTESIAN_POINT ( 'NONE',  ( -45.62287095715004881, -29.50249982740957577, 7.747779886224967605 ) ) ;
#12107 = CARTESIAN_POINT ( 'NONE',  ( 16.30000000000000071, 0.000000000000000000, 21.89999999999999858 ) ) ;
#12108 = CARTESIAN_POINT ( 'NONE',  ( -95.59106694108504598, -24.40034930558991633, 0.3402023900116099009 ) ) ;
#12109 = CARTESIAN_POINT ( 'NONE',  ( -123.6228709571500559, -23.47593901973091235, -1.443836447538997536 ) ) ;
#12111 = EDGE_LOOP ( 'NONE', ( #31612, #15653, #23246, #25701 ) ) ;
#12110 = CARTESIAN_POINT ( 'NONE',  ( 19.36035776617087123, -9.008237321879198234, 11.49999999999999645 ) ) ;
#12112 = DIRECTION ( 'NONE',  ( 4.476705744456278313E-16, -1.000000000000000000, 0.000000000000000000 ) ) ;
#12113 = ORIENTED_EDGE ( 'NONE', *, *, #79142, .T. ) ;
#12114 = CARTESIAN_POINT ( 'NONE',  ( 7.309977242446557888, -21.02818303981469583, 11.49999999999998934 ) ) ;
#12115 = CARTESIAN_POINT ( 'NONE',  ( 20.35908867758196550, 3.722869731652943770, 11.49999999999998934 ) ) ;
#12116 = VECTOR ( 'NONE', #98051, 1000.000000000000114 ) ;
#12117 = EDGE_LOOP ( 'NONE', ( #69412, #81162, #25936, #21205 ) ) ;
#12118 = DIRECTION ( 'NONE',  ( 0.000000000000000000, -0.5144957554275265688, 0.8574929257125440962 ) ) ;
#12119 = ORIENTED_EDGE ( 'NONE', *, *, #13693, .T. ) ;
#12120 = CARTESIAN_POINT ( 'NONE',  ( -61.62287095715004881, -24.66019654487199020, 8.947790411086131712 ) ) ;
#12121 = ORIENTED_EDGE ( 'NONE', *, *, #11803, .T. ) ;
#12122 = CARTESIAN_POINT ( 'NONE',  ( -111.6468792378191779, -25.28710546256126790, 4.332404433089555695 ) ) ;
#12123 = CARTESIAN_POINT ( 'NONE',  ( -19.40224465947428456, -7.824916089261592766, -1.500000000000002220 ) ) ;
#12125 = EDGE_CURVE ( 'NONE', #65481, #14129, #35791, .T. ) ;
#12124 = CARTESIAN_POINT ( 'NONE',  ( -19.33260374144687077, -10.33727041909969380, 11.49999999999999645 ) ) ;
#12126 = CIRCLE ( 'NONE', #15383, 129.7684398600581517 ) ;
#12127 = CARTESIAN_POINT ( 'NONE',  ( -107.6228709571500701, -23.48786465467241769, 11.44779295918253936 ) ) ;
#12128 = CARTESIAN_POINT ( 'NONE',  ( -1.797493081057526032, -22.44471576765463183, -1.500000000000002220 ) ) ;
#12129 = CARTESIAN_POINT ( 'NONE',  ( 15.04517842881462819, -14.58609674458608829, -1.500000000000002220 ) ) ;
#12130 = CARTESIAN_POINT ( 'NONE',  ( -26.27733073949819698, -24.88149021042581666, 6.353770771295153885 ) ) ;
#12131 = CARTESIAN_POINT ( 'NONE',  ( 5.671814302646631667, -5.876774720514418071, 20.58085404595000512 ) ) ;
#12132 = B_SPLINE_CURVE_WITH_KNOTS ( 'NONE', 3,
 ( #32764, #93151, #76922, #31769 ),
 .UNSPECIFIED., .F., .F.,
 ( 4, 4 ),
 ( 1.387778780781445676E-17, 0.0001000000000000028779 ),
 .UNSPECIFIED. ) ;
#12133 = CARTESIAN_POINT ( 'NONE',  ( -119.5193653822925484, -24.15620529776629510, 10.23563542870659582 ) ) ;
#12134 = CARTESIAN_POINT ( 'NONE',  ( -99.52287095715009002, -23.47593901973090524, -1.443836447538996648 ) ) ;
#12135 = VERTEX_POINT ( 'NONE', #4348 ) ;
#12136 = ORIENTED_EDGE ( 'NONE', *, *, #91149, .F. ) ;
#12137 = VERTEX_POINT ( 'NONE', #34296 ) ;
#12138 = CARTESIAN_POINT ( 'NONE',  ( -106.6228709571500559, -29.50250786944525672, 11.44777988621622988 ) ) ;
#12139 = ORIENTED_EDGE ( 'NONE', *, *, #83089, .T. ) ;
#12140 = CARTESIAN_POINT ( 'NONE',  ( 21.40653236543258231, -1.377805879665675803, -1.500000000000002220 ) ) ;
#12141 = EDGE_CURVE ( 'NONE', #73698, #39531, #78609, .T. ) ;
#12142 = CARTESIAN_POINT ( 'NONE',  ( -59.52287095715006160, -23.48783264082477018, -1.443836473390095021 ) ) ;
#12143 = ORIENTED_EDGE ( 'NONE', *, *, #11539, .F. ) ;
#12144 = CARTESIAN_POINT ( 'NONE',  ( 19.39439428382967634, -8.317090367284466268, 11.49999999999998934 ) ) ;
#12145 = LINE ( 'NONE', #6037, #19003 ) ;
#12146 = CARTESIAN_POINT ( 'NONE',  ( 2.787364042957740651, -6.376774720514424288, 21.14548745790758488 ) ) ;
#12147 = CARTESIAN_POINT ( 'NONE',  ( -50.51068615954277874, -23.85049219812685095, 10.88485053497527133 ) ) ;
#12148 = CARTESIAN_POINT ( 'NONE',  ( -80.84160375922890296, -25.30877089043013228, 4.579768006309718587 ) ) ;
#12150 = B_SPLINE_CURVE_WITH_KNOTS ( 'NONE', 3,
 ( #13013, #13511, #66342, #97266, #28253, #83023, #44483, #50104, #73439, #75407 ),
 .UNSPECIFIED., .F., .F.,
 ( 4, 2, 2, 2, 4 ),
 ( 0.000000000000000000, 0.0001573231488620521995, 0.0003146462977241043990, 0.0004719694465861565985, 0.0006292925954482087979 ),
 .UNSPECIFIED. ) ;
#12149 = CARTESIAN_POINT ( 'NONE',  ( 282.9764569301858046, 4.540774720514427543, 20.79159422840526616 ) ) ;
#12151 = CARTESIAN_POINT ( 'NONE',  ( 21.87352179494074633, -3.179377960941109915, -1.500000000000002220 ) ) ;
#12152 = ORIENTED_EDGE ( 'NONE', *, *, #56853, .F. ) ;
#12153 = B_SPLINE_CURVE_WITH_KNOTS ( 'NONE', 3,
 ( #73418, #90627, #88643, #90132 ),
 .UNSPECIFIED., .F., .F.,
 ( 4, 4 ),
 ( 0.000000000000000000, 0.002085937500000002720 ),
 .UNSPECIFIED. ) ;
#12154 = DIRECTION ( 'NONE',  ( 1.387778780781445429E-16, -1.000000000000000000, 0.000000000000000000 ) ) ;
#12155 = EDGE_CURVE ( 'NONE', #72161, #35495, #57529, .T. ) ;
#12156 = CARTESIAN_POINT ( 'NONE',  ( -3.095730855174848362, -6.376774720514413630, 20.04377961306771638 ) ) ;
#12157 = CARTESIAN_POINT ( 'NONE',  ( -78.62287095715007013, -24.66019654487199375, 8.947790411086124607 ) ) ;
#12158 = CARTESIAN_POINT ( 'NONE',  ( -28.39313913820096857, -25.15290109896971416, 6.075536601959948158 ) ) ;
#12159 = VECTOR ( 'NONE', #64647, 1000.000000000000114 ) ;
#12160 = DIRECTION ( 'NONE',  ( 0.9975640502598241977, -0.06975647374412546897, -0.000000000000000000 ) ) ;
#12161 = CARTESIAN_POINT ( 'NONE',  ( 8.224165413489119558, 19.69228431130148493, -1.500000000000002220 ) ) ;
#12162 = CARTESIAN_POINT ( 'NONE',  ( -68.98046560660316118, -25.21707011523245967, 6.550344061802529261 ) ) ;
#12163 = CARTESIAN_POINT ( 'NONE',  ( -50.91671811657901969, -25.31392319263089519, 5.203681702801226550 ) ) ;
#12164 = CARTESIAN_POINT ( 'NONE',  ( -86.58953762381671027, -24.64898659630528854, 1.056161002820827477 ) ) ;
#12165 = DIRECTION ( 'NONE',  ( -3.773278334444167608E-23, 1.000000000000000000, 0.000000000000000000 ) ) ;
#12166 = CARTESIAN_POINT ( 'NONE',  ( 16.59953334139655468, -15.42474913338910980, -1.500000000000002220 ) ) ;
#12167 = CARTESIAN_POINT ( 'NONE',  ( -85.52287095715004739, -25.00158670708909625, 2.256160236439166411 ) ) ;
#12168 = EDGE_LOOP ( 'NONE', ( #93349, #72278, #18499, #94724 ) ) ;
#12169 = CARTESIAN_POINT ( 'NONE',  ( -35.62287095715004170, -24.15516710230296482, 10.28746687063729048 ) ) ;
#12170 = DIRECTION ( 'NONE',  ( 0.000000000000000000, 0.000000000000000000, 1.000000000000000000 ) ) ;
#12171 = CARTESIAN_POINT ( 'NONE',  ( -18.32884136524465291, -7.267937366463995907, 11.49999999999999645 ) ) ;
#12172 = CARTESIAN_POINT ( 'NONE',  ( -73.62287095715005592, -23.47593901973091235, -1.443836447539006196 ) ) ;
#12173 = CARTESIAN_POINT ( 'NONE',  ( -67.62721668323153779, -24.51314013834315730, 0.6176544820404126224 ) ) ;
#12174 = ORIENTED_EDGE ( 'NONE', *, *, #24907, .F. ) ;
#12175 = CARTESIAN_POINT ( 'NONE',  ( -42.55620429048338593, -23.47593901973091235, -1.443836447539011525 ) ) ;
#12176 = CARTESIAN_POINT ( 'NONE',  ( -28.79528301136424417, -25.26026362501326972, 1.979579709026720202 ) ) ;
#12177 = CARTESIAN_POINT ( 'NONE',  ( -40.43756433397305727, -25.11033443737753501, 2.832404817301930056 ) ) ;
#12178 = CARTESIAN_POINT ( 'NONE',  ( -21.57582672592670292, -1.461774377805347802, -1.500000000000002220 ) ) ;
#12179 = DIRECTION ( 'NONE',  ( -0.06283980576413537855, 0.000000000000000000, -0.9980236263794188822 ) ) ;
#12180 = CARTESIAN_POINT ( 'NONE',  ( -70.62287095715005592, -25.00158670708909270, 2.256160236439166855 ) ) ;
#12181 = CARTESIAN_POINT ( 'NONE',  ( 282.9764569301858046, 4.540774720514427543, 20.79159422840526616 ) ) ;
#12182 = CARTESIAN_POINT ( 'NONE',  ( -71.52287095715007581, -29.50250786944525672, 11.44777988621623699 ) ) ;
#12183 = CARTESIAN_POINT ( 'NONE',  ( -3.504374479207110316, 19.46862825742285708, -1.500000000000002220 ) ) ;
#12184 = VERTEX_POINT ( 'NONE', #27680 ) ;
#12185 = CARTESIAN_POINT ( 'NONE',  ( -3.766600276044322904, -19.90762401167813067, 11.49999999999999645 ) ) ;
#12186 = CARTESIAN_POINT ( 'NONE',  ( 13.91401389203221406, 3.316774720514426456, 158.0376437107427137 ) ) ;
#12187 = B_SPLINE_CURVE_WITH_KNOTS ( 'NONE', 3,
 ( #43716, #5147, #36099, #6139, #37092, #67068, #97978, #28476, #68056, #90383, #98979, #62950 ),
 .UNSPECIFIED., .F., .F.,
 ( 4, 2, 2, 2, 2, 4 ),
 ( 0.000000000000000000, 0.0003571373273646645031, 0.0007142746547293290062, 0.001071411982093993564, 0.001249980645776326005, 0.001428549309458658663 ),
 .UNSPECIFIED. ) ;
#12188 = VECTOR ( 'NONE', #4619, 1000.000000000000227 ) ;
#12189 = CARTESIAN_POINT ( 'NONE',  ( -43.62287095715006302, -23.96177878511307568, 10.65340807706330217 ) ) ;
#12190 = VERTEX_POINT ( 'NONE', #49027 ) ;
#12191 = CARTESIAN_POINT ( 'NONE',  ( -99.61087926561188510, -25.28548745278821386, 4.301861072295783295 ) ) ;
#12192 = CARTESIAN_POINT ( 'NONE',  ( 11.95416678406013489, -5.152774720514426754, -26.25966023343078248 ) ) ;
#12193 = DIRECTION ( 'NONE',  ( 0.000000000000000000, -0.9999999999976377785, -2.173523156925979975E-06 ) ) ;
#12194 = CARTESIAN_POINT ( 'NONE',  ( 30.09341516180546350, -4.772774720514425972, -13.09311774897855862 ) ) ;
#12195 = CARTESIAN_POINT ( 'NONE',  ( -50.67452368755364489, -25.12646064496887988, 7.081740622684785436 ) ) ;
#12196 = CARTESIAN_POINT ( 'NONE',  ( 8.743921044546416610, -18.04861246754477477, -1.500000000000002220 ) ) ;
#12197 = VECTOR ( 'NONE', #95636, 1000.000000000000227 ) ;
#12198 = LINE ( 'NONE', #28424, #30513 ) ;
#12199 = ORIENTED_EDGE ( 'NONE', *, *, #71885, .T. ) ;
#12200 = AXIS2_PLACEMENT_3D ( 'NONE', #24578, #38308, #100183 ) ;
#12201 = CARTESIAN_POINT ( 'NONE',  ( -58.62287095715004881, -24.66019654487199020, 8.947790411086131712 ) ) ;
#12202 = EDGE_CURVE ( 'NONE', #59550, #64433, #14451, .T. ) ;
#12203 = DIRECTION ( 'NONE',  ( -3.773278334453079030E-23, 0.9999999999976377785, 2.173523156925979128E-06 ) ) ;
#12204 = CARTESIAN_POINT ( 'NONE',  ( -59.62287095715002749, -23.94994826722514958, -0.6494450866351729745 ) ) ;
#12205 = EDGE_CURVE ( 'NONE', #99563, #42617, #89952, .T. ) ;
#12206 = CARTESIAN_POINT ( 'NONE',  ( -105.5228709571500616, -24.99132157543084887, 2.256160258750667502 ) ) ;
#12207 = CARTESIAN_POINT ( 'NONE',  ( -89.40841769935767047, -25.12770588385219028, 7.104042889571341668 ) ) ;
#12208 = LINE ( 'NONE', #12708, #95474 ) ;
#12209 = ORIENTED_EDGE ( 'NONE', *, *, #353, .F. ) ;
#12210 = CARTESIAN_POINT ( 'NONE',  ( 8.409737122318338365, 18.51778827956368190, -1.500000000000002220 ) ) ;
#12211 = ORIENTED_EDGE ( 'NONE', *, *, #21123, .T. ) ;
#12212 = B_SPLINE_CURVE_WITH_KNOTS ( 'NONE', 3,
 ( #57868, #89297, #72086, #25895, #87288, #81181 ),
 .UNSPECIFIED., .F., .F.,
 ( 4, 2, 4 ),
 ( 0.000000000000000000, 0.001380764517854761713, 0.002761529035709523426 ),
 .UNSPECIFIED. ) ;
#12213 = EDGE_CURVE ( 'NONE', #81670, #78575, #58630, .T. ) ;
#12214 = CARTESIAN_POINT ( 'NONE',  ( -22.24355531667433539, 5.575215412481045796, 11.49999999999998934 ) ) ;
#12215 = CARTESIAN_POINT ( 'NONE',  ( 29.74624769612771402, 6.376774720514427841, 26.55905195464798396 ) ) ;
#12216 = EDGE_LOOP ( 'NONE', ( #76730, #94976, #98601, #86533 ) ) ;
#12217 = CARTESIAN_POINT ( 'NONE',  ( -109.5228709571499905, -23.73907113216990084, -1.053371485793244355 ) ) ;
#12218 = CARTESIAN_POINT ( 'NONE',  ( -76.52287095715003318, -23.94994826722565406, -0.6494450866342715845 ) ) ;
#12219 = CARTESIAN_POINT ( 'NONE',  ( -72.55620429048340725, -23.47593901973091235, -1.443836447539006196 ) ) ;
#12220 = CARTESIAN_POINT ( 'NONE',  ( 3.105769797727405024, 20.95935918496786599, 11.49999999999999645 ) ) ;
#12221 = VECTOR ( 'NONE', #25311, 1000.000000000000114 ) ;
#12222 = CARTESIAN_POINT ( 'NONE',  ( -14.74362065938029076, 16.57599527146691898, 11.49999999999998934 ) ) ;
#12223 = CARTESIAN_POINT ( 'NONE',  ( 20.58124611042576646, 0.8182449333618511123, 11.49999999999998934 ) ) ;
#12224 = EDGE_LOOP ( 'NONE', ( #62825, #31015, #26636, #83748 ) ) ;
#12225 = ORIENTED_EDGE ( 'NONE', *, *, #85862, .T. ) ;
#12226 = PLANE ( 'NONE',  #98174 ) ;
#12227 = CARTESIAN_POINT ( 'NONE',  ( -49.62287095715004881, -23.72747288104441665, -1.053458166803662444 ) ) ;
#12228 = VERTEX_POINT ( 'NONE', #57640 ) ;
#12229 = ORIENTED_EDGE ( 'NONE', *, *, #57927, .F. ) ;
#12230 = ORIENTED_EDGE ( 'NONE', *, *, #47716, .F. ) ;
#12231 = DIRECTION ( 'NONE',  ( -0.09824042138329623641, -2.980407940728110405E-17, 0.9951627101165078093 ) ) ;
#12232 = CARTESIAN_POINT ( 'NONE',  ( -28.63639164618194854, -24.19797167907964663, 9.817618374534072601 ) ) ;
#12233 = CARTESIAN_POINT ( 'NONE',  ( 15.76197349289645189, -3.603191427427929305, -28.09505689080105384 ) ) ;
#12234 = CARTESIAN_POINT ( 'NONE',  ( 16.81283763619640936, 12.23492182941471107, -1.500000000000002220 ) ) ;
#12235 = CARTESIAN_POINT ( 'NONE',  ( -21.25272785503416273, -4.502612752106283978, 11.49999999999999645 ) ) ;
#12236 = ORIENTED_EDGE ( 'NONE', *, *, #40937, .T. ) ;
#12237 = CARTESIAN_POINT ( 'NONE',  ( -113.6228709571500559, -23.48786465467241769, 11.44779295918254114 ) ) ;
#12238 = CARTESIAN_POINT ( 'NONE',  ( -115.5528692014212453, -24.52300882791528380, 0.6510814631126371488 ) ) ;
#12239 = CARTESIAN_POINT ( 'NONE',  ( -20.38924965233672282, -9.335317855073830273, -1.500000000000002220 ) ) ;
#12240 = FACE_OUTER_BOUND ( 'NONE', #13497, .T. ) ;
#12241 = CARTESIAN_POINT ( 'NONE',  ( -102.5228709571501042, -23.73934037231757443, 11.05740245334328442 ) ) ;
#12243 = ORIENTED_EDGE ( 'NONE', *, *, #47366, .T. ) ;
#12242 = ADVANCED_FACE ( 'NONE', ( #34792 ), #84445, .F. ) ;
#12244 = DIRECTION ( 'NONE',  ( 1.000000000000000000, 2.464095846557964090E-17, 0.000000000000000000 ) ) ;
#12245 = CARTESIAN_POINT ( 'NONE',  ( -116.4728709571500502, -25.40674640480650126, 5.000950440061918911 ) ) ;
#12246 = VERTEX_POINT ( 'NONE', #59633 ) ;
#12247 = ORIENTED_EDGE ( 'NONE', *, *, #91233, .T. ) ;
#12248 = CARTESIAN_POINT ( 'NONE',  ( -46.48845903137226543, -24.51419770103157347, 9.386484678747180510 ) ) ;
#12249 = EDGE_CURVE ( 'NONE', #99250, #32256, #5330, .T. ) ;
#12250 = ORIENTED_EDGE ( 'NONE', *, *, #14073, .F. ) ;
#12251 = AXIS2_PLACEMENT_3D ( 'NONE', #15959, #746, #77852 ) ;
#12252 = B_SPLINE_CURVE_WITH_KNOTS ( 'NONE', 3,
 ( #68183, #99109, #38717, #8777 ),
 .UNSPECIFIED., .F., .F.,
 ( 4, 4 ),
 ( 0.1606146910193919086, 0.1696211222915076089 ),
 .UNSPECIFIED. ) ;
#12253 = CARTESIAN_POINT ( 'NONE',  ( -18.01091527469349529, -11.40912366963296698, -1.500000000000002220 ) ) ;
#12254 = ORIENTED_EDGE ( 'NONE', *, *, #56545, .F. ) ;
#12255 = CARTESIAN_POINT ( 'NONE',  ( -88.50804541005757642, -24.34968618360933945, 0.1864209137778829184 ) ) ;
#12256 = VECTOR ( 'NONE', #6771, 1000.000000000000114 ) ;
#12257 = CARTESIAN_POINT ( 'NONE',  ( 21.44370820036873937, 4.193779532373530294, 11.49999999999998934 ) ) ;
#12258 = CYLINDRICAL_SURFACE ( 'NONE', #38416, 2.899999999999999911 ) ;
#12259 = CARTESIAN_POINT ( 'NONE',  ( 22.61316900856233403, 2.020702135111208442, 11.49999999999998934 ) ) ;
#12260 = DIRECTION ( 'NONE',  ( 0.9952638024365005887, 0.000000000000000000, 0.09721092304694053943 ) ) ;
#12261 = AXIS2_PLACEMENT_3D ( 'NONE', #77551, #83675, #6558 ) ;
#12262 = CARTESIAN_POINT ( 'NONE',  ( -81.52287095715006160, -29.50250243563736774, 8.947779886222141599 ) ) ;
#12263 = CARTESIAN_POINT ( 'NONE',  ( 19.94191871449930531, -9.063712221575384476, -1.500000000000002220 ) ) ;
#12264 = CARTESIAN_POINT ( 'NONE',  ( 7.153659783701941777, -6.376774720514422512, 20.92502190304499265 ) ) ;
#12265 = VERTEX_POINT ( 'NONE', #5829 ) ;
#12266 = CARTESIAN_POINT ( 'NONE',  ( -122.6250501111026381, -24.15620529776629510, 10.23563542870659582 ) ) ;
#12267 = CARTESIAN_POINT ( 'NONE',  ( -40.94687923781921768, -29.50249942614373921, 7.563164501610022405 ) ) ;
#12268 = VECTOR ( 'NONE', #99319, 1000.000000000000114 ) ;
#12269 = AXIS2_PLACEMENT_3D ( 'NONE', #9233, #62038, #126 ) ;
#12270 = VERTEX_POINT ( 'NONE', #76321 ) ;
#12271 = CARTESIAN_POINT ( 'NONE',  ( -41.62287095715006302, -23.48786465467240703, 11.44779295918255180 ) ) ;
#12272 = VERTEX_POINT ( 'NONE', #29164 ) ;
#12273 = CARTESIAN_POINT ( 'NONE',  ( 10.64801255963128668, 6.475225279485572472, -27.03041135669327488 ) ) ;
#12274 = CARTESIAN_POINT ( 'NONE',  ( -0.08811923664316988203, -21.90922723398732330, 0.04347934593173655160 ) ) ;
#12275 = CARTESIAN_POINT ( 'NONE',  ( 17.81766572339076404, -11.58780717566545526, -1.500000000000002220 ) ) ;
#12276 = CARTESIAN_POINT ( 'NONE',  ( -112.5505015245452540, -24.65952944569305316, 1.056160979905707675 ) ) ;
#12277 = CARTESIAN_POINT ( 'NONE',  ( -26.80230302508262241, -24.75186045690199421, 2.622372983264014135 ) ) ;
#12278 = EDGE_CURVE ( 'NONE', #29076, #73650, #85623, .T. ) ;
#12279 = FACE_OUTER_BOUND ( 'NONE', #1036, .T. ) ;
#12280 = CARTESIAN_POINT ( 'NONE',  ( -129.5228709571500758, -23.73907113216990084, -1.053371485793237916 ) ) ;
#12281 = EDGE_CURVE ( 'NONE', #33442, #1208, #36027, .T. ) ;
#12282 = LINE ( 'NONE', #43258, #19867 ) ;
#12283 = EDGE_LOOP ( 'NONE', ( #80396, #29602, #40102, #45072 ) ) ;
#12284 = CARTESIAN_POINT ( 'NONE',  ( 2.036066721924049805, 19.47704226162102614, 11.49999999999999645 ) ) ;
#12285 = DIRECTION ( 'NONE',  ( 0.000000000000000000, -0.9999999999976377785, -2.173523156925979128E-06 ) ) ;
#12286 = CARTESIAN_POINT ( 'NONE',  ( -116.5895376238167103, -23.48786465467241769, 11.44779295918253759 ) ) ;
#12287 = EDGE_LOOP ( 'NONE', ( #21414, #71161, #94809, #89869 ) ) ;
#12288 = CARTESIAN_POINT ( 'NONE',  ( 31.74473449900405697, 4.976825198871215328, -4.259190951192157293 ) ) ;
#12289 = EDGE_CURVE ( 'NONE', #30492, #50183, #22034, .T. ) ;
#12290 = CARTESIAN_POINT ( 'NONE',  ( -99.29884676835234814, -25.31439730870533111, 6.107783201820498498 ) ) ;
#12291 = DIRECTION ( 'NONE',  ( 0.000000000000000000, -3.055962005780221396E-15, -1.000000000000000000 ) ) ;
#12292 = CARTESIAN_POINT ( 'NONE',  ( -62.55620429048339304, -23.48783264082478084, -1.443836473390068820 ) ) ;
#12293 = CARTESIAN_POINT ( 'NONE',  ( 15.15379598424239838, -12.58889634127381640, 11.49999999999998934 ) ) ;
#12294 = B_SPLINE_CURVE_WITH_KNOTS ( 'NONE', 3,
 ( #3580, #96416, #10681, #57381, #27899, #26902, #19773, #10179, #57875, #88812, #19278, #41142, #81189, #35021 ),
 .UNSPECIFIED., .F., .F.,
 ( 4, 2, 2, 2, 2, 2, 4 ),
 ( 8.673617379884035472E-19, 0.0001743298406709247502, 0.0003486596813418486331, 0.0006973193626836755822, 0.001045979044025502694, 0.001220308884696416412, 0.001394638725367330565 ),
 .UNSPECIFIED. ) ;
#12295 = ORIENTED_EDGE ( 'NONE', *, *, #56022, .F. ) ;
#12296 = DIRECTION ( 'NONE',  ( -0.000000000000000000, -0.000000000000000000, -1.000000000000000000 ) ) ;
#12297 = CARTESIAN_POINT ( 'NONE',  ( 30.59431191903084013, -4.508530027678929741, 26.46517314890041916 ) ) ;
#12298 = PERSON_AND_ORGANIZATION ( #70597, #27821 ) ;
#12299 = ORIENTED_EDGE ( 'NONE', *, *, #95504, .T. ) ;
#12300 = CARTESIAN_POINT ( 'NONE',  ( 9.058420110819380255, -0.8999999999999999112, 3.692441080025382405 ) ) ;
#12301 = CARTESIAN_POINT ( 'NONE',  ( -101.6228709571500559, -24.65952944569304606, 1.056160979905702790 ) ) ;
#12302 = CARTESIAN_POINT ( 'NONE',  ( -47.48417913239472909, -24.65952944569304606, 1.056160979905696129 ) ) ;
#12303 = CARTESIAN_POINT ( 'NONE',  ( -118.5167440879351375, -24.65952944569305316, 1.056160979905708119 ) ) ;
#12304 = CARTESIAN_POINT ( 'NONE',  ( -7.264088518202086675, -6.376774720514411854, 19.78976258633487717 ) ) ;
#12305 = DIRECTION ( 'NONE',  ( 7.994117400814786717E-16, 0.000000000000000000, -1.000000000000000000 ) ) ;
#12306 = EDGE_CURVE ( 'NONE', #33323, #83635, #39677, .T. ) ;
#12307 = CARTESIAN_POINT ( 'NONE',  ( -73.52287095715007581, -24.64898659630528854, 1.056161002820824368 ) ) ;
#12309 = EDGE_CURVE ( 'NONE', #12874, #84227, #37293, .T. ) ;
#12308 = CARTESIAN_POINT ( 'NONE',  ( 18.80405327530603543, -6.659971710459020144, 11.49999999999998934 ) ) ;
#12310 = DIRECTION ( 'NONE',  ( 0.000000000000000000, 0.000000000000000000, -1.000000000000000000 ) ) ;
#12311 = CARTESIAN_POINT ( 'NONE',  ( -0.06713937605066598591, -22.18082801617931921, 0.4473269341374352392 ) ) ;
#12312 = ORIENTED_EDGE ( 'NONE', *, *, #49112, .T. ) ;
#12313 = CARTESIAN_POINT ( 'NONE',  ( -128.5895376238167103, -23.48786465467242479, 11.44779295918253403 ) ) ;
#12314 = CARTESIAN_POINT ( 'NONE',  ( 9.492487079130338401, -5.851656861456516978, -26.75003832473357690 ) ) ;
#12315 = VECTOR ( 'NONE', #92675, 1000.000000000000000 ) ;
#12316 = B_SPLINE_CURVE_WITH_KNOTS ( 'NONE', 3,
 ( #96531, #51865, #35144, #66115, #89424, #42764 ),
 .UNSPECIFIED., .F., .F.,
 ( 4, 2, 4 ),
 ( 0.000000000000000000, 0.001380901958385382256, 0.002761803916770764512 ),
 .UNSPECIFIED. ) ;
#12317 = DIRECTION ( 'NONE',  ( 1.000000000000000000, 0.000000000000000000, 0.000000000000000000 ) ) ;
#12318 = CARTESIAN_POINT ( 'NONE',  ( 6.783277368979140576, -6.376774720515435924, -28.31678455572487252 ) ) ;
#12319 = CARTESIAN_POINT ( 'NONE',  ( 8.676776695296462449, 18.57322330470351091, 2.100000000000000089 ) ) ;
#12320 = DIRECTION ( 'NONE',  ( 0.000000000000000000, 0.9967269304714136968, 0.08084198211964954695 ) ) ;
#12321 = EDGE_CURVE ( 'NONE', #86027, #94971, #85095, .T. ) ;
#12322 = CARTESIAN_POINT ( 'NONE',  ( -28.98875734969026041, -5.965225279485572685, 26.43402280011862615 ) ) ;
#12323 = DIRECTION ( 'NONE',  ( 0.000000000000000000, 0.000000000000000000, -1.000000000000000000 ) ) ;
#12324 = VECTOR ( 'NONE', #69759, 1000.000000000000000 ) ;
#12325 = ORIENTED_EDGE ( 'NONE', *, *, #49711, .F. ) ;
#12326 = CARTESIAN_POINT ( 'NONE',  ( -64.62287095715008434, -23.96127896941632329, -0.6493128931037873697 ) ) ;
#12327 = ADVANCED_FACE ( 'NONE', ( #51518 ), #39284, .T. ) ;
#12328 = CARTESIAN_POINT ( 'NONE',  ( 6.420673076923079314, -6.376774720514427841, 21.83974358974358765 ) ) ;
#12329 = ORIENTED_EDGE ( 'NONE', *, *, #25961, .F. ) ;
#12330 = VECTOR ( 'NONE', #56630, 1000.000000000000000 ) ;
#12331 = CARTESIAN_POINT ( 'NONE',  ( 19.68333694646799614, 4.735253856516091098, -1.500000000000002220 ) ) ;
#12332 = B_SPLINE_CURVE_WITH_KNOTS ( 'NONE', 3,
 ( #86855, #86365, #16849, #17351, #58433, #34588 ),
 .UNSPECIFIED., .F., .F.,
 ( 4, 2, 4 ),
 ( 0.000000000000000000, 0.001380764517854760629, 0.002761529035709521258 ),
 .UNSPECIFIED. ) ;
#12333 = CARTESIAN_POINT ( 'NONE',  ( -122.5921601752248904, -23.48783264082477373, -1.443836473390087471 ) ) ;
#12334 = EDGE_CURVE ( 'NONE', #20807, #89693, #64055, .T. ) ;
#12335 = VECTOR ( 'NONE', #54368, 1000.000000000000000 ) ;
#12336 = DIRECTION ( 'NONE',  ( 0.9888510809027408754, 5.365801633547220192E-16, 0.1489078231574191280 ) ) ;
#12337 = VECTOR ( 'NONE', #82350, 1000.000000000000000 ) ;
#12338 = EDGE_CURVE ( 'NONE', #35233, #33585, #80778, .T. ) ;
#12339 = CYLINDRICAL_SURFACE ( 'NONE', #71988, 21.89999999999999858 ) ;
#12340 = ORIENTED_EDGE ( 'NONE', *, *, #89017, .T. ) ;
#12341 = CARTESIAN_POINT ( 'NONE',  ( -46.62287095715006302, -23.95044443724992433, 10.65354141964650125 ) ) ;
#12342 = CARTESIAN_POINT ( 'NONE',  ( -52.52287095715006870, -23.96177878511308634, 10.65340807706330573 ) ) ;
#12343 = CARTESIAN_POINT ( 'NONE',  ( -14.05898297266747221, -14.31596314050798568, -1.500000000000002220 ) ) ;
#12344 = CARTESIAN_POINT ( 'NONE',  ( -11.20027426441765961, 17.80179601997297212, 11.49999999999999645 ) ) ;
#12345 = DIRECTION ( 'NONE',  ( -3.773278334453080206E-23, 0.9999999999976377785, 2.173523156925979975E-06 ) ) ;
#12346 = CARTESIAN_POINT ( 'NONE',  ( -70.53857251337137768, -24.73531770709095312, 8.716586749053510275 ) ) ;
#12347 = CARTESIAN_POINT ( 'NONE',  ( -9.261969182712835646, 20.05037652441878038, 11.49999999999998934 ) ) ;
#12348 = CARTESIAN_POINT ( 'NONE',  ( -40.41683116089613748, -25.31589329912315378, 5.082404370520299253 ) ) ;
#12349 = CARTESIAN_POINT ( 'NONE',  ( -2.499999999999986677, 22.00000000000000000, 2.100000000000000089 ) ) ;
#12350 = DIRECTION ( 'NONE',  ( 3.773278334444167608E-23, -1.000000000000000000, 0.000000000000000000 ) ) ;
#12351 = ORIENTED_EDGE ( 'NONE', *, *, #42597, .F. ) ;
#12352 = CARTESIAN_POINT ( 'NONE',  ( -89.40841769935764205, -25.12049752546738191, 2.832404795212221327 ) ) ;
#12353 = CARTESIAN_POINT ( 'NONE',  ( -31.64312605532579425, -24.15543982623907127, -0.2315651400026576545 ) ) ;
#12354 = ORIENTED_EDGE ( 'NONE', *, *, #88534, .T. ) ;
#12355 = ORIENTED_EDGE ( 'NONE', *, *, #23512, .F. ) ;
#12356 = CARTESIAN_POINT ( 'NONE',  ( -6.499999999999992895, 3.851859888774471706E-31, 4.499999999999999112 ) ) ;
#12357 = CARTESIAN_POINT ( 'NONE',  ( 10.95759398273795249, -4.132774720514426292, -26.86884997114579932 ) ) ;
#12358 = CARTESIAN_POINT ( 'NONE',  ( -76.59623109255625195, -23.96119346886880663, -0.6495511937832059157 ) ) ;
#12359 = CARTESIAN_POINT ( 'NONE',  ( 10.54205562766345672, -17.70522803435136083, -1.500000000000002220 ) ) ;
#12360 = CARTESIAN_POINT ( 'NONE',  ( 19.98928912078053699, -8.061568661392884749, 11.49999999999999645 ) ) ;
#12361 = ORIENTED_EDGE ( 'NONE', *, *, #71364, .F. ) ;
#12362 = FACE_OUTER_BOUND ( 'NONE', #20979, .T. ) ;
#12363 = PLANE ( 'NONE',  #70945 ) ;
#12364 = AXIS2_PLACEMENT_3D ( 'NONE', #76422, #43994, #45009 ) ;
#12365 = DIRECTION ( 'NONE',  ( -2.216313064514630605E-15, -0.000000000000000000, -1.000000000000000000 ) ) ;
#12366 = CARTESIAN_POINT ( 'NONE',  ( 7.974090105135403839, 20.87195307945309963, -1.500000000000002220 ) ) ;
#12367 = CARTESIAN_POINT ( 'NONE',  ( -59.62287095715002749, -23.96177878511307568, 10.65340807706330573 ) ) ;
#12368 = CARTESIAN_POINT ( 'NONE',  ( -65.62287095715005592, -29.50249982740957577, 7.747779886224967605 ) ) ;
#12369 = VERTEX_POINT ( 'NONE', #16422 ) ;
#12370 = CYLINDRICAL_SURFACE ( 'NONE', #61511, 251.9358649670780892 ) ;
#12371 = DIRECTION ( 'NONE',  ( -1.387778780781446464E-15, 0.000000000000000000, -1.000000000000000000 ) ) ;
#12372 = CARTESIAN_POINT ( 'NONE',  ( -7.158894406585330827, 19.61798520005962487, -1.500000000000002220 ) ) ;
#12373 = ORIENTED_EDGE ( 'NONE', *, *, #40303, .T. ) ;
#12374 = B_SPLINE_CURVE_WITH_KNOTS ( 'NONE', 3,
 ( #14531, #35013, #60732, #73085 ),
 .UNSPECIFIED., .F., .F.,
 ( 4, 4 ),
 ( 0.000000000000000000, 9.999999999998897304E-05 ),
 .UNSPECIFIED. ) ;
#12376 = ORIENTED_EDGE ( 'NONE', *, *, #8881, .F. ) ;
#12375 = CARTESIAN_POINT ( 'NONE',  ( -86.64361993685139396, -23.48783264082478084, -1.443836473390066155 ) ) ;
#12377 = B_SPLINE_CURVE_WITH_KNOTS ( 'NONE', 3,
 ( #65345, #51588, #11025, #82522, #36358, #96263 ),
 .UNSPECIFIED., .F., .F.,
 ( 4, 2, 4 ),
 ( 1.570755371633954459E-05, 0.001396183895866087319, 0.002776660238015835145 ),
 .UNSPECIFIED. ) ;
#12378 = ORIENTED_EDGE ( 'NONE', *, *, #18038, .T. ) ;
#12379 = ADVANCED_FACE ( 'NONE', ( #39764 ), #78171, .T. ) ;
#12380 = CARTESIAN_POINT ( 'NONE',  ( -100.5461013931486605, -24.83644354573578994, 8.397322867130101898 ) ) ;
#12381 = CARTESIAN_POINT ( 'NONE',  ( 16.98782256641479904, -12.52229676876588371, -1.500000000000002220 ) ) ;
#12382 = ADVANCED_FACE ( 'NONE', ( #92553 ), #52197, .T. ) ;
#12383 = ORIENTED_EDGE ( 'NONE', *, *, #34432, .T. ) ;
#12384 = CARTESIAN_POINT ( 'NONE',  ( -37.62287095715007013, -23.47596703998600276, 11.44779298504227505 ) ) ;
#12385 = CARTESIAN_POINT ( 'NONE',  ( -48.89837313299270960, -25.27432442679760527, 5.876172143706702933 ) ) ;
#12386 = CARTESIAN_POINT ( 'NONE',  ( -48.62287095715004881, -23.48786465467241058, 11.44779295918254824 ) ) ;
#12387 = CARTESIAN_POINT ( 'NONE',  ( -76.58156790035729955, -24.66019654487199375, 8.947790411086119278 ) ) ;
#12388 = CARTESIAN_POINT ( 'NONE',  ( -49.11396232410867668, -25.24991201570810162, 3.837753354500891501 ) ) ;
#12389 = CARTESIAN_POINT ( 'NONE',  ( 20.36105213711617878, 7.643125777291208678, -1.500000000000002220 ) ) ;
#12390 = CARTESIAN_POINT ( 'NONE',  ( -20.27875734969026311, 3.456774720514426136, 24.00402280011862288 ) ) ;
#12392 = ORIENTED_EDGE ( 'NONE', *, *, #28413, .F. ) ;
#12391 = CARTESIAN_POINT ( 'NONE',  ( -17.05807961832342912, 14.25954964135033265, 11.49999999999999645 ) ) ;
#12393 = CARTESIAN_POINT ( 'NONE',  ( -45.62287095715004170, -24.15431212366391023, -0.2830839119429199857 ) ) ;
#12394 = CARTESIAN_POINT ( 'NONE',  ( 7.165897526731081157, -6.376774720514420736, 20.76279523443833597 ) ) ;
#12395 = CARTESIAN_POINT ( 'NONE',  ( -24.90875734969025501, 6.475225279485573360, 26.43402280011862615 ) ) ;
#12396 = ORIENTED_EDGE ( 'NONE', *, *, #85282, .F. ) ;
#12398 = ORIENTED_EDGE ( 'NONE', *, *, #47366, .F. ) ;
#12397 = CARTESIAN_POINT ( 'NONE',  ( 30.53060340732036337, 1.477225279485574028, 3.744237563515920634E-15 ) ) ;
#12399 = ORIENTED_EDGE ( 'NONE', *, *, #77694, .T. ) ;
#12400 = CARTESIAN_POINT ( 'NONE',  ( 3.675000000000002487, 14.49999999999999822, 24.00000000000000000 ) ) ;
#12401 = CARTESIAN_POINT ( 'NONE',  ( -49.62287095715005592, -24.65952944569304250, 1.056160979905693020 ) ) ;
#12402 = CARTESIAN_POINT ( 'NONE',  ( -49.41588265436393357, -25.31237105244463237, 4.715953302175392103 ) ) ;
#12403 = EDGE_CURVE ( 'NONE', #82488, #16105, #41279, .T. ) ;
#12404 = CARTESIAN_POINT ( 'NONE',  ( -87.52287095715006160, -23.47596703998600631, 11.44779298504228393 ) ) ;
#12405 = CARTESIAN_POINT ( 'NONE',  ( -121.5228709571500616, -29.50250786944525672, 11.44777988621622811 ) ) ;
#12406 = VERTEX_POINT ( 'NONE', #34669 ) ;
#12407 = AXIS2_PLACEMENT_3D ( 'NONE', #67300, #91120, #37348 ) ;
#12408 = CARTESIAN_POINT ( 'NONE',  ( 16.99290379607386114, -9.356058476803225332, 11.49999999999999645 ) ) ;
#12409 = CARTESIAN_POINT ( 'NONE',  ( -115.5228709571501327, -24.92604778743018556, 8.074972756849357225 ) ) ;
#12410 = VECTOR ( 'NONE', #2660, 1000.000000000000114 ) ;
#12411 = EDGE_CURVE ( 'NONE', #99951, #68864, #27583, .T. ) ;
#12412 = VERTEX_POINT ( 'NONE', #11328 ) ;
#12413 = CARTESIAN_POINT ( 'NONE',  ( 21.57151214508649772, 3.625915217019311583E-15, -1.700000000000000178 ) ) ;
#12414 = LINE ( 'NONE', #36266, #50640 ) ;
#12415 = EDGE_CURVE ( 'NONE', #71483, #96695, #56725, .T. ) ;
#12416 = EDGE_CURVE ( 'NONE', #61919, #35496, #73234, .T. ) ;
#12417 = DIRECTION ( 'NONE',  ( -0.3133898629642186684, 0.000000000000000000, 0.9496245541219267006 ) ) ;
#12418 = VECTOR ( 'NONE', #28188, 1000.000000000000000 ) ;
#12419 = EDGE_CURVE ( 'NONE', #18110, #62581, #90469, .T. ) ;
#12420 = LINE ( 'NONE', #60117, #22847 ) ;
#12421 = CARTESIAN_POINT ( 'NONE',  ( 9.507684299284662188, -17.14340340408069707, -1.500000000000002220 ) ) ;
#12422 = CARTESIAN_POINT ( 'NONE',  ( -91.15361000704896810, -25.27880950044357178, 5.947789066507965572 ) ) ;
#12424 = EDGE_CURVE ( 'NONE', #44696, #36479, #19432, .T. ) ;
#12423 = ORIENTED_EDGE ( 'NONE', *, *, #94859, .F. ) ;
#12425 = B_SPLINE_CURVE_WITH_KNOTS ( 'NONE', 3,
 ( #2082, #63489, #63995, #78662 ),
 .UNSPECIFIED., .F., .F.,
 ( 4, 4 ),
 ( 0.000000000000000000, 9.999999999998897304E-05 ),
 .UNSPECIFIED. ) ;
#12426 = CARTESIAN_POINT ( 'NONE',  ( -19.98823316618875268, 7.996883007359760320, -1.500000000000002220 ) ) ;
#12427 = CYLINDRICAL_SURFACE ( 'NONE', #65835, 1.500000000000001332 ) ;
#12428 = CARTESIAN_POINT ( 'NONE',  ( -80.43221577628075636, -25.30394759211435485, 4.967019781099680564 ) ) ;
#12429 = CARTESIAN_POINT ( 'NONE',  ( -50.52287095715006160, -23.84047902841603772, -0.8780736468305390119 ) ) ;
#12430 = CARTESIAN_POINT ( 'NONE',  ( -100.1584806888234738, -25.27473227769451114, 3.322325759095222431 ) ) ;
#12431 = CARTESIAN_POINT ( 'NONE',  ( 9.898807498884217182, 20.75630955806377287, -1.500000000000002220 ) ) ;
#12432 = PERSON_AND_ORGANIZATION ( #70597, #27821 ) ;
#12433 = DIRECTION ( 'NONE',  ( 1.000000000000000000, 3.773278334444167608E-23, 8.201307833595939069E-29 ) ) ;
#12434 = CARTESIAN_POINT ( 'NONE',  ( -53.63875608333281519, -24.15543982623906771, -0.2315651400026670359 ) ) ;
#12435 = CARTESIAN_POINT ( 'NONE',  ( -19.70923665959843873, 4.302044407003456250, 11.49999999999999645 ) ) ;
#12436 = CARTESIAN_POINT ( 'NONE',  ( -109.5317876555421037, -25.28814117369136838, 3.055434580949142553 ) ) ;
#12437 = CARTESIAN_POINT ( 'NONE',  ( -32.60153139752230089, -23.96169478059712787, 10.65365249895719124 ) ) ;
#12438 = CARTESIAN_POINT ( 'NONE',  ( -46.52287095715006160, -24.65952944569304606, 1.056160979905693686 ) ) ;
#12439 = PLANE ( 'NONE',  #55340 ) ;
#12440 = CARTESIAN_POINT ( 'NONE',  ( -82.52287095715007581, -23.72773821059537269, 11.05748984161097503 ) ) ;
#12441 = EDGE_CURVE ( 'NONE', #80312, #3302, #80335, .T. ) ;
#12443 = EDGE_CURVE ( 'NONE', #2424, #70415, #66140, .T. ) ;
#12442 = CARTESIAN_POINT ( 'NONE',  ( -18.60049703728633474, -6.982253431394513932, 11.49999999999998934 ) ) ;
#12444 = FACE_OUTER_BOUND ( 'NONE', #82303, .T. ) ;
#12445 = CARTESIAN_POINT ( 'NONE',  ( -6.535591236171724105, 18.61618873491671877, -1.500000000000002220 ) ) ;
#12446 = VECTOR ( 'NONE', #64582, 1000.000000000000000 ) ;
#12447 = DIRECTION ( 'NONE',  ( 0.9978940991575084851, 0.000000000000000000, 0.06486421869277853025 ) ) ;
#12448 = CARTESIAN_POINT ( 'NONE',  ( -110.5228709571500616, -24.99156044556120548, 7.747789690856173195 ) ) ;
#12449 = CARTESIAN_POINT ( 'NONE',  ( 1.949999999999999956, -0.1925000000000001155, -0.1925000000000000600 ) ) ;
#12450 = CARTESIAN_POINT ( 'NONE',  ( -3.087264924507187924, 20.40197043678811539, 11.49999999999999645 ) ) ;
#12451 = AXIS2_PLACEMENT_3D ( 'NONE', #79678, #41638, #40125 ) ;
#12452 = CARTESIAN_POINT ( 'NONE',  ( -75.52287095715007581, -23.47596703998600631, 11.44779298504228571 ) ) ;
#12453 = EDGE_CURVE ( 'NONE', #40720, #17533, #8910, .T. ) ;
#12454 = CARTESIAN_POINT ( 'NONE',  ( 31.71875899258513698, 3.424184405370887863, -3.672337713816452354 ) ) ;
#12455 = CARTESIAN_POINT ( 'NONE',  ( -20.48750165597241590, 9.616757810196778777, 11.49999999999999645 ) ) ;
#12456 = B_SPLINE_CURVE_WITH_KNOTS ( 'NONE', 3,
 ( #29236, #13503, #97752, #20128 ),
 .UNSPECIFIED., .F., .F.,
 ( 4, 4 ),
 ( 0.9004288987138345801, 0.9094353299859498918 ),
 .UNSPECIFIED. ) ;
#12457 = ORIENTED_EDGE ( 'NONE', *, *, #22244, .T. ) ;
#12458 = CARTESIAN_POINT ( 'NONE',  ( -10.75273025779354263, -5.876774720514426953, 16.96478738960562893 ) ) ;
#12459 = ADVANCED_FACE ( 'NONE', ( #79828 ), #34171, .T. ) ;
#12460 = CARTESIAN_POINT ( 'NONE',  ( 30.58729439590573662, 5.356774720514427379, 26.14186284044631492 ) ) ;
#12461 = CARTESIAN_POINT ( 'NONE',  ( -60.52287095715006160, -23.47593901973090169, -1.443836447538996870 ) ) ;
#12462 = ADVANCED_FACE ( 'NONE', ( #57520 ), #88456, .T. ) ;
#12463 = CARTESIAN_POINT ( 'NONE',  ( -2.220741593810419801, -6.376774720514411854, 19.46247113826587238 ) ) ;
#12464 = ORIENTED_EDGE ( 'NONE', *, *, #66279, .F. ) ;
#12465 = VECTOR ( 'NONE', #70062, 1000.000000000000114 ) ;
#12466 = EDGE_CURVE ( 'NONE', #86336, #19038, #50895, .T. ) ;
#12467 = VERTEX_POINT ( 'NONE', #33157 ) ;
#12468 = CARTESIAN_POINT ( 'NONE',  ( -65.05438548721849656, -5.356774720514425603, 24.50402280011859091 ) ) ;
#12469 = CARTESIAN_POINT ( 'NONE',  ( 15.09361930729867574, -17.17024899132524496, 11.49999999999998934 ) ) ;
#12471 = EDGE_CURVE ( 'NONE', #75788, #90630, #64142, .T. ) ;
#12470 = CARTESIAN_POINT ( 'NONE',  ( -29.61080365403367054, -23.65836453306689080, -1.055554856561816246 ) ) ;
#12472 = CARTESIAN_POINT ( 'NONE',  ( 4.073501596442082651, -21.17334570714589859, -1.500000000000002220 ) ) ;
#12473 = CARTESIAN_POINT ( 'NONE',  ( -113.5932527405990555, -23.73791477778912196, 11.05961554403170233 ) ) ;
#12474 = CARTESIAN_POINT ( 'NONE',  ( -80.48900664166535535, -29.50249842297920466, 7.101626040072651413 ) ) ;
#12475 = CARTESIAN_POINT ( 'NONE',  ( 1.861690257272737847, 22.46465895387273903, 11.49999999999999645 ) ) ;
#12476 = ORIENTED_EDGE ( 'NONE', *, *, #72802, .T. ) ;
#12477 = CARTESIAN_POINT ( 'NONE',  ( -69.75794024142732042, -25.24754266353784260, 4.946031669615599036 ) ) ;
#12478 = CARTESIAN_POINT ( 'NONE',  ( 10.07166557822571207, 19.55152498600455857, 11.49999999999998934 ) ) ;
#12479 = AXIS2_PLACEMENT_3D ( 'NONE', #100177, #70762, #54536 ) ;
#12480 = FACE_OUTER_BOUND ( 'NONE', #99720, .T. ) ;
#12481 = CARTESIAN_POINT ( 'NONE',  ( -62.62287095715004881, -29.50250243563736774, 8.947779886222145151 ) ) ;
#12482 = ORIENTED_EDGE ( 'NONE', *, *, #70155, .F. ) ;
#12483 = EDGE_CURVE ( 'NONE', #39449, #79246, #26046, .T. ) ;
#12484 = DIRECTION ( 'NONE',  ( 0.000000000000000000, 1.000000000000000000, -0.000000000000000000 ) ) ;
#12485 = CARTESIAN_POINT ( 'NONE',  ( -111.6228709571500701, -24.50216790748098461, 0.6166512839513800248 ) ) ;
#12486 = ORIENTED_EDGE ( 'NONE', *, *, #80614, .T. ) ;
#12487 = VECTOR ( 'NONE', #61562, 1000.000000000000000 ) ;
#12488 = DIRECTION ( 'NONE',  ( -3.773278334453079618E-23, 0.9999999999976377785, 2.173523156925979975E-06 ) ) ;
#12489 = ORIENTED_EDGE ( 'NONE', *, *, #21802, .T. ) ;
#12490 = VECTOR ( 'NONE', #48607, 1000.000000000000000 ) ;
#12491 = EDGE_LOOP ( 'NONE', ( #56082, #68905, #493, #34662 ) ) ;
#12492 = CARTESIAN_POINT ( 'NONE',  ( -126.5228709571500332, -23.72747288104470442, -1.053458166803224572 ) ) ;
#12493 = DIRECTION ( 'NONE',  ( -0.000000000000000000, -0.000000000000000000, -1.000000000000000000 ) ) ;
#12494 = CARTESIAN_POINT ( 'NONE',  ( -57.49291429130692421, -24.51314013834315375, 0.6176544820404114011 ) ) ;
#12495 = CARTESIAN_POINT ( 'NONE',  ( -18.43012528856881715, -8.789534013050598560, -1.500000000000002220 ) ) ;
#12496 = ORIENTED_EDGE ( 'NONE', *, *, #87032, .T. ) ;
#12497 = DIRECTION ( 'NONE',  ( -0.000000000000000000, -1.000000000000000000, -0.000000000000000000 ) ) ;
#12498 = CARTESIAN_POINT ( 'NONE',  ( -115.6228709571500701, -24.91570333823100469, 8.075032458375558164 ) ) ;
#12499 = CARTESIAN_POINT ( 'NONE',  ( -105.6242956764457972, -24.92564183028979130, 1.928384488918251316 ) ) ;
#12500 = CARTESIAN_POINT ( 'NONE',  ( -71.70602904702231228, -25.03149565143765543, 6.253518850926207406 ) ) ;
#12501 = VERTEX_POINT ( 'NONE', #44777 ) ;
#12502 = CARTESIAN_POINT ( 'NONE',  ( -50.22287095715005734, -23.47596703998600276, 11.44779298504227860 ) ) ;
#12503 = CARTESIAN_POINT ( 'NONE',  ( -27.70544111104076990, -24.63646064706438565, 8.251826737477770735 ) ) ;
#12504 = ORIENTED_EDGE ( 'NONE', *, *, #59655, .F. ) ;
#12505 = CARTESIAN_POINT ( 'NONE',  ( 14.06386034339543478, -15.33156129944631729, -1.500000000000002220 ) ) ;
#12506 = EDGE_LOOP ( 'NONE', ( #96885, #89803, #65821, #75291 ) ) ;
#12508 = ORIENTED_EDGE ( 'NONE', *, *, #48536, .F. ) ;
#12507 = CARTESIAN_POINT ( 'NONE',  ( -40.11295564403756231, -25.30551896248393007, 5.047575478646234792 ) ) ;
#12509 = CARTESIAN_POINT ( 'NONE',  ( -28.62287095715004526, -24.34983653798460779, 9.387659975667750345 ) ) ;
#12510 = CARTESIAN_POINT ( 'NONE',  ( -123.6228709571500559, -29.50247984919015209, -1.443849546365046699 ) ) ;
#12511 = EDGE_LOOP ( 'NONE', ( #54848, #55714, #77034, #100314 ) ) ;
#12512 = VERTEX_POINT ( 'NONE', #51894 ) ;
#12513 = CARTESIAN_POINT ( 'NONE',  ( -114.6228709571500417, -24.65952944569305316, 1.056160979905703234 ) ) ;
#12514 = CARTESIAN_POINT ( 'NONE',  ( -64.52287095715006160, -23.48786465467241769, 11.44779295918254824 ) ) ;
#12515 = CARTESIAN_POINT ( 'NONE',  ( -19.77875734969026311, 6.143225279485574397, 29.49402280011862487 ) ) ;
#12516 = CARTESIAN_POINT ( 'NONE',  ( -71.20303962927951602, -25.31201693143477627, 5.785489938579095437 ) ) ;
#12518 = EDGE_LOOP ( 'NONE', ( #70452, #18269, #10542, #39446 ) ) ;
#12517 = CARTESIAN_POINT ( 'NONE',  ( -5.561696574893697509, -21.35426480686918538, 11.49999999999999645 ) ) ;
#12519 = DIRECTION ( 'NONE',  ( 0.000000000000000000, -0.9999999999976377785, -2.173523156925979128E-06 ) ) ;
#12520 = CARTESIAN_POINT ( 'NONE',  ( 16.66146196086182130, -15.28366505690825328, -1.500000000000002220 ) ) ;
#12521 = AXIS2_PLACEMENT_3D ( 'NONE', #15007, #20241, #45974 ) ;
#12523 = ORIENTED_EDGE ( 'NONE', *, *, #16995, .T. ) ;
#12522 = CARTESIAN_POINT ( 'NONE',  ( -115.5168655184217243, -24.40133493613050675, 9.663955038902797057 ) ) ;
#12524 = ORIENTED_EDGE ( 'NONE', *, *, #45378, .T. ) ;
#12525 = CIRCLE ( 'NONE', #59535, 2.899999999999999467 ) ;
#12526 = CARTESIAN_POINT ( 'NONE',  ( -8.160000000000000142, -10.65233964170348635, 1.628518864987183790 ) ) ;
#12527 = EDGE_CURVE ( 'NONE', #85754, #52727, #22704, .T. ) ;
#12528 = CARTESIAN_POINT ( 'NONE',  ( -57.54802801865898232, -24.15620529776628089, 10.23563542870660470 ) ) ;
#12529 = VERTEX_POINT ( 'NONE', #20413 ) ;
#12530 = CARTESIAN_POINT ( 'NONE',  ( -21.05374637409849825, 2.266213160971460194, 11.49999999999998934 ) ) ;
#12531 = EDGE_CURVE ( 'NONE', #49615, #84685, #66640, .T. ) ;
#12532 = CARTESIAN_POINT ( 'NONE',  ( -65.62287095715005592, -23.48783264082478084, -1.443836473390067265 ) ) ;
#12533 = CARTESIAN_POINT ( 'NONE',  ( -20.07822104958740539, -9.643837532803976487, -1.500000000000002220 ) ) ;
#12534 = CARTESIAN_POINT ( 'NONE',  ( 29.57907552799942863, 6.376774720514426953, 29.21818156447040948 ) ) ;
#12535 = EDGE_CURVE ( 'NONE', #10502, #47563, #28846, .T. ) ;
#12536 = ORIENTED_EDGE ( 'NONE', *, *, #42355, .F. ) ;
#12537 = PLANE ( 'NONE',  #1178 ) ;
#12538 = CARTESIAN_POINT ( 'NONE',  ( -48.62287095715004881, -24.65952944569303895, 1.056160979905692798 ) ) ;
#12539 = EDGE_CURVE ( 'NONE', #29076, #92355, #83321, .T. ) ;
#12540 = AXIS2_PLACEMENT_3D ( 'NONE', #91652, #16023, #100242 ) ;
#12541 = EDGE_CURVE ( 'NONE', #40108, #39879, #73600, .T. ) ;
#12542 = CARTESIAN_POINT ( 'NONE',  ( -49.62287095715007013, -23.95044443724992078, 10.65354141964650125 ) ) ;
#12543 = PLANE ( 'NONE',  #80973 ) ;
#12544 = CARTESIAN_POINT ( 'NONE',  ( 10.93668938013857783, -16.14717738681254033, -1.500000000000002220 ) ) ;
#12545 = EDGE_CURVE ( 'NONE', #35590, #8339, #7300, .T. ) ;
#12546 = CARTESIAN_POINT ( 'NONE',  ( -11.90495014755217618, 17.82271480561356469, -1.500000000000002220 ) ) ;
#12547 = CARTESIAN_POINT ( 'NONE',  ( -26.36451126669314604, -24.57999616917673080, 2.180457946598438834 ) ) ;
#12548 = CYLINDRICAL_SURFACE ( 'NONE', #58414, 1.399999999999998579 ) ;
#12549 = DIRECTION ( 'NONE',  ( -3.773278334444167608E-23, 1.000000000000000000, 0.000000000000000000 ) ) ;
#12550 = CARTESIAN_POINT ( 'NONE',  ( 0.8422786845129024424, 22.77647355728978340, -1.500000000000002220 ) ) ;
#12551 = AXIS2_PLACEMENT_3D ( 'NONE', #94230, #9501, #40462 ) ;
#12552 = ADVANCED_BREP_SHAPE_REPRESENTATION ( '', ( #8170, #37391 ), #27759 ) ;
#12553 = APPROVAL_DATE_TIME ( #67354, #21550 ) ;
#12554 = CARTESIAN_POINT ( 'NONE',  ( -106.5970399906172474, -23.48786465467241769, 11.44779295918253581 ) ) ;
#12555 = LINE ( 'NONE', #88696, #55729 ) ;
#12556 = CARTESIAN_POINT ( 'NONE',  ( 19.57267778704439820, -3.578973306870405047, 11.49999999999999645 ) ) ;
#12557 = CARTESIAN_POINT ( 'NONE',  ( -104.5908932905232120, -24.15543982623907482, -0.2315651400026580709 ) ) ;
#12558 = VECTOR ( 'NONE', #58837, 1000.000000000000000 ) ;
#12559 = CARTESIAN_POINT ( 'NONE',  ( 7.166666666666668739, -6.376774720514414518, 20.78665865384614975 ) ) ;
#12560 = CARTESIAN_POINT ( 'NONE',  ( -101.6228709571500559, -24.64898659630368627, 1.056161002820829697 ) ) ;
#12561 = ORIENTED_EDGE ( 'NONE', *, *, #20331, .F. ) ;
#12562 = CARTESIAN_POINT ( 'NONE',  ( -25.78461022856923890, -24.79966393088477972, 3.119017264803729983 ) ) ;
#12563 = EDGE_CURVE ( 'NONE', #45115, #92012, #21410, .T. ) ;
#12564 = CARTESIAN_POINT ( 'NONE',  ( -124.5228709571500048, -23.73907113216990084, -1.053371485793245910 ) ) ;
#12565 = CARTESIAN_POINT ( 'NONE',  ( -6.179238894844691465, -20.81818906610659425, -1.500000000000002220 ) ) ;
#12566 = CARTESIAN_POINT ( 'NONE',  ( -88.88918693012693950, -25.24179881669681080, 6.255794699373288914 ) ) ;
#12567 = CARTESIAN_POINT ( 'NONE',  ( -18.23695082634099407, 6.967386181637144738, -1.500000000000002220 ) ) ;
#12568 = DIRECTION ( 'NONE',  ( 0.7512896232465892110, 0.000000000000000000, 0.6599726524652350657 ) ) ;
#12569 = EDGE_CURVE ( 'NONE', #59330, #45280, #5836, .T. ) ;
#12570 = VERTEX_POINT ( 'NONE', #52387 ) ;
#12571 = CALENDAR_DATE ( 2026, 9, 10 ) ;
#12572 = CARTESIAN_POINT ( 'NONE',  ( 7.462166178408539352, -5.965225279485572685, -27.67315496249664974 ) ) ;
#12573 = CARTESIAN_POINT ( 'NONE',  ( -20.46784169311667867, 0.4426517378232717737, 11.49999999999999645 ) ) ;
#12574 = CARTESIAN_POINT ( 'NONE',  ( 7.858420481369514654, -6.475225279485573360, -27.14867965659404092 ) ) ;
#12575 = B_SPLINE_CURVE_WITH_KNOTS ( 'NONE', 3,
 ( #13016, #37374, #98252, #90159, #99253, #42996, #66346, #89662 ),
 .UNSPECIFIED., .F., .F.,
 ( 4, 2, 2, 4 ),
 ( 0.000000000000000000, 0.0005126904249026073470, 0.0007690356373538911796, 0.001025380849805175012 ),
 .UNSPECIFIED. ) ;
#12576 = LINE ( 'NONE', #41544, #75572 ) ;
#12577 = VERTEX_POINT ( 'NONE', #99531 ) ;
#12578 = CARTESIAN_POINT ( 'NONE',  ( -29.49875734969025842, -5.965225279485572685, 17.86602280011862476 ) ) ;
#12579 = CARTESIAN_POINT ( 'NONE',  ( 2.499999999999994671, 18.99999999999977618, 0.000000000000000000 ) ) ;
#12580 = CARTESIAN_POINT ( 'NONE',  ( -75.62287095715005592, -23.47596703998600631, 11.44779298504227860 ) ) ;
#12581 = CARTESIAN_POINT ( 'NONE',  ( -99.62287095715005592, -23.47593901973091235, -1.443836447539001089 ) ) ;
#12582 = VERTEX_POINT ( 'NONE', #6201 ) ;
#12583 = DIRECTION ( 'NONE',  ( 0.000000000000000000, 0.9999999999976377785, 2.173523156925979975E-06 ) ) ;
#12584 = AXIS2_PLACEMENT_3D ( 'NONE', #77153, #91386, #21863 ) ;
#12585 = EDGE_CURVE ( 'NONE', #95752, #75373, #17020, .T. ) ;
#12586 = CARTESIAN_POINT ( 'NONE',  ( -14.43837761634077310, -17.93274050997184332, 11.49999999999999645 ) ) ;
#12587 = CARTESIAN_POINT ( 'NONE',  ( -13.73562189146022661, -18.16285900770654393, 11.49999999999998934 ) ) ;
#12588 = CARTESIAN_POINT ( 'NONE',  ( -110.5975890800676780, -23.48786465467241769, 11.44779295918253759 ) ) ;
#12589 = B_SPLINE_SURFACE_WITH_KNOTS ( 'NONE', 3, 3, ( 
 ( #74941, #52623, #21161, #83052 ),
 ( #22149, #36397, #90185, #67860 ),
 ( #45024, #44009, #68848, #82567 ),
 ( #75944, #6448, #37405, #29281 ),
 ( #58740, #60252, #29782, #45521 ),
 ( #53137, #83559, #84063, #74460 ),
 ( #68351, #5446, #99766, #37897 ) ),
 .UNSPECIFIED., .F., .F., .F.,
 ( 4, 3, 4 ),
 ( 4, 4 ),
 ( 0.7945040050992232539, 0.8970133687736497885, 0.9995227324480763231 ),
 ( 0.5596362085602246683, 0.5609072983260594558 ),
 .UNSPECIFIED. ) ;
#12590 = LINE ( 'NONE', #34935, #90138 ) ;
#12591 = DIRECTION ( 'NONE',  ( 1.000000000000000000, -7.960204194457801640E-17, 0.000000000000000000 ) ) ;
#12592 = CARTESIAN_POINT ( 'NONE',  ( -70.52287095715010423, -24.83602698348161297, 1.605859176311264402 ) ) ;
#12593 = CARTESIAN_POINT ( 'NONE',  ( -110.6281984393044979, -24.40034930558991633, 0.3402023900116072364 ) ) ;
#12594 = ADVANCED_FACE ( 'NONE', ( #13802 ), #62828, .T. ) ;
#12595 = CARTESIAN_POINT ( 'NONE',  ( 16.40513048700843513, 14.50174154637248591, 11.49999999999998934 ) ) ;
#12596 = DIRECTION ( 'NONE',  ( -0.1593164160933055740, 0.000000000000000000, 0.9872275723272646575 ) ) ;
#12597 = CARTESIAN_POINT ( 'NONE',  ( -50.62287095715005592, -23.48786465467241058, 11.44779295918255180 ) ) ;
#12598 = CARTESIAN_POINT ( 'NONE',  ( -71.67930401912705918, -25.27253457059604358, 5.900159938492183898 ) ) ;
#12599 = CARTESIAN_POINT ( 'NONE',  ( 8.982289454725519207, -0.9478013341236714018, 3.727086380289612144 ) ) ;
#12600 = VERTEX_POINT ( 'NONE', #61504 ) ;
#12601 = PRODUCT_DEFINITION_SHAPE ( 'NONE', 'NONE',  #100426 ) ;
#12602 = CARTESIAN_POINT ( 'NONE',  ( 16.92567061652012228, 11.46397006495115534, 11.49999999999998934 ) ) ;
#12603 = VERTEX_POINT ( 'NONE', #32544 ) ;
#12604 = VERTEX_POINT ( 'NONE', #24924 ) ;
#12605 = ORIENTED_EDGE ( 'NONE', *, *, #96094, .F. ) ;
#12606 = VERTEX_POINT ( 'NONE', #61999 ) ;
#12607 = CARTESIAN_POINT ( 'NONE',  ( -8.820007276677138464, 21.28423624206370945, -1.500000000000002220 ) ) ;
#12608 = CARTESIAN_POINT ( 'NONE',  ( -61.59803820341726777, -23.96119346886880308, -0.6495511937832122440 ) ) ;
#12609 = CARTESIAN_POINT ( 'NONE',  ( -5.286950244708777724, -19.55949958832428948, -1.500000000000002220 ) ) ;
#12610 = ORIENTED_EDGE ( 'NONE', *, *, #33632, .T. ) ;
#12611 = CARTESIAN_POINT ( 'NONE',  ( -69.52287095715006160, -23.47596703998600631, 11.44779298504228748 ) ) ;
#12612 = VECTOR ( 'NONE', #58622, 1000.000000000000114 ) ;
#12613 = DIRECTION ( 'NONE',  ( -1.226388327005079762E-16, 0.000000000000000000, 1.000000000000000000 ) ) ;
#12614 = B_SPLINE_CURVE_WITH_KNOTS ( 'NONE', 3,
 ( #53569, #99212, #37826, #61184 ),
 .UNSPECIFIED., .F., .F.,
 ( 4, 4 ),
 ( 0.000000000000000000, 0.0001000000000000028644 ),
 .UNSPECIFIED. ) ;
#12615 = B_SPLINE_CURVE_WITH_KNOTS ( 'NONE', 3,
 ( #80216, #90198, #41673, #57405 ),
 .UNSPECIFIED., .F., .F.,
 ( 4, 4 ),
 ( 0.3490140499820214015, 0.3500147970227868166 ),
 .UNSPECIFIED. ) ;
#12616 = CARTESIAN_POINT ( 'NONE',  ( -51.62287095715004881, -23.72773821059535138, 11.05748984161097503 ) ) ;
#12617 = DIRECTION ( 'NONE',  ( -1.000000000000000000, -3.773278334444166432E-23, -8.201307841325785021E-29 ) ) ;
#12619 = VERTEX_POINT ( 'NONE', #100025 ) ;
#12618 = CARTESIAN_POINT ( 'NONE',  ( -13.85510387911049079, -16.26762222697724880, 11.49999999999999645 ) ) ;
#12620 = FACE_OUTER_BOUND ( 'NONE', #58034, .T. ) ;
#12621 = EDGE_LOOP ( 'NONE', ( #15258, #66402, #89594, #21119 ) ) ;
#12622 = CARTESIAN_POINT ( 'NONE',  ( 20.56042274393015035, -8.519965759701490171, -1.500000000000002220 ) ) ;
#12623 = CARTESIAN_POINT ( 'NONE',  ( -19.40337959798338119, 7.141409694766009508, 11.49999999999998934 ) ) ;
#12624 = VECTOR ( 'NONE', #59946, 1000.000000000000000 ) ;
#12625 = ORIENTED_EDGE ( 'NONE', *, *, #73195, .T. ) ;
#12626 = CARTESIAN_POINT ( 'NONE',  ( -70.78987763377477904, -25.30060019737137367, 6.009288023823078362 ) ) ;
#12627 = VERTEX_POINT ( 'NONE', #1605 ) ;
#12628 = CARTESIAN_POINT ( 'NONE',  ( -61.58953762381672448, -24.66019654487198665, 8.947790411086129936 ) ) ;
#12629 = AXIS2_PLACEMENT_3D ( 'NONE', #24093, #70284, #76867 ) ;
#12630 = ORIENTED_EDGE ( 'NONE', *, *, #95022, .F. ) ;
#12631 = CARTESIAN_POINT ( 'NONE',  ( 10.03794737889396771, 18.37758748099471973, -1.500000000000002220 ) ) ;
#12632 = CARTESIAN_POINT ( 'NONE',  ( -19.17877449816284496, 10.63638241594707345, 11.49999999999999645 ) ) ;
#12633 = CARTESIAN_POINT ( 'NONE',  ( -73.64959498640008917, -23.48786465467241058, 11.44779295918254824 ) ) ;
#12634 = CARTESIAN_POINT ( 'NONE',  ( -22.39070119279581306, -2.479732019442284496, 11.49999999999998934 ) ) ;
#12635 = CARTESIAN_POINT ( 'NONE',  ( 19.40473180639871131, -7.901900427366274293, -1.500000000000002220 ) ) ;
#12636 = CARTESIAN_POINT ( 'NONE',  ( -106.5895376238167387, -23.47596703998600631, 11.44779298504227683 ) ) ;
#12637 = CARTESIAN_POINT ( 'NONE',  ( -75.52287095715007581, -23.47596703998600631, 11.44779298504228571 ) ) ;
#12638 = CARTESIAN_POINT ( 'NONE',  ( -99.52287095715009002, -24.66019654487200441, 8.947790411086119278 ) ) ;
#12639 = VERTEX_POINT ( 'NONE', #69096 ) ;
#12640 = VERTEX_POINT ( 'NONE', #85830 ) ;
#12641 = ORIENTED_EDGE ( 'NONE', *, *, #52203, .T. ) ;
#12642 = CARTESIAN_POINT ( 'NONE',  ( -66.58006201227493648, -24.65952944569304250, 1.056160979905692798 ) ) ;
#12643 = CARTESIAN_POINT ( 'NONE',  ( -3.867184171070207288, -21.11305558764578194, -1.500000000000002220 ) ) ;
#12644 = EDGE_CURVE ( 'NONE', #51886, #84743, #94438, .T. ) ;
#12645 = CARTESIAN_POINT ( 'NONE',  ( -121.6228709571500275, -24.66019654487200441, 8.947790411086119278 ) ) ;
#12646 = ORIENTED_EDGE ( 'NONE', *, *, #68929, .T. ) ;
#12647 = CARTESIAN_POINT ( 'NONE',  ( -3.607955376466517095, 20.77440192976073519, -1.500000000000002220 ) ) ;
#12648 = CARTESIAN_POINT ( 'NONE',  ( 17.51792015816173986, -5.965225279485572685, 29.01255224319336889 ) ) ;
#12649 = EDGE_CURVE ( 'NONE', #884, #91131, #45729, .T. ) ;
#12650 = CARTESIAN_POINT ( 'NONE',  ( -52.62287095715004170, -24.51283580621364777, 0.6167428607019739273 ) ) ;
#12651 = CARTESIAN_POINT ( 'NONE',  ( -50.65952796453198914, -23.85049219812685095, 10.88485053497527133 ) ) ;
#12652 = CARTESIAN_POINT ( 'NONE',  ( 14.76093561896378326, -3.316774720514426456, -26.55548769130088260 ) ) ;
#12653 = CARTESIAN_POINT ( 'NONE',  ( -129.5219949681614935, -24.15620529776629155, 10.23563542870659759 ) ) ;
#12654 = CARTESIAN_POINT ( 'NONE',  ( 7.643743511751816655, -20.74876368896106271, -1.500000000000002220 ) ) ;
#12655 = PLANE ( 'NONE',  #15998 ) ;
#12656 = ADVANCED_FACE ( 'NONE', ( #31535 ), #15809, .T. ) ;
#12657 = LINE ( 'NONE', #45126, #31956 ) ;
#12658 = DIRECTION ( 'NONE',  ( -0.000000000000000000, -1.000000000000000000, -0.000000000000000000 ) ) ;
#12659 = EDGE_CURVE ( 'NONE', #65405, #66719, #62632, .T. ) ;
#12660 = CARTESIAN_POINT ( 'NONE',  ( -100.6015228439523099, -23.48783264082476663, -1.443836473390090358 ) ) ;
#12661 = EDGE_CURVE ( 'NONE', #64249, #35854, #60784, .T. ) ;
#12662 = CARTESIAN_POINT ( 'NONE',  ( 9.194277187580093269, -19.27880637823015419, 11.49999999999998934 ) ) ;
#12663 = CARTESIAN_POINT ( 'NONE',  ( -100.6814946224345846, -25.30267106336103922, 4.736250553104468963 ) ) ;
#12664 = EDGE_CURVE ( 'NONE', #88647, #71294, #988, .T. ) ;
#12665 = CARTESIAN_POINT ( 'NONE',  ( -50.92528559392947329, -25.03707831087709579, 7.590867751134624974 ) ) ;
#12666 = CARTESIAN_POINT ( 'NONE',  ( -0.1469176100155287212, -21.14803608454491268, 11.46586199002818951 ) ) ;
#12667 = DIRECTION ( 'NONE',  ( 0.000000000000000000, 0.000000000000000000, 1.000000000000000000 ) ) ;
#12668 = CARTESIAN_POINT ( 'NONE',  ( -22.43363504178351775, 2.973318333978472339, -1.500000000000002220 ) ) ;
#12669 = B_SPLINE_SURFACE_WITH_KNOTS ( 'NONE', 3, 3, ( 
 ( #31476, #23854, #23344, #46712 ),
 ( #60938, #62436, #7641, #76137 ),
 ( #93363, #6634, #54829, #38587 ),
 ( #54329, #53826, #70037, #85764 ),
 ( #22340, #83754, #62947, #24363 ),
 ( #37590, #30970, #53324, #84254 ),
 ( #14739, #15245, #85254, #7132 ) ),
 .UNSPECIFIED., .F., .F., .F.,
 ( 4, 3, 4 ),
 ( 4, 4 ),
 ( 0.7945040050992242531, 0.8970133687736501216, 0.9995227324480759901 ),
 ( 0.5196260414224536106, 0.5208786598400961809 ),
 .UNSPECIFIED. ) ;
#12670 = ORIENTED_EDGE ( 'NONE', *, *, #68543, .T. ) ;
#12671 = DIRECTION ( 'NONE',  ( 1.000000000000000000, 0.000000000000000000, -1.611864046919725738E-15 ) ) ;
#12672 = CARTESIAN_POINT ( 'NONE',  ( -79.54044106604338538, -24.65952944569304606, 1.056160979905700126 ) ) ;
#12673 = CARTESIAN_POINT ( 'NONE',  ( 3.912202881759007767, 19.34271161525698091, 11.49999999999999645 ) ) ;
#12674 = LINE ( 'NONE', #4584, #77993 ) ;
#12675 = DIRECTION ( 'NONE',  ( -0.000000000000000000, -0.000000000000000000, -1.000000000000000000 ) ) ;
#12676 = EDGE_LOOP ( 'NONE', ( #44347, #22570, #72070, #35851 ) ) ;
#12677 = CARTESIAN_POINT ( 'NONE',  ( 7.207151257207165429, -5.965225279485574461, -28.24477140324590252 ) ) ;
#12678 = CARTESIAN_POINT ( 'NONE',  ( -29.12854162637831834, -24.60094034115323680, 2.289900629743222282 ) ) ;
#12679 = DIRECTION ( 'NONE',  ( -0.5656310827093757876, -0.8246584009594636333, -1.161164194647626387E-16 ) ) ;
#12680 = CARTESIAN_POINT ( 'NONE',  ( 5.568959250215116619, -20.88136358707659923, -1.500000000000002220 ) ) ;
#12681 = DIRECTION ( 'NONE',  ( 0.000000000000000000, 0.000000000000000000, 1.000000000000000000 ) ) ;
#12682 = CIRCLE ( 'NONE', #53260, 20.00000000000000355 ) ;
#12683 = CARTESIAN_POINT ( 'NONE',  ( -12.28997142660015740, 14.97987746540053422, -1.500000000000002220 ) ) ;
#12684 = CARTESIAN_POINT ( 'NONE',  ( -50.52287095715006160, -23.47593901973090169, -1.443836447538997092 ) ) ;
#12685 = CARTESIAN_POINT ( 'NONE',  ( -81.38737579674543099, -25.10497842348888042, 7.257320789189920518 ) ) ;
#12686 = CARTESIAN_POINT ( 'NONE',  ( -18.99895575154661742, -5.639348582513488140, 11.49999999999998934 ) ) ;
#12687 = VERTEX_POINT ( 'NONE', #23922 ) ;
#12688 = CARTESIAN_POINT ( 'NONE',  ( 19.26017855675105750, 6.235128648364509196, 11.49999999999999645 ) ) ;
#12689 = FACE_OUTER_BOUND ( 'NONE', #67223, .T. ) ;
#12690 = CARTESIAN_POINT ( 'NONE',  ( -51.62287095715005592, -24.65952944569304250, 1.056160979905695019 ) ) ;
#12691 = ORIENTED_EDGE ( 'NONE', *, *, #77301, .T. ) ;
#12692 = CARTESIAN_POINT ( 'NONE',  ( 33.28704981706498955, 4.441298812401576868, -11.58844794911118647 ) ) ;
#12693 = CARTESIAN_POINT ( 'NONE',  ( -11.64875734969026233, -0.3587747205144265483, 31.02402280011862246 ) ) ;
#12694 = CIRCLE ( 'NONE', #95347, 6.600000000000001421 ) ;
#12695 = CARTESIAN_POINT ( 'NONE',  ( -92.52287095715009002, -24.66019654487200086, 8.947790411086115725 ) ) ;
#12696 = CARTESIAN_POINT ( 'NONE',  ( -60.52287095715006160, -29.50249982740957577, 7.747779886224967605 ) ) ;
#12697 = CARTESIAN_POINT ( 'NONE',  ( -12.65591448191638335, 15.52279176289047236, 11.49999999999998934 ) ) ;
#12698 = CARTESIAN_POINT ( 'NONE',  ( -8.160000000000000142, -10.15233964170348457, 0.003711184059992174607 ) ) ;
#12699 = ORIENTED_EDGE ( 'NONE', *, *, #12281, .F. ) ;
#12700 = AXIS2_PLACEMENT_3D ( 'NONE', #94568, #63644, #38779 ) ;
#12701 = CARTESIAN_POINT ( 'NONE',  ( -49.50986403386431078, -25.31297060778654995, 4.014908341799525715 ) ) ;
#12702 = DIRECTION ( 'NONE',  ( 0.000000000000000000, -1.000000000000000000, 0.000000000000000000 ) ) ;
#12703 = CARTESIAN_POINT ( 'NONE',  ( -129.5228709571500758, -24.64965694238408034, 8.947790433994189385 ) ) ;
#12704 = PLANE ( 'NONE',  #20511 ) ;
#12705 = ADVANCED_FACE ( 'NONE', ( #38648 ), #46209, .F. ) ;
#12706 = CARTESIAN_POINT ( 'NONE',  ( -79.11611000704996854, -29.50248939449842922, 2.947779886236309377 ) ) ;
#12707 = EDGE_CURVE ( 'NONE', #32707, #55189, #32042, .T. ) ;
#12708 = CARTESIAN_POINT ( 'NONE',  ( -19.37210865224160017, -5.965225279485592225, -21.60955166348795586 ) ) ;
#12709 = VERTEX_POINT ( 'NONE', #93428 ) ;
#12710 = CARTESIAN_POINT ( 'NONE',  ( 3.964343641299885146, 19.94596313931659992, 11.49999999999998934 ) ) ;
#12711 = EDGE_LOOP ( 'NONE', ( #93864, #25530, #27483, #91794 ) ) ;
#12712 = CARTESIAN_POINT ( 'NONE',  ( 20.74614131242519477, 9.816050768296040729, 11.49999999999998934 ) ) ;
#12713 = CARTESIAN_POINT ( 'NONE',  ( 7.160000000000000142, -6.754662360505032659, 7.925641719537454222 ) ) ;
#12714 = VERTEX_POINT ( 'NONE', #31034 ) ;
#12715 = CARTESIAN_POINT ( 'NONE',  ( -89.52287095715003318, -23.48783264083374789, -1.443836473376144180 ) ) ;
#12716 = CARTESIAN_POINT ( 'NONE',  ( -49.27993637813898431, -25.12215232176118107, 6.239169103029740704 ) ) ;
#12717 = CARTESIAN_POINT ( 'NONE',  ( -38.55620429048340725, -24.66019654487199020, 8.947790411086135265 ) ) ;
#12719 = ORIENTED_EDGE ( 'NONE', *, *, #17382, .F. ) ;
#12718 = CARTESIAN_POINT ( 'NONE',  ( -14.68016216564755894, -15.32010671487267572, 11.49999999999999645 ) ) ;
#12720 = ORIENTED_EDGE ( 'NONE', *, *, #46353, .F. ) ;
#12721 = CARTESIAN_POINT ( 'NONE',  ( -20.56242917251232782, -8.299981740788712870, -1.500000000000002220 ) ) ;
#12722 = CARTESIAN_POINT ( 'NONE',  ( 1.511266892140219920, 20.53031905857337591, -1.500000000000002220 ) ) ;
#12723 = VERTEX_POINT ( 'NONE', #45767 ) ;
#12724 = ORIENTED_EDGE ( 'NONE', *, *, #22814, .F. ) ;
#12725 = DIRECTION ( 'NONE',  ( -1.000000000000000000, -3.773278334444167608E-23, -8.201307833595939069E-29 ) ) ;
#12726 = CARTESIAN_POINT ( 'NONE',  ( -49.62287095715004881, -24.50216790748097395, 0.6166512839513585975 ) ) ;
#12727 = EDGE_LOOP ( 'NONE', ( #94505, #13987, #9221, #88334, #94414, #5990, #59959, #770 ) ) ;
#12728 = VERTEX_POINT ( 'NONE', #70606 ) ;
#12729 = VECTOR ( 'NONE', #41003, 1000.000000000000000 ) ;
#12730 = VERTEX_POINT ( 'NONE', #589 ) ;
#12731 = CARTESIAN_POINT ( 'NONE',  ( -4.993225604111835914, 5.965225279485592225, -29.11654937215278593 ) ) ;
#12732 = CARTESIAN_POINT ( 'NONE',  ( -71.52287095715007581, -24.64965694238408034, 8.947790433994200043 ) ) ;
#12733 = CARTESIAN_POINT ( 'NONE',  ( 22.81105451610979173, 6.475225279485573360, -18.46691820600746681 ) ) ;
#12734 = CARTESIAN_POINT ( 'NONE',  ( -18.43438512255917772, -9.567967903218889347, -1.500000000000002220 ) ) ;
#12735 = CARTESIAN_POINT ( 'NONE',  ( 17.47290450027814757, -12.96279059203284767, 11.49999999999999645 ) ) ;
#12736 = ORIENTED_EDGE ( 'NONE', *, *, #37346, .F. ) ;
#12737 = CARTESIAN_POINT ( 'NONE',  ( -44.62287095715004881, -29.50248528299804818, 1.056150453629031594 ) ) ;
#12738 = CARTESIAN_POINT ( 'NONE',  ( -98.89303308397303738, -25.25494757631710385, 6.110950176066591411 ) ) ;
#12739 = CARTESIAN_POINT ( 'NONE',  ( 30.09341516180546350, -2.682774720514426559, -11.39311774897855933 ) ) ;
#12740 = CARTESIAN_POINT ( 'NONE',  ( -21.67104271438225638, 5.786422744429515319, -1.500000000000002220 ) ) ;
#12741 = VECTOR ( 'NONE', #92236, 1000.000000000000000 ) ;
#12742 = CARTESIAN_POINT ( 'NONE',  ( 32.85081302853804885, -3.622774720514426949, -13.10817780685210643 ) ) ;
#12743 = CARTESIAN_POINT ( 'NONE',  ( -65.55949795840675165, -23.85016227208580730, -0.8807180028928343063 ) ) ;
#12744 = VERTEX_POINT ( 'NONE', #7192 ) ;
#12745 = CARTESIAN_POINT ( 'NONE',  ( -75.52287095715007581, -23.47593901973090169, -1.443836447538996870 ) ) ;
#12746 = CARTESIAN_POINT ( 'NONE',  ( 27.86270917940689174, -0.3587747205144265483, 29.02104833056109001 ) ) ;
#12747 = ORIENTED_EDGE ( 'NONE', *, *, #91106, .T. ) ;
#12748 = VECTOR ( 'NONE', #74849, 1000.000000000000227 ) ;
#12749 = EDGE_LOOP ( 'NONE', ( #15637, #66835, #35684, #19356 ) ) ;
#12750 = PLANE ( 'NONE',  #449 ) ;
#12751 = ORIENTED_EDGE ( 'NONE', *, *, #13158, .F. ) ;
#12752 = B_SPLINE_CURVE_WITH_KNOTS ( 'NONE', 3,
 ( #55587, #71304, #56593, #73791, #90020, #4290, #35240, #44355, #42862, #11397, #12385, #75280, #51962, #27125 ),
 .UNSPECIFIED., .F., .F.,
 ( 4, 2, 2, 2, 2, 2, 4 ),
 ( 9.813077866773594792E-18, 0.0001940785162856977137, 0.0003881570325713856154, 0.0007763140651427799044, 0.001164471097714174031, 0.001358549613999873208, 0.001552628130285572602 ),
 .UNSPECIFIED. ) ;
#12753 = CARTESIAN_POINT ( 'NONE',  ( -8.014198274750887308, -19.69740135394370384, -1.500000000000002220 ) ) ;
#12754 = EDGE_LOOP ( 'NONE', ( #9259, #64430, #100213 ) ) ;
#12755 = DIRECTION ( 'NONE',  ( -0.9978940991575084851, -0.000000000000000000, -0.06486421869277853025 ) ) ;
#12756 = CARTESIAN_POINT ( 'NONE',  ( 17.39636294008568740, -13.23181597624684791, -1.500000000000002220 ) ) ;
#12757 = CARTESIAN_POINT ( 'NONE',  ( -124.5895376238167387, -23.47596703998600631, 11.44779298504227683 ) ) ;
#12758 = CARTESIAN_POINT ( 'NONE',  ( 4.020035926878589905, 22.33396232419688587, -1.500000000000002220 ) ) ;
#12759 = AXIS2_PLACEMENT_3D ( 'NONE', #78466, #86091, #94703 ) ;
#12760 = CARTESIAN_POINT ( 'NONE',  ( 7.403636664866980688, -6.376774720514424288, 21.18544102487025782 ) ) ;
#12761 = DIRECTION ( 'NONE',  ( -1.000000000000000000, 0.000000000000000000, 0.000000000000000000 ) ) ;
#12762 = CARTESIAN_POINT ( 'NONE',  ( 20.73430856240977249, 7.200853762728330665, -1.500000000000002220 ) ) ;
#12763 = CARTESIAN_POINT ( 'NONE',  ( -100.5228709571500616, -25.00158670708909625, 2.256160236439166411 ) ) ;
#12764 = VERTEX_POINT ( 'NONE', #1098 ) ;
#12765 = CARTESIAN_POINT ( 'NONE',  ( -122.5572053947523585, -23.48786465467241769, 11.44779295918253581 ) ) ;
#12766 = DIRECTION ( 'NONE',  ( 1.000000000000000000, 0.000000000000000000, 0.000000000000000000 ) ) ;
#12767 = EDGE_CURVE ( 'NONE', #97595, #51586, #62499, .T. ) ;
#12769 = ORIENTED_EDGE ( 'NONE', *, *, #82424, .T. ) ;
#12768 = ADVANCED_FACE ( 'NONE', ( #63013 ), #86330, .T. ) ;
#12770 = DIRECTION ( 'NONE',  ( 3.773278334444167608E-23, -1.000000000000000000, 0.000000000000000000 ) ) ;
#12771 = EDGE_CURVE ( 'NONE', #833, #52813, #13012, .T. ) ;
#12772 = CARTESIAN_POINT ( 'NONE',  ( 14.61581670307174008, 6.475225279485573360, -27.35847990810646024 ) ) ;
#12773 = CARTESIAN_POINT ( 'NONE',  ( -0.05753151201984656182, -22.30520936630598072, 1.095224832288506089 ) ) ;
#12774 = CARTESIAN_POINT ( 'NONE',  ( -20.86817740539179056, 4.147639786170328691, -1.500000000000002220 ) ) ;
#12775 = CARTESIAN_POINT ( 'NONE',  ( -8.376690734369036662, 12.50000000000004974, 2.100000000000000089 ) ) ;
#12776 = EDGE_CURVE ( 'NONE', #61188, #10237, #72340, .T. ) ;
#12777 = CARTESIAN_POINT ( 'NONE',  ( -26.10669942825130363, -24.97064885537375645, 4.499505497235293916 ) ) ;
#12778 = CARTESIAN_POINT ( 'NONE',  ( -85.59145065735712876, -24.40034930558991633, 0.3402023900116044608 ) ) ;
#12779 = CARTESIAN_POINT ( 'NONE',  ( -68.55932668679069764, -23.73766607897670156, -1.055555164236458232 ) ) ;
#12780 = CLOSED_SHELL ( 'NONE', ( #94564, #48137, #64114, #87577, #19854, #67713, #6787, #7043, #54379, #88561, #81574, #30448, #77872, #60883, #7909, #7963, #64305, #82317, #67653, #37429, #1159, #86121, #27203, #72171, #188, #59072, #6249, #65348, #78713, #15968, #40513, #38544, #14625, #83633, #5337, #63231, #61581, #26786, #93106, #14616, #20344, #85617, #16875, #55508, #58982, #16793, #80241, #29627, #19073, #78202, #80819, #80245, #27682, #14657, #30764, #60782, #83207, #82746, #20306, #58940, #10424, #26287, #856, #65132, #30973, #86299, #14500, #9953 ) ) ;
#12781 = CARTESIAN_POINT ( 'NONE',  ( -32.58953762381671737, -23.47593901973091235, -1.443836447539013301 ) ) ;
#12782 = ORIENTED_EDGE ( 'NONE', *, *, #60097, .T. ) ;
#12783 = CARTESIAN_POINT ( 'NONE',  ( -9.112395119859147741, -17.30902560603237106, 11.49999999999999645 ) ) ;
#12784 = CARTESIAN_POINT ( 'NONE',  ( -78.52287095715006160, -24.35013146730203815, 9.818937971375097717 ) ) ;
#12785 = CARTESIAN_POINT ( 'NONE',  ( -118.5228709571501184, -23.48783264082477373, -1.443836473390083475 ) ) ;
#12786 = EDGE_CURVE ( 'NONE', #29980, #9998, #9710, .T. ) ;
#12787 = ORIENTED_EDGE ( 'NONE', *, *, #94896, .T. ) ;
#12788 = DIRECTION ( 'NONE',  ( -3.773278334453079030E-23, 0.9999999999976377785, 2.173523156925979128E-06 ) ) ;
#12789 = CARTESIAN_POINT ( 'NONE',  ( -7.999999999999996447, -5.876774720514426953, 0.000000000000000000 ) ) ;
#12790 = CARTESIAN_POINT ( 'NONE',  ( -27.24607494285254816, -24.62946685170201633, 8.199799071658667060 ) ) ;
#12791 = CARTESIAN_POINT ( 'NONE',  ( -75.52287095715004739, -25.00182538069145366, 7.747789668545101094 ) ) ;
#12792 = CARTESIAN_POINT ( 'NONE',  ( 10.64064036176630879, -16.58286410872727146, -1.500000000000002220 ) ) ;
#12793 = ORIENTED_EDGE ( 'NONE', *, *, #82545, .F. ) ;
#12794 = CARTESIAN_POINT ( 'NONE',  ( -108.6228709571500417, -23.47596703998600631, 11.44779298504227860 ) ) ;
#12795 = CARTESIAN_POINT ( 'NONE',  ( 1.000208336950358934, 0.000000000000000000, 0.000000000000000000 ) ) ;
#12796 = PERSON_AND_ORGANIZATION ( #70597, #27821 ) ;
#12797 = ORIENTED_EDGE ( 'NONE', *, *, #32537, .T. ) ;
#12798 = CARTESIAN_POINT ( 'NONE',  ( 8.567893164715615129, -0.1262136116457340251, 3.707288619710387145 ) ) ;
#12799 = LINE ( 'NONE', #84314, #86318 ) ;
#12800 = CARTESIAN_POINT ( 'NONE',  ( -47.66149957754198851, -23.48783264082478084, -1.443836473390071928 ) ) ;
#12801 = CARTESIAN_POINT ( 'NONE',  ( -118.5902651629808560, -24.15543982623907837, -0.2315651400026558782 ) ) ;
#12802 = PLANE ( 'NONE',  #9605 ) ;
#12803 = AXIS2_PLACEMENT_3D ( 'NONE', #34936, #75472, #4983 ) ;
#12804 = AXIS2_PLACEMENT_3D ( 'NONE', #34199, #97580, #66667 ) ;
#12805 = CARTESIAN_POINT ( 'NONE',  ( 9.478389368232452483, -4.132774720514426292, -23.17485683983816003 ) ) ;
#12806 = CARTESIAN_POINT ( 'NONE',  ( -85.55620429048337883, -25.00158670708909625, 2.256160236439166855 ) ) ;
#12807 = CARTESIAN_POINT ( 'NONE',  ( 18.73470368118781693, 6.836574088118649861, 11.49999999999998934 ) ) ;
#12808 = CARTESIAN_POINT ( 'NONE',  ( 26.25551457520358056, -4.772774720514425972, -10.59759736550660492 ) ) ;
#12809 = CARTESIAN_POINT ( 'NONE',  ( -0.008299077606883394423, -22.94256191861778760, 3.420120028211836694 ) ) ;
#12810 = ORIENTED_EDGE ( 'NONE', *, *, #47760, .T. ) ;
#12811 = VECTOR ( 'NONE', #32571, 1000.000000000000114 ) ;
#12812 = CARTESIAN_POINT ( 'NONE',  ( -3.212051231530181017, 17.72614232434105475, 8.999999999999998224 ) ) ;
#12813 = CARTESIAN_POINT ( 'NONE',  ( 11.59154397149680626, -4.779967012825416361, -27.71550087055790712 ) ) ;
#12814 = EDGE_CURVE ( 'NONE', #39855, #733, #33693, .T. ) ;
#12815 =( NAMED_UNIT ( * ) PLANE_ANGLE_UNIT ( ) SI_UNIT ( $, .RADIAN. ) );
#12816 = CARTESIAN_POINT ( 'NONE',  ( -28.98875734969026396, 5.965225279485572685, 0.1180228001186258285 ) ) ;
#12817 = CARTESIAN_POINT ( 'NONE',  ( -127.4728709572981415, -25.30561157749831480, 5.197923170786341807 ) ) ;
#12818 = CARTESIAN_POINT ( 'NONE',  ( -81.55065612788921214, -24.15543982623907482, -0.2315651400026469686 ) ) ;
#12819 = AXIS2_PLACEMENT_3D ( 'NONE', #64429, #62918, #48692 ) ;
#12820 = EDGE_CURVE ( 'NONE', #17742, #73137, #17316, .T. ) ;
#12821 = CARTESIAN_POINT ( 'NONE',  ( -75.52287095715007581, -23.47593901973090169, -1.443836447538996870 ) ) ;
#12822 = CARTESIAN_POINT ( 'NONE',  ( -51.09576285965076181, -25.26280100839387543, 4.912419055384075861 ) ) ;
#12823 = ORIENTED_EDGE ( 'NONE', *, *, #99672, .F. ) ;
#12824 = CARTESIAN_POINT ( 'NONE',  ( -34.62287095715005592, -24.65952944569303895, 1.056160979905691688 ) ) ;
#12825 = CARTESIAN_POINT ( 'NONE',  ( -127.5219661461652265, -23.73766607897670866, -1.055555164236447574 ) ) ;
#12826 = ORIENTED_EDGE ( 'NONE', *, *, #62083, .F. ) ;
#12827 = VECTOR ( 'NONE', #25207, 1000.000000000000114 ) ;
#12828 = B_SPLINE_CURVE_WITH_KNOTS ( 'NONE', 3,
 ( #96967, #12217, #36064, #50306, #90353, #34581 ),
 .UNSPECIFIED., .F., .F.,
 ( 4, 2, 4 ),
 ( 6.384118678616914202E-06, 0.001386860460828380189, 0.002767336802978143193 ),
 .UNSPECIFIED. ) ;
#12829 = CARTESIAN_POINT ( 'NONE',  ( 12.15850541088210868, 16.18036119754114566, -1.500000000000002220 ) ) ;
#12830 = CARTESIAN_POINT ( 'NONE',  ( -128.5228709571501042, -24.66019654487200441, 8.947790411086108620 ) ) ;
#12831 = CARTESIAN_POINT ( 'NONE',  ( 0.7395552074414002419, -5.331939213628640317, 8.999999999999998224 ) ) ;
#12832 = CARTESIAN_POINT ( 'NONE',  ( -86.52287095715006160, -29.50247984919015209, -1.443849546365051806 ) ) ;
#12833 = EDGE_LOOP ( 'NONE', ( #45067, #13051, #8692, #19143, #50817, #48485, #92645, #12947, #74760, #45977, #18158, #91579 ) ) ;
#12834 = CARTESIAN_POINT ( 'NONE',  ( -77.52287095715006160, -24.33927499327854349, 9.819080762295806508 ) ) ;
#12835 = DIRECTION ( 'NONE',  ( -0.000000000000000000, 1.000000000000000000, -0.000000000000000000 ) ) ;
#12836 = CARTESIAN_POINT ( 'NONE',  ( -19.96166555454951208, -2.086822695551191043, -1.500000000000002220 ) ) ;
#12837 = CARTESIAN_POINT ( 'NONE',  ( 17.94697546605861760, -10.91086909363634838, 11.49999999999999645 ) ) ;
#12838 = CARTESIAN_POINT ( 'NONE',  ( -27.83177597161019179, -24.82260152899532102, 7.598324359836099440 ) ) ;
#12839 = CARTESIAN_POINT ( 'NONE',  ( -32.52287095715005449, -23.73907113217656573, -1.053371485781500860 ) ) ;
#12840 = CARTESIAN_POINT ( 'NONE',  ( -21.77411086464670831, -3.637377321037103872, -1.500000000000002220 ) ) ;
#12841 = CC_DESIGN_DATE_AND_TIME_ASSIGNMENT ( #45018, #97297, ( #40782 ) ) ;
#12842 = CARTESIAN_POINT ( 'NONE',  ( -27.96875734969026084, 6.475225279485573360, 0.7300228001186309656 ) ) ;
#12843 = VECTOR ( 'NONE', #87953, 1000.000000000000114 ) ;
#12844 = CARTESIAN_POINT ( 'NONE',  ( -76.58953762381673869, -23.47593901973091235, -1.443836447539004642 ) ) ;
#12845 = FACE_OUTER_BOUND ( 'NONE', #84777, .T. ) ;
#12846 = ORIENTED_EDGE ( 'NONE', *, *, #79169, .F. ) ;
#12847 = CARTESIAN_POINT ( 'NONE',  ( 6.403846153846157740, -6.376774720514426065, 21.48076923076922995 ) ) ;
#12848 = B_SPLINE_SURFACE_WITH_KNOTS ( 'NONE', 3, 3, ( 
 ( #73766, #66688, #43822, #29582 ),
 ( #68157, #66187, #12854, #97107 ),
 ( #59553, #12358, #51438, #19974 ),
 ( #74269, #35714, #74756, #37204 ),
 ( #5252, #21456, #51937, #82866 ),
 ( #67669, #44329, #75258, #5750 ),
 ( #98590, #13853, #29084, #60058 ) ),
 .UNSPECIFIED., .F., .F., .F.,
 ( 4, 3, 4 ),
 ( 4, 4 ),
 ( 0.0004766839783822049946, 0.1029713700210897892, 0.2054660560637973643 ),
 ( 0.5396312702239698389, 0.5408929796565489223 ),
 .UNSPECIFIED. ) ;
#12849 = LINE ( 'NONE', #81876, #9717 ) ;
#12850 = ORIENTED_EDGE ( 'NONE', *, *, #38089, .T. ) ;
#12851 = ORIENTED_EDGE ( 'NONE', *, *, #86227, .F. ) ;
#12852 = CARTESIAN_POINT ( 'NONE',  ( -55.52287095715008292, -24.52232992886361629, 0.6492154411906015943 ) ) ;
#12853 = CARTESIAN_POINT ( 'NONE',  ( -97.52287095715006160, -24.65952944569304606, 1.056160979905702346 ) ) ;
#12854 = CARTESIAN_POINT ( 'NONE',  ( -76.55889680453810797, -23.73766607897670866, -1.055555164236452681 ) ) ;
#12855 = CARTESIAN_POINT ( 'NONE',  ( -10.57813111170615983, 17.65445453266677234, -1.500000000000002220 ) ) ;
#12856 = CARTESIAN_POINT ( 'NONE',  ( -20.03152041342270806, -8.007337437543776915, 11.49999999999999645 ) ) ;
#12857 = ORIENTED_EDGE ( 'NONE', *, *, #11016, .F. ) ;
#12858 = CARTESIAN_POINT ( 'NONE',  ( 31.64143112576189765, -5.965225279485572685, 14.03360796525321774 ) ) ;
#12859 = CARTESIAN_POINT ( 'NONE',  ( -121.6228709571500417, -23.48786465467241769, 11.44779295918253759 ) ) ;
#12860 = CARTESIAN_POINT ( 'NONE',  ( -4.312370003044874167, -6.376774720514408301, 19.42522865122897358 ) ) ;
#12861 = CARTESIAN_POINT ( 'NONE',  ( 13.15158565771796084, -18.08388448789661851, -1.500000000000002220 ) ) ;
#12862 = CARTESIAN_POINT ( 'NONE',  ( -62.52287095715006160, -23.48783264082477018, -1.443836473390091912 ) ) ;
#12863 = CARTESIAN_POINT ( 'NONE',  ( -84.63607199451277552, -23.96119346886880663, -0.6495511937832096905 ) ) ;
#12864 = ORIENTED_EDGE ( 'NONE', *, *, #69130, .F. ) ;
#12865 = PLANE ( 'NONE',  #24189 ) ;
#12866 = PLANE ( 'NONE',  #68566 ) ;
#12867 = CARTESIAN_POINT ( 'NONE',  ( -0.8937202392249329330, 20.86669477224961256, -1.500000000000002220 ) ) ;
#12868 = EDGE_LOOP ( 'NONE', ( #37875, #4852, #68043, #96780, #83024, #88678 ) ) ;
#12870 = ORIENTED_EDGE ( 'NONE', *, *, #54648, .T. ) ;
#12869 = CARTESIAN_POINT ( 'NONE',  ( -29.49875734969025842, -5.965225279485572685, 23.37402280011862743 ) ) ;
#12871 = ORIENTED_EDGE ( 'NONE', *, *, #30311, .F. ) ;
#12872 = CARTESIAN_POINT ( 'NONE',  ( -100.5179223032556024, -23.85049219812686161, 10.88485053497527133 ) ) ;
#12873 = CARTESIAN_POINT ( 'NONE',  ( -16.61111445048470614, -13.04167290785011701, -1.500000000000002220 ) ) ;
#12874 = VERTEX_POINT ( 'NONE', #25431 ) ;
#12875 = CARTESIAN_POINT ( 'NONE',  ( -117.5885033326503475, -24.51314013834316086, 0.6176544820404201719 ) ) ;
#12876 = CARTESIAN_POINT ( 'NONE',  ( 6.666194146093591399, -5.876774720514413630, 19.75460921626947908 ) ) ;
#12877 = CARTESIAN_POINT ( 'NONE',  ( -109.8650282762807393, -25.28040082146351608, 5.784628005357986602 ) ) ;
#12878 = VECTOR ( 'NONE', #89621, 1000.000000000000114 ) ;
#12879 = DIRECTION ( 'NONE',  ( 0.000000000000000000, -2.173523156925979552E-06, 0.9999999999976378895 ) ) ;
#12880 = CARTESIAN_POINT ( 'NONE',  ( -49.10457154551148307, -25.26416398485831749, 3.999772271414141489 ) ) ;
#12881 = CARTESIAN_POINT ( 'NONE',  ( -11.39883337241029793, 18.50525654427185884, -1.500000000000002220 ) ) ;
#12882 = CARTESIAN_POINT ( 'NONE',  ( -107.5562042904834072, -23.48783264082478794, -1.443836473390060160 ) ) ;
#12883 = EDGE_CURVE ( 'NONE', #45125, #50697, #10574, .T. ) ;
#12885 = ORIENTED_EDGE ( 'NONE', *, *, #75635, .F. ) ;
#12884 = CARTESIAN_POINT ( 'NONE',  ( 20.80681148587913754, 8.022540738981085440, 11.49999999999999645 ) ) ;
#12886 = CARTESIAN_POINT ( 'NONE',  ( -129.6228709571500417, -24.65952944569305316, 1.056160979905706121 ) ) ;
#12887 = CARTESIAN_POINT ( 'NONE',  ( 15.29947330337541445, 3.316774720514426456, -27.16854002387010780 ) ) ;
#12888 = CARTESIAN_POINT ( 'NONE',  ( -106.5228709571500616, -24.50321055353805733, 9.387540953477520489 ) ) ;
#12889 = ORIENTED_EDGE ( 'NONE', *, *, #17141, .F. ) ;
#12890 = ORIENTED_EDGE ( 'NONE', *, *, #94958, .T. ) ;
#12891 = AXIS2_PLACEMENT_3D ( 'NONE', #68024, #61414, #60914 ) ;
#12892 = ORIENTED_EDGE ( 'NONE', *, *, #17584, .T. ) ;
#12893 = EDGE_CURVE ( 'NONE', #77615, #91001, #67488, .T. ) ;
#12894 = AXIS2_PLACEMENT_3D ( 'NONE', #41685, #72630, #79719 ) ;
#12895 = FACE_OUTER_BOUND ( 'NONE', #65736, .T. ) ;
#12896 = LINE ( 'NONE', #14392, #59501 ) ;
#12897 = EDGE_CURVE ( 'NONE', #53473, #45924, #44482, .T. ) ;
#12898 = CARTESIAN_POINT ( 'NONE',  ( -52.55620429048340014, -23.48786465467241058, 11.44779295918254647 ) ) ;
#12899 = LINE ( 'NONE', #29129, #89115 ) ;
#12900 = AXIS2_PLACEMENT_3D ( 'NONE', #81414, #51964, #50972 ) ;
#12901 = LINE ( 'NONE', #27146, #55045 ) ;
#12902 = DIRECTION ( 'NONE',  ( -0.9903949459893287566, 0.09776975748868974025, 0.09776975748868974025 ) ) ;
#12903 = EDGE_LOOP ( 'NONE', ( #32750, #75800, #38221, #82288 ) ) ;
#12905 = CARTESIAN_POINT ( 'NONE',  ( 7.147005326088517130, -18.03964237587283037, 11.49999999999999645 ) ) ;
#12904 =( REPRESENTATION_RELATIONSHIP ('NONE','NONE', #96270, #60715 ) REPRESENTATION_RELATIONSHIP_WITH_TRANSFORMATION ( #55146 )SHAPE_REPRESENTATION_RELATIONSHIP( ) );
#12907 = CARTESIAN_POINT ( 'NONE',  ( -130.5728709571500303, -23.86862559985391741, 11.02355999656199792 ) ) ;
#12906 =( BOUNDED_SURFACE ( )  B_SPLINE_SURFACE ( 3, 2, ( 
 ( #122, #21941, #39680 ),
 ( #76724, #78230, #7733 ),
 ( #32069, #46806, #31063 ),
 ( #6732, #37686, #22933 ) ),
 .UNSPECIFIED., .F., .F., .T. ) 
 B_SPLINE_SURFACE_WITH_KNOTS ( ( 4, 4 ),
 ( 3, 3 ),
 ( 0.0009756167707891351057, 0.001181474220861217185 ),
 ( 0.000000000000000000, 1.000000000000000000 ),
 .UNSPECIFIED. ) 
 GEOMETRIC_REPRESENTATION_ITEM ( )  RATIONAL_B_SPLINE_SURFACE ( (
 ( 1.000000000000000000, 0.8117984224361689538, 1.000000000000000000),
 ( 1.000000000000000000, 0.7811245729408042848, 1.000000000000000000),
 ( 1.000000000000000000, 0.7458076110977203133, 1.000000000000000000),
 ( 1.000000000000000000, 0.7071067811865505703, 1.000000000000000000) ) ) 
 REPRESENTATION_ITEM ( '' )  SURFACE ( )  );
#12908 = EDGE_CURVE ( 'NONE', #12604, #100201, #73122, .T. ) ;
#12909 = ORIENTED_EDGE ( 'NONE', *, *, #20908, .T. ) ;
#12910 = CARTESIAN_POINT ( 'NONE',  ( 3.559170184186323915, -5.876774720514402972, 18.55412939673608719 ) ) ;
#12911 = DIRECTION ( 'NONE',  ( 0.000000000000000000, 1.000000000000000000, 0.000000000000000000 ) ) ;
#12912 = DIRECTION ( 'NONE',  ( -1.000000000000000000, 0.000000000000000000, 0.000000000000000000 ) ) ;
#12913 = CARTESIAN_POINT ( 'NONE',  ( -120.6228709571500417, -23.47596703998600631, 11.44779298504227683 ) ) ;
#12914 = CARTESIAN_POINT ( 'NONE',  ( 18.62133539762988121, 6.091496293051981148, 11.49999999999998934 ) ) ;
#12915 = CARTESIAN_POINT ( 'NONE',  ( -28.47875734969025885, -5.965225279485572685, -0.08597719988137125791 ) ) ;
#12916 = ORIENTED_EDGE ( 'NONE', *, *, #13517, .F. ) ;
#12917 = CARTESIAN_POINT ( 'NONE',  ( -8.857468890034409625, -19.66367526556523870, 11.49999999999998934 ) ) ;
#12918 = FACE_OUTER_BOUND ( 'NONE', #77671, .T. ) ;
#12919 = FACE_OUTER_BOUND ( 'NONE', #82011, .T. ) ;
#12920 = CARTESIAN_POINT ( 'NONE',  ( -40.65336132159010418, -24.15503026093912453, -0.2815557561904605266 ) ) ;
#12921 = DIRECTION ( 'NONE',  ( -3.773278334453079030E-23, 0.9999999999976377785, 2.173523156925979128E-06 ) ) ;
#12922 = CARTESIAN_POINT ( 'NONE',  ( 14.37299948674089123, 17.95305339730678185, -1.500000000000002220 ) ) ;
#12923 = B_SPLINE_CURVE_WITH_KNOTS ( 'NONE', 3,
 ( #482, #8605, #31436, #54789, #47173, #72014, #73010, #2495, #57299, #26820, #81106, #57785, #81610, #65417, #35441, #50662 ),
 .UNSPECIFIED., .F., .F.,
 ( 4, 2, 2, 2, 2, 2, 2, 4 ),
 ( 2.195984522899320023E-17, 0.0002681372138471760217, 0.0005362744276943301426, 0.001072548855388625374, 0.001340686069235787247, 0.001608823283082948686, 0.001876960496930110342, 0.002145097710777272432 ),
 .UNSPECIFIED. ) ;
#12924 = PERSON_AND_ORGANIZATION_ROLE ( 'creator' ) ;
#12925 = DIRECTION ( 'NONE',  ( -0.03244919754393515293, 0.000000000000000000, 0.9994733861282923959 ) ) ;
#12926 = DIRECTION ( 'NONE',  ( -3.773278334453079618E-23, 0.9999999999976377785, 2.173523156925979975E-06 ) ) ;
#12927 = CARTESIAN_POINT ( 'NONE',  ( -17.16780662754360520, -10.58209718439171176, 11.49999999999999645 ) ) ;
#12928 = CARTESIAN_POINT ( 'NONE',  ( -109.0059884841570153, -25.28814275788919019, 3.784296300591792228 ) ) ;
#12929 = CARTESIAN_POINT ( 'NONE',  ( 30.93860345374796594, -6.475225279485573360, 20.86760796525322093 ) ) ;
#12930 = CARTESIAN_POINT ( 'NONE',  ( -4.141166922167975883, -5.876774720514419847, 20.63520656483649063 ) ) ;
#12931 = DIRECTION ( 'NONE',  ( -0.000000000000000000, -0.000000000000000000, 1.000000000000000000 ) ) ;
#12932 = B_SPLINE_CURVE_WITH_KNOTS ( 'NONE', 3,
 ( #96571, #49928, #27072, #12326, #61017, #75227 ),
 .UNSPECIFIED., .F., .F.,
 ( 4, 2, 4 ),
 ( 1.570755371634052715E-05, 0.001396183895866089488, 0.002776660238015838181 ),
 .UNSPECIFIED. ) ;
#12933 = CARTESIAN_POINT ( 'NONE',  ( -38.52287095715006870, -24.64898659630367206, 1.056161002820819261 ) ) ;
#12934 = ADVANCED_FACE ( 'NONE', ( #42679 ), #4105, .T. ) ;
#12935 = CARTESIAN_POINT ( 'NONE',  ( -5.703961651189128901, -19.02375728206049743, -1.500000000000002220 ) ) ;
#12936 = FACE_OUTER_BOUND ( 'NONE', #67833, .T. ) ;
#12937 = CARTESIAN_POINT ( 'NONE',  ( 16.04393857186779115, -11.51807295290239885, -1.500000000000002220 ) ) ;
#12938 = CARTESIAN_POINT ( 'NONE',  ( -126.6245546122516714, -23.96169478059714564, 10.65365249895716637 ) ) ;
#12939 = CARTESIAN_POINT ( 'NONE',  ( -125.6228709571500843, -24.51254535404253687, 9.355368623467642308 ) ) ;
#12940 = CARTESIAN_POINT ( 'NONE',  ( 2.920210193027767076, -6.376774720514413630, 19.64065332113010243 ) ) ;
#12941 = CARTESIAN_POINT ( 'NONE',  ( 20.35908867758196550, 3.722869731652943770, 11.49999999999999645 ) ) ;
#12942 = CARTESIAN_POINT ( 'NONE',  ( -53.62287095715005592, -24.66019654487199375, 8.947790411086135265 ) ) ;
#12943 = AXIS2_PLACEMENT_3D ( 'NONE', #40515, #54243, #24764 ) ;
#12944 = CARTESIAN_POINT ( 'NONE',  ( -32.30247028140506416, 6.475225279485573360, 27.60502002861223048 ) ) ;
#12946 = EDGE_CURVE ( 'NONE', #41731, #18934, #52914, .T. ) ;
#12945 = CARTESIAN_POINT ( 'NONE',  ( 18.27610663105864219, 13.37729726205769154, 11.49999999999999645 ) ) ;
#12947 = ORIENTED_EDGE ( 'NONE', *, *, #61263, .T. ) ;
#12948 = DIRECTION ( 'NONE',  ( -1.000000000000000000, -0.000000000000000000, -0.000000000000000000 ) ) ;
#12949 = LINE ( 'NONE', #52527, #12748 ) ;
#12950 = AXIS2_PLACEMENT_3D ( 'NONE', #42718, #28462, #5132 ) ;
#12951 = CARTESIAN_POINT ( 'NONE',  ( -63.50465895583770504, -24.15543982623906416, -0.2315651400026651485 ) ) ;
#12952 = DIRECTION ( 'NONE',  ( 0.000000000000000000, 0.000000000000000000, 1.000000000000000000 ) ) ;
#12953 = VECTOR ( 'NONE', #97997, 1000.000000000000000 ) ;
#12954 = ORIENTED_EDGE ( 'NONE', *, *, #33299, .T. ) ;
#12955 = EDGE_LOOP ( 'NONE', ( #95492, #32331, #54564, #48732 ) ) ;
#12956 = CARTESIAN_POINT ( 'NONE',  ( 0.3906119451836247425, -5.876774720514418071, 20.56083401959467594 ) ) ;
#12957 = CARTESIAN_POINT ( 'NONE',  ( -21.74799678179195794, 7.114197580472080951, -1.500000000000002220 ) ) ;
#12958 = CARTESIAN_POINT ( 'NONE',  ( -29.63600644203553003, -24.27415457529449938, 0.1864212292069159782 ) ) ;
#12959 = VECTOR ( 'NONE', #59820, 1000.000000000000000 ) ;
#12960 = CARTESIAN_POINT ( 'NONE',  ( 10.40854797073303395, 18.91789161722374146, -1.500000000000002220 ) ) ;
#12961 = FACE_OUTER_BOUND ( 'NONE', #77280, .T. ) ;
#12962 = CARTESIAN_POINT ( 'NONE',  ( -6.914873625533462409, -5.965225279485572685, 29.95171384920748281 ) ) ;
#12963 = CARTESIAN_POINT ( 'NONE',  ( -3.310667818835141940, 22.29536907041311977, 11.49999999999999645 ) ) ;
#12964 = ORIENTED_EDGE ( 'NONE', *, *, #16778, .F. ) ;
#12965 = AXIS2_PLACEMENT_3D ( 'NONE', #60295, #75483, #31694 ) ;
#12966 = CARTESIAN_POINT ( 'NONE',  ( -27.68651082257922980, -24.78174777341091328, 2.274903344755643708 ) ) ;
#12967 = CARTESIAN_POINT ( 'NONE',  ( 8.537626919312410578, 20.26776412955123163, -1.500000000000002220 ) ) ;
#12968 = EDGE_CURVE ( 'NONE', #64651, #27420, #3118, .T. ) ;
#12970 = CARTESIAN_POINT ( 'NONE',  ( -111.5936661300013952, -23.73766607897671221, -1.055555164236450905 ) ) ;
#12969 = AXIS2_PLACEMENT_3D ( 'NONE', #27882, #34504, #58839 ) ;
#12971 = CARTESIAN_POINT ( 'NONE',  ( -41.86995616089613748, -25.10926067824552632, 4.210710108100564675 ) ) ;
#12972 = ORIENTED_EDGE ( 'NONE', *, *, #24897, .F. ) ;
#12973 = DIRECTION ( 'NONE',  ( 3.773278334444166432E-23, -1.000000000000000000, 0.000000000000000000 ) ) ;
#12974 = CARTESIAN_POINT ( 'NONE',  ( -90.50426386717819582, -24.63419186844611275, 9.035850630976923981 ) ) ;
#12975 = ORIENTED_EDGE ( 'NONE', *, *, #56028, .T. ) ;
#12976 = CARTESIAN_POINT ( 'NONE',  ( 5.202077965628057576, 7.402934475628871785E-15, -2.038091937962834166 ) ) ;
#12977 = ADVANCED_FACE ( 'NONE', ( #48792 ), #34055, .F. ) ;
#12978 = ORIENTED_EDGE ( 'NONE', *, *, #12767, .T. ) ;
#12979 = ORIENTED_EDGE ( 'NONE', *, *, #1246, .F. ) ;
#12980 = CARTESIAN_POINT ( 'NONE',  ( -65.52287095715011844, -24.62226745350437795, 0.9660975649728075210 ) ) ;
#12981 = CARTESIAN_POINT ( 'NONE',  ( -72.22287095715007865, -23.47596703998600631, 11.44779298504227860 ) ) ;
#12982 = CARTESIAN_POINT ( 'NONE',  ( -36.61836639171551866, -23.48783264082477018, -1.443836473390095909 ) ) ;
#12983 = CARTESIAN_POINT ( 'NONE',  ( -0.5597704280004801580, 20.37679164443051505, -1.500000000000002220 ) ) ;
#12984 = EDGE_LOOP ( 'NONE', ( #35258, #46087, #23060, #90654 ) ) ;
#12985 = CARTESIAN_POINT ( 'NONE',  ( -3.108974358974359475, -6.376774720514417183, 20.36458333333334281 ) ) ;
#12986 = EDGE_CURVE ( 'NONE', #73782, #13191, #84465, .T. ) ;
#12987 = CARTESIAN_POINT ( 'NONE',  ( -69.52287095715003318, -24.66019654487199375, 8.947790411086119278 ) ) ;
#12988 = EDGE_CURVE ( 'NONE', #68362, #20017, #26937, .T. ) ;
#12989 = CARTESIAN_POINT ( 'NONE',  ( 282.9764569301858046, 5.356774720514427379, 20.79159422840526616 ) ) ;
#12990 = DIRECTION ( 'NONE',  ( -1.000000000000000000, -3.773278334444167608E-23, -8.201307833595939069E-29 ) ) ;
#12991 = ORIENTED_EDGE ( 'NONE', *, *, #91233, .F. ) ;
#12992 = CARTESIAN_POINT ( 'NONE',  ( 0.000000000000000000, 1.682774720514426114, -1.352392034746782823 ) ) ;
#12993 = CARTESIAN_POINT ( 'NONE',  ( -40.41683116089613748, -25.30532407203700984, 5.082404393492757855 ) ) ;
#12994 = EDGE_CURVE ( 'NONE', #75736, #43450, #56643, .T. ) ;
#12995 = CARTESIAN_POINT ( 'NONE',  ( 20.50115541507891948, 3.495740877612329101, 11.49999999999998934 ) ) ;
#12996 = ORIENTED_EDGE ( 'NONE', *, *, #80716, .T. ) ;
#12998 = ORIENTED_EDGE ( 'NONE', *, *, #67328, .F. ) ;
#12997 = DIRECTION ( 'NONE',  ( 3.773278334444167608E-23, -1.000000000000000000, 0.000000000000000000 ) ) ;
#12999 = CARTESIAN_POINT ( 'NONE',  ( -44.62287095715004881, -23.47596703998600631, 11.44779298504227505 ) ) ;
#13000 = CARTESIAN_POINT ( 'NONE',  ( -33.52287095715008292, -24.33832256527048088, 0.1851278514138557096 ) ) ;
#13001 = ORIENTED_EDGE ( 'NONE', *, *, #88327, .F. ) ;
#13002 = ORIENTED_EDGE ( 'NONE', *, *, #80426, .F. ) ;
#13003 = CARTESIAN_POINT ( 'NONE',  ( -112.5228709571500616, -23.48783264083431988, -1.443836473375253782 ) ) ;
#13004 = CARTESIAN_POINT ( 'NONE',  ( 13.59451591917074431, -3.316774720514426456, -28.23515841827053308 ) ) ;
#13005 = CARTESIAN_POINT ( 'NONE',  ( -35.62287095715005592, -29.50247984919015209, -1.443849546365060466 ) ) ;
#13006 = CARTESIAN_POINT ( 'NONE',  ( -71.04293837957820301, -25.24515098662989487, 5.573254966138859068 ) ) ;
#13007 = EDGE_CURVE ( 'NONE', #78619, #2616, #81223, .T. ) ;
#13009 = EDGE_LOOP ( 'NONE', ( #84987, #68748, #5786, #66804 ) ) ;
#13008 = CARTESIAN_POINT ( 'NONE',  ( -5.973063517705734071, 21.31661749205449041, 11.49999999999999645 ) ) ;
#13010 = CARTESIAN_POINT ( 'NONE',  ( -108.5222109390871594, -23.48783264082478084, -1.443836473390062602 ) ) ;
#13011 = CARTESIAN_POINT ( 'NONE',  ( -13.31036990564671818, -18.29084955798148471, 11.49999999999998934 ) ) ;
#13012 = B_SPLINE_CURVE_WITH_KNOTS ( 'NONE', 3,
 ( #80727, #71618, #56408, #87840 ),
 .UNSPECIFIED., .F., .F.,
 ( 4, 4 ),
 ( 0.000000000000000000, 0.0001000000000000028644 ),
 .UNSPECIFIED. ) ;
#13014 = EDGE_LOOP ( 'NONE', ( #77011, #20334, #67532, #76893 ) ) ;
#13013 = CARTESIAN_POINT ( 'NONE',  ( -99.64934318012689118, -25.30535455722350591, 4.927356316503054501 ) ) ;
#13015 = EDGE_LOOP ( 'NONE', ( #14653, #17224, #83306, #25811 ) ) ;
#13016 = CARTESIAN_POINT ( 'NONE',  ( -81.42380231474228935, -25.31401921878147832, 5.197788989978542773 ) ) ;
#13017 = VECTOR ( 'NONE', #57067, 1000.000000000000000 ) ;
#13018 = EDGE_CURVE ( 'NONE', #79516, #69040, #97926, .T. ) ;
#13019 = EDGE_CURVE ( 'NONE', #39486, #29468, #67504, .T. ) ;
#13020 = CARTESIAN_POINT ( 'NONE',  ( -57.52207137348256794, -23.48786465467241413, 11.44779295918254647 ) ) ;
#13021 = ORIENTED_EDGE ( 'NONE', *, *, #69062, .T. ) ;
#13022 = CARTESIAN_POINT ( 'NONE',  ( -40.01839366089613748, -25.30507950832802777, 5.509688047871486027 ) ) ;
#13023 = CARTESIAN_POINT ( 'NONE',  ( -21.97457344801873447, 3.670769625195870134, -1.500000000000002220 ) ) ;
#13024 = LINE ( 'NONE', #12534, #33831 ) ;
#13025 = EDGE_CURVE ( 'NONE', #88628, #19742, #11863, .T. ) ;
#13026 = ORIENTED_EDGE ( 'NONE', *, *, #64012, .F. ) ;
#13027 = CARTESIAN_POINT ( 'NONE',  ( -74.22287095715006444, -23.47596703998600631, 11.44779298504227860 ) ) ;
#13028 = CARTESIAN_POINT ( 'NONE',  ( -75.52287095715007581, -29.50248528299804818, 1.056150453629038477 ) ) ;
#13029 = CARTESIAN_POINT ( 'NONE',  ( -25.67560423947781700, -24.83136250832902547, 3.472477514678372845 ) ) ;
#13030 = ADVANCED_FACE ( 'NONE', ( #50782 ), #90328, .F. ) ;
#13031 = CARTESIAN_POINT ( 'NONE',  ( -61.64687923781919920, -29.50249039766296022, 3.409318347773680369 ) ) ;
#13032 = DIRECTION ( 'NONE',  ( -0.9952638024365005887, -0.000000000000000000, -0.09721092304694052555 ) ) ;
#13033 = EDGE_CURVE ( 'NONE', #29283, #45187, #21302, .T. ) ;
#13034 = AXIS2_PLACEMENT_3D ( 'NONE', #38203, #147, #82028 ) ;
#13035 = CARTESIAN_POINT ( 'NONE',  ( 13.27039818535887505, -14.28956163997708906, 11.49999999999998934 ) ) ;
#13036 = VECTOR ( 'NONE', #34819, 1000.000000000000000 ) ;
#13037 = CARTESIAN_POINT ( 'NONE',  ( -3.867184171070207288, -21.11305558764578194, 11.49999999999998934 ) ) ;
#13038 = CARTESIAN_POINT ( 'NONE',  ( -2.772696838893043747, -6.376774720514413630, 19.95463486386180207 ) ) ;
#13039 = DIRECTION ( 'NONE',  ( 0.7512896232465891000, -1.109416176496794925E-16, 0.6599726524652351767 ) ) ;
#13040 = FACE_BOUND ( 'NONE', #35195, .T. ) ;
#13041 = CARTESIAN_POINT ( 'NONE',  ( -18.69919181139871966, -13.08804974640095686, -1.500000000000002220 ) ) ;
#13042 = CIRCLE ( 'NONE', #43845, 2.999999999999999112 ) ;
#13043 = APPROVAL_ROLE ( '' ) ;
#13044 = CARTESIAN_POINT ( 'NONE',  ( -96.58459092476410035, -24.66019654487199375, 8.947790411086115725 ) ) ;
#13045 = CARTESIAN_POINT ( 'NONE',  ( -61.52287095715006160, -29.50248528299804818, 1.056150453629034924 ) ) ;
#13046 = CARTESIAN_POINT ( 'NONE',  ( 1.534201407001029027, 19.92515851932037663, 11.49999999999999645 ) ) ;
#13047 = CARTESIAN_POINT ( 'NONE',  ( -89.67764846858844408, -25.06732983082694943, 7.447789526168955732 ) ) ;
#13048 = B_SPLINE_CURVE_WITH_KNOTS ( 'NONE', 3,
 ( #25826, #34445, #97334, #74005 ),
 .UNSPECIFIED., .F., .F.,
 ( 4, 4 ),
 ( 0.000000000000000000, 9.999999999998897304E-05 ),
 .UNSPECIFIED. ) ;
#13049 = CARTESIAN_POINT ( 'NONE',  ( -117.6228709571500559, -24.64965695001469115, 8.947790433994175174 ) ) ;
#13050 = CARTESIAN_POINT ( 'NONE',  ( -48.59340580069252269, -24.15543982623907127, -0.2315651400026527418 ) ) ;
#13051 = ORIENTED_EDGE ( 'NONE', *, *, #56102, .T. ) ;
#13052 = CARTESIAN_POINT ( 'NONE',  ( -26.29825405928423265, -24.66912159618280143, 2.250704355267874046 ) ) ;
#13053 = FACE_OUTER_BOUND ( 'NONE', #30344, .T. ) ;
#13054 = CARTESIAN_POINT ( 'NONE',  ( -14.78470843206283902, -15.91074852019131924, -1.500000000000002220 ) ) ;
#13055 = LINE ( 'NONE', #36903, #7460 ) ;
#13056 = CARTESIAN_POINT ( 'NONE',  ( 4.865394487973861537, 18.91859722749940786, -1.500000000000002220 ) ) ;
#13057 = CARTESIAN_POINT ( 'NONE',  ( -34.52287095715006160, -23.48783264083359867, -1.443836473376372442 ) ) ;
#13058 = B_SPLINE_CURVE_WITH_KNOTS ( 'NONE', 3,
 ( #21673, #51656, #82595, #68375, #44035, #53660 ),
 .UNSPECIFIED., .F., .F.,
 ( 4, 2, 4 ),
 ( 0.000000000000000000, 0.001380901958385399603, 0.002761803916770799207 ),
 .UNSPECIFIED. ) ;
#13059 = VERTEX_POINT ( 'NONE', #43664 ) ;
#13060 = SECURITY_CLASSIFICATION_LEVEL ( 'unclassified' ) ;
#13061 = FACE_OUTER_BOUND ( 'NONE', #37941, .T. ) ;
#13062 = CARTESIAN_POINT ( 'NONE',  ( -40.55620429048340014, -23.47593901973091235, -1.443836447539011525 ) ) ;
#13063 = CARTESIAN_POINT ( 'NONE',  ( 14.40702264168333890, -14.58922348230443689, 11.49999999999999645 ) ) ;
#13064 = CARTESIAN_POINT ( 'NONE',  ( -49.34333941570991300, -25.27829611938825494, 5.818708551465133105 ) ) ;
#13065 = CARTESIAN_POINT ( 'NONE',  ( 32.16024265030974050, -0.3587747205144265483, 14.03360796525321774 ) ) ;
#13066 = VERTEX_POINT ( 'NONE', #14189 ) ;
#13067 = CARTESIAN_POINT ( 'NONE',  ( -110.2093792378191921, -25.29160350784524880, 5.585409231008217290 ) ) ;
#13068 = CARTESIAN_POINT ( 'NONE',  ( -106.6228709571500275, -23.95044443724992789, 10.65354141964649592 ) ) ;
#13069 = DIRECTION ( 'NONE',  ( -3.773278334453079618E-23, 0.9999999999976377785, 2.173523156925979975E-06 ) ) ;
#13070 = CARTESIAN_POINT ( 'NONE',  ( -61.59189125704995860, -25.07259839747099051, 7.371166918563575976 ) ) ;
#13071 = EDGE_LOOP ( 'NONE', ( #1814, #63595, #14502, #50813 ) ) ;
#13072 = B_SPLINE_CURVE_WITH_KNOTS ( 'NONE', 3,
 ( #68605, #90440, #21408, #75208, #20915, #59009, #13800, #14301, #36161, #12304, #45273, #36653, #20409, #89448, #51891, #28534, #67126, #76200, #6696 ),
 .UNSPECIFIED., .F., .F.,
 ( 4, 1, 1, 1, 1, 1, 1, 1, 1, 1, 1, 1, 1, 1, 1, 1, 4 ),
 ( 0.000000000000000000, 0.07834298519370234970, 0.1505633028794191031, 0.2161510566599780803, 0.2756797924514261533, 0.3287070503654628273, 0.3759044348322084228, 0.4173018977400322349, 0.4526927480535833936, 0.5172652917530119465, 0.5812165680623057051, 0.6453218939728029291, 0.7120244933797633680, 0.7801300447160454121, 0.8502182262116654288, 0.9226485217347378809, 1.000000000000000000 ),
 .UNSPECIFIED. ) ;
#13073 = CARTESIAN_POINT ( 'NONE',  ( 5.930937628982182908, -6.376774720514417183, 20.24478033514397524 ) ) ;
#13074 = CARTESIAN_POINT ( 'NONE',  ( -17.35246277222573141, 15.15038115719275424, 11.49999999999999645 ) ) ;
#13075 = CARTESIAN_POINT ( 'NONE',  ( 6.015242202445381992, 21.98585358372262633, 11.49999999999998934 ) ) ;
#13076 = CARTESIAN_POINT ( 'NONE',  ( -121.5228709571500616, -29.50247984919015209, -1.443849546365046699 ) ) ;
#13077 = CARTESIAN_POINT ( 'NONE',  ( -49.21454750704995007, -25.13877828889947352, 7.069183601642414772 ) ) ;
#13078 = CARTESIAN_POINT ( 'NONE',  ( -50.19553086926238450, -25.19638685952546808, 3.303372276271722363 ) ) ;
#13079 = CARTESIAN_POINT ( 'NONE',  ( -64.52287095715006160, -24.65952944569304606, 1.056160979905695463 ) ) ;
#13080 = CARTESIAN_POINT ( 'NONE',  ( -104.5228709571500758, -23.47596703998600631, 11.44779298504228215 ) ) ;
#13081 = VECTOR ( 'NONE', #75394, 1000.000000000000000 ) ;
#13082 = CARTESIAN_POINT ( 'NONE',  ( 19.28182042344761626, 10.37885539243483812, 11.49999999999998934 ) ) ;
#13083 = CARTESIAN_POINT ( 'NONE',  ( -87.52287095715006160, -24.65952944569304606, 1.056160979905700570 ) ) ;
#13084 = EDGE_CURVE ( 'NONE', #61918, #72942, #20803, .T. ) ;
#13085 = CARTESIAN_POINT ( 'NONE',  ( -58.87764846857956513, -25.14083923594470704, 2.947789366366647901 ) ) ;
#13086 = FACE_OUTER_BOUND ( 'NONE', #72828, .T. ) ;
#13087 = DIRECTION ( 'NONE',  ( 3.773278334444166432E-23, -1.000000000000000000, 0.000000000000000000 ) ) ;
#13088 = CARTESIAN_POINT ( 'NONE',  ( -45.52287095715006160, -29.50248789122583659, 2.256150453626215580 ) ) ;
#13089 = ORIENTED_EDGE ( 'NONE', *, *, #42097, .T. ) ;
#13090 = CARTESIAN_POINT ( 'NONE',  ( 6.539103723289373171, -19.38406401830294712, -1.500000000000002220 ) ) ;
#13091 = EDGE_LOOP ( 'NONE', ( #94727, #84265, #51449, #30219, #93372, #40861, #91680, #90239, #54809, #85097, #54465, #48578, #19084, #93480, #19536, #63967, #54546, #96981, #64584, #94228, #16151, #77305, #65964, #23335 ) ) ;
#13092 = VERTEX_POINT ( 'NONE', #28927 ) ;
#13093 = ORIENTED_EDGE ( 'NONE', *, *, #8136, .F. ) ;
#13094 = ORIENTED_EDGE ( 'NONE', *, *, #4458, .T. ) ;
#13095 = CARTESIAN_POINT ( 'NONE',  ( -8.820007276677138464, 21.28423624206370945, 11.49999999999998934 ) ) ;
#13096 = CARTESIAN_POINT ( 'NONE',  ( -61.65508124498639120, -23.48783264082476663, -1.443836473390096575 ) ) ;
#13097 = CARTESIAN_POINT ( 'NONE',  ( 20.02926185082240451, -2.967945350358753398, -1.500000000000002220 ) ) ;
#13098 = ORIENTED_EDGE ( 'NONE', *, *, #80136, .F. ) ;
#13099 = EDGE_CURVE ( 'NONE', #26794, #12874, #34770, .T. ) ;
#13100 = DIRECTION ( 'NONE',  ( 0.03244919754393515293, 0.000000000000000000, -0.9994733861282923959 ) ) ;
#13101 = EDGE_CURVE ( 'NONE', #58179, #17782, #81723, .T. ) ;
#13102 = CARTESIAN_POINT ( 'NONE',  ( 4.621320343559619737, 12.50000000000004974, 2.100000000000000089 ) ) ;
#13103 = EDGE_CURVE ( 'NONE', #56351, #80901, #82711, .T. ) ;
#13105 = CARTESIAN_POINT ( 'NONE',  ( -95.55038110527486594, -24.40034930558991633, 0.3402023900116099009 ) ) ;
#13104 = AXIS2_PLACEMENT_3D ( 'NONE', #75304, #89546, #5802 ) ;
#13106 = CARTESIAN_POINT ( 'NONE',  ( -53.64457961018205623, -23.96169478059712787, 10.65365249895718591 ) ) ;
#13108 = VERTEX_POINT ( 'NONE', #13188 ) ;
#13107 = CARTESIAN_POINT ( 'NONE',  ( 11.86944616785735818, -17.87650476368427732, 11.49999999999999645 ) ) ;
#13109 = CARTESIAN_POINT ( 'NONE',  ( -128.6228709571500417, -23.94994826722516379, -0.6494450866351710872 ) ) ;
#13111 = EDGE_CURVE ( 'NONE', #19685, #40707, #97444, .T. ) ;
#13110 = AXIS2_PLACEMENT_3D ( 'NONE', #60559, #4266, #28099 ) ;
#13112 = ORIENTED_EDGE ( 'NONE', *, *, #47493, .F. ) ;
#13113 = CARTESIAN_POINT ( 'NONE',  ( 16.16129659511371131, 15.28805624652528472, 11.49999999999998934 ) ) ;
#13114 = CARTESIAN_POINT ( 'NONE',  ( 20.27745880512110688, -4.159726151199424571, -1.500000000000002220 ) ) ;
#13115 = VERTEX_POINT ( 'NONE', #37041 ) ;
#13116 = CARTESIAN_POINT ( 'NONE',  ( -2.794871794871791604, -5.876774720514426953, 21.75000000000001066 ) ) ;
#13117 = ORIENTED_EDGE ( 'NONE', *, *, #14952, .F. ) ;
#13118 = CARTESIAN_POINT ( 'NONE',  ( -81.52287095715007581, -23.96127896942134683, -0.6493128930938705246 ) ) ;
#13119 = EDGE_LOOP ( 'NONE', ( #52584, #46403, #95434, #61434 ) ) ;
#13120 = CARTESIAN_POINT ( 'NONE',  ( 19.95448254803897115, -6.385634049875297258, -1.500000000000002220 ) ) ;
#13121 = EDGE_CURVE ( 'NONE', #29369, #8268, #89340, .T. ) ;
#13122 = CARTESIAN_POINT ( 'NONE',  ( 6.821863743248424150, 20.85434273413645911, 11.49999999999999645 ) ) ;
#13123 = CARTESIAN_POINT ( 'NONE',  ( 2.449489742783179214, 4.293056017849825601, 2.499999999999999112 ) ) ;
#13124 = CARTESIAN_POINT ( 'NONE',  ( -8.307687032909205627, 20.95097986170506488, 11.49999999999998934 ) ) ;
#13125 = CARTESIAN_POINT ( 'NONE',  ( 15.04517842881462819, -14.58609674458608829, 11.49999999999998934 ) ) ;
#13126 = CARTESIAN_POINT ( 'NONE',  ( 5.993553214355093139, -6.376774720514417183, 20.20316077874593930 ) ) ;
#13127 = CARTESIAN_POINT ( 'NONE',  ( -52.62287095715005592, -24.66019654487199020, 8.947790411086135265 ) ) ;
#13128 = CARTESIAN_POINT ( 'NONE',  ( 8.071512145086501278, -1.000000000000008882, -3.746884140868835367 ) ) ;
#13130 = EDGE_CURVE ( 'NONE', #26963, #11989, #4611, .T. ) ;
#13129 = ORIENTED_EDGE ( 'NONE', *, *, #86725, .T. ) ;
#13131 = ORIENTED_EDGE ( 'NONE', *, *, #20480, .F. ) ;
#13132 = ORIENTED_EDGE ( 'NONE', *, *, #33105, .F. ) ;
#13133 = FACE_OUTER_BOUND ( 'NONE', #3193, .T. ) ;
#13134 = EDGE_CURVE ( 'NONE', #5411, #62723, #23806, .T. ) ;
#13135 = CARTESIAN_POINT ( 'NONE',  ( -4.253298834618286506, 21.06115358058179154, -1.500000000000002220 ) ) ;
#13136 = CARTESIAN_POINT ( 'NONE',  ( -86.62287095714999907, -24.35013146730203815, 9.818937971375108376 ) ) ;
#13137 = ORIENTED_EDGE ( 'NONE', *, *, #99800, .T. ) ;
#13138 = CARTESIAN_POINT ( 'NONE',  ( -20.28541985502614509, -5.886007371444655689, 11.49999999999998934 ) ) ;
#13139 = CARTESIAN_POINT ( 'NONE',  ( -59.56094173781918499, -25.20074414198133539, 3.409327697718782080 ) ) ;
#13140 = CARTESIAN_POINT ( 'NONE',  ( -64.53961665416358073, -24.51314013834315730, 0.6176544820404094027 ) ) ;
#13141 = CARTESIAN_POINT ( 'NONE',  ( -64.55620429048340725, -23.48783264082478084, -1.443836473390069264 ) ) ;
#13142 = CARTESIAN_POINT ( 'NONE',  ( 8.205893897551582938, -6.475225279485575136, -27.11136772256261196 ) ) ;
#13143 = CARTESIAN_POINT ( 'NONE',  ( -123.5228709571501042, -23.48783264082477018, -1.443836473390084141 ) ) ;
#13144 = CARTESIAN_POINT ( 'NONE',  ( 14.84500176111689207, -16.38379996218902335, -1.500000000000002220 ) ) ;
#13145 = DIRECTION ( 'NONE',  ( 0.000000000000000000, 0.9999999999976377785, 2.173523156925979975E-06 ) ) ;
#13146 = B_SPLINE_CURVE_WITH_KNOTS ( 'NONE', 3,
 ( #17297, #48768, #32021, #47761, #48262, #78676 ),
 .UNSPECIFIED., .F., .F.,
 ( 4, 2, 4 ),
 ( 0.000000000000000000, 0.001380764517854768218, 0.002761529035709536437 ),
 .UNSPECIFIED. ) ;
#13147 = EDGE_CURVE ( 'NONE', #8399, #72949, #20190, .T. ) ;
#13148 = CARTESIAN_POINT ( 'NONE',  ( -2.492070857093962921, -6.376774720514408301, 19.17707164986947177 ) ) ;
#13149 = LINE ( 'NONE', #7048, #8673 ) ;
#13150 = CARTESIAN_POINT ( 'NONE',  ( -0.02075734969026423599, 6.376774720514426953, -0.08597719988137648983 ) ) ;
#13151 = ADVANCED_FACE ( 'NONE', ( #53275 ), #24312, .T. ) ;
#13152 = DIRECTION ( 'NONE',  ( 0.000000000000000000, 0.000000000000000000, 1.000000000000000000 ) ) ;
#13153 = CARTESIAN_POINT ( 'NONE',  ( -19.08929872761019908, -3.557156390981079053, -1.500000000000002220 ) ) ;
#13154 = CARTESIAN_POINT ( 'NONE',  ( 20.90283063341239966, -4.354886778353011856, 11.49999999999998934 ) ) ;
#13155 = CARTESIAN_POINT ( 'NONE',  ( -66.55620429048339304, -23.48783264082478794, -1.443836473390067265 ) ) ;
#13156 = CARTESIAN_POINT ( 'NONE',  ( -49.89149569650673754, -25.11539320716599377, 2.804431449967496714 ) ) ;
#13157 = B_SPLINE_CURVE_WITH_KNOTS ( 'NONE', 3,
 ( #33558, #73621, #49804, #56416 ),
 .UNSPECIFIED., .F., .F.,
 ( 4, 4 ),
 ( 0.000000000000000000, 0.0001000000000000028644 ),
 .UNSPECIFIED. ) ;
#13158 = EDGE_CURVE ( 'NONE', #23352, #34952, #7018, .T. ) ;
#13159 = CARTESIAN_POINT ( 'NONE',  ( -86.52287095715006160, -24.64898659630367916, 1.056161002820827921 ) ) ;
#13160 = CARTESIAN_POINT ( 'NONE',  ( -69.55126625704997423, -25.15208592601422311, 3.076695591939294427 ) ) ;
#13161 = CARTESIAN_POINT ( 'NONE',  ( 5.572475817582897228, 21.94689365879375131, -1.500000000000002220 ) ) ;
#13162 = VERTEX_POINT ( 'NONE', #46663 ) ;
#13163 = CARTESIAN_POINT ( 'NONE',  ( 4.215004826710222474, -5.876774720514426953, 21.34072927444733381 ) ) ;
#13164 = FACE_OUTER_BOUND ( 'NONE', #53955, .T. ) ;
#13165 = CARTESIAN_POINT ( 'NONE',  ( -15.51018552496569392, -12.33189742059753868, 11.49999999999999645 ) ) ;
#13166 = DIRECTION ( 'NONE',  ( 0.000000000000000000, 0.000000000000000000, -1.000000000000000000 ) ) ;
#13167 = CARTESIAN_POINT ( 'NONE',  ( -119.5562042904833930, -24.66019654487200086, 8.947790411086121054 ) ) ;
#13168 = ORIENTED_EDGE ( 'NONE', *, *, #63376, .F. ) ;
#13169 = CARTESIAN_POINT ( 'NONE',  ( -68.55620429048339304, -24.66019654487199020, 8.947790411086131712 ) ) ;
#13170 = CARTESIAN_POINT ( 'NONE',  ( -28.67105337545913812, -25.26026344719939942, 1.897770660017422673 ) ) ;
#13171 = CARTESIAN_POINT ( 'NONE',  ( -100.5528973737291238, -25.17353343482556483, 7.099974540203241702 ) ) ;
#13172 = CARTESIAN_POINT ( 'NONE',  ( -7.466173891270859286, -20.28576548065916541, -1.500000000000002220 ) ) ;
#13173 = CARTESIAN_POINT ( 'NONE',  ( -99.62287095715007013, -24.51283580621365843, 0.6167428607019790343 ) ) ;
#13174 = CARTESIAN_POINT ( 'NONE',  ( -19.24332624019526961, -2.196797614219411443, -1.500000000000002220 ) ) ;
#13175 = CARTESIAN_POINT ( 'NONE',  ( -108.6228709571500559, -29.50247984919015209, -1.443849546365048253 ) ) ;
#13176 = DIRECTION ( 'NONE',  ( -1.000000000000000000, -3.773278334444166432E-23, -8.201307841325785021E-29 ) ) ;
#13177 = CARTESIAN_POINT ( 'NONE',  ( -17.21045110277357182, -9.822940424218707278, 11.49999999999998934 ) ) ;
#13178 = VECTOR ( 'NONE', #55000, 1000.000000000000000 ) ;
#13179 = VERTEX_POINT ( 'NONE', #93824 ) ;
#13180 = CARTESIAN_POINT ( 'NONE',  ( -11.05657426389776354, 17.00066307926000420, 11.49999999999999645 ) ) ;
#13181 = CARTESIAN_POINT ( 'NONE',  ( 11.59154397149680626, 4.779967012825416361, -27.71550087055790712 ) ) ;
#13182 = CYLINDRICAL_SURFACE ( 'NONE', #55472, 10.20000000000000107 ) ;
#13183 = ORIENTED_EDGE ( 'NONE', *, *, #27502, .T. ) ;
#13184 = CARTESIAN_POINT ( 'NONE',  ( -102.5508160338511914, -24.35071581493543746, 9.817618358456027039 ) ) ;
#13185 = CARTESIAN_POINT ( 'NONE',  ( -102.5228709571501042, -23.48783264083375144, -1.443836473376139740 ) ) ;
#13186 = LINE ( 'NONE', #28418, #74283 ) ;
#13187 = PLANE ( 'NONE',  #37574 ) ;
#13188 = CARTESIAN_POINT ( 'NONE',  ( -70.62287095715005592, -25.00158670708909270, 2.256160236439166855 ) ) ;
#13189 = CARTESIAN_POINT ( 'NONE',  ( -0.1815635828756200498, -20.05798930676971636, -1.500000000000002220 ) ) ;
#13190 = CARTESIAN_POINT ( 'NONE',  ( -85.52287095715006160, -24.14321612903117042, -0.2833117244520886868 ) ) ;
#13191 = VERTEX_POINT ( 'NONE', #14694 ) ;
#13192 = B_SPLINE_CURVE_WITH_KNOTS ( 'NONE', 3,
 ( #41528, #34411, #58255, #65391 ),
 .UNSPECIFIED., .F., .F.,
 ( 4, 4 ),
 ( 2.218788294603013803E-07, 9.487457706522013176E-07 ),
 .UNSPECIFIED. ) ;
#13193 = CARTESIAN_POINT ( 'NONE',  ( 4.317061085376620255, -22.40314112565372540, 11.49999999999999645 ) ) ;
#13194 = CARTESIAN_POINT ( 'NONE',  ( -49.84984290111637506, -25.26258851161916397, 4.578680057367619405 ) ) ;
#13195 = DIRECTION ( 'NONE',  ( -3.773278334453079618E-23, 0.9999999999976377785, 2.173523156925979975E-06 ) ) ;
#13196 = CYLINDRICAL_SURFACE ( 'NONE', #19477, 2.249999999999998668 ) ;
#13197 = CARTESIAN_POINT ( 'NONE',  ( -76.52287095715007581, -23.47596703998600631, 11.44779298504228571 ) ) ;
#13198 = PLANE ( 'NONE',  #36527 ) ;
#13199 = AXIS2_PLACEMENT_3D ( 'NONE', #61086, #84900, #71065 ) ;
#13200 = CARTESIAN_POINT ( 'NONE',  ( -5.254942042970298210, 21.81482460008805546, 11.49999999999999645 ) ) ;
#13201 = B_SPLINE_CURVE_WITH_KNOTS ( 'NONE', 3,
 ( #25548, #56517, #87446, #89331, #74107, #97438 ),
 .UNSPECIFIED., .F., .F.,
 ( 4, 2, 4 ),
 ( 6.384118678610533503E-06, 0.001386860460828370214, 0.002767336802978130183 ),
 .UNSPECIFIED. ) ;
#13202 = CARTESIAN_POINT ( 'NONE',  ( 4.712727796232550226, -6.376774720514426953, -25.55789472434992859 ) ) ;
#13203 = EDGE_LOOP ( 'NONE', ( #53550, #67155, #38976, #98236 ) ) ;
#13204 = ADVANCED_FACE ( 'NONE', ( #69986 ), #78082, .F. ) ;
#13205 = CARTESIAN_POINT ( 'NONE',  ( 19.78452974690265975, -4.759501717958375622, -1.500000000000002220 ) ) ;
#13206 = B_SPLINE_CURVE_WITH_KNOTS ( 'NONE', 3,
 ( #17228, #49204, #18725, #80634, #22932, #64442 ),
 .UNSPECIFIED., .F., .F.,
 ( 4, 2, 4 ),
 ( 1.570887131794638196E-05, 0.001396322306279761940, 0.002776935741241577573 ),
 .UNSPECIFIED. ) ;
#13208 = EDGE_CURVE ( 'NONE', #22696, #77182, #9088, .T. ) ;
#13207 = ORIENTED_EDGE ( 'NONE', *, *, #18607, .T. ) ;
#13209 = B_SPLINE_CURVE_WITH_KNOTS ( 'NONE', 3,
 ( #93878, #71557, #55336, #71053 ),
 .UNSPECIFIED., .F., .F.,
 ( 4, 4 ),
 ( 0.000000000000000000, 9.999999999998897304E-05 ),
 .UNSPECIFIED. ) ;
#13210 = CARTESIAN_POINT ( 'NONE',  ( 8.986065527603487979, -21.13286776747340667, -1.500000000000002220 ) ) ;
#13211 = DIRECTION ( 'NONE',  ( 0.000000000000000000, 0.000000000000000000, -1.000000000000000000 ) ) ;
#13212 = ADVANCED_FACE ( 'NONE', ( #47664 ), #30922, .T. ) ;
#13213 = VERTEX_POINT ( 'NONE', #39542 ) ;
#13214 = CARTESIAN_POINT ( 'NONE',  ( -37.62287095715005592, -24.64898659630367206, 1.056161002820819261 ) ) ;
#13215 = ADVANCED_FACE ( 'NONE', ( #53778 ), #89639, .T. ) ;
#13216 = CARTESIAN_POINT ( 'NONE',  ( -77.52287095715006160, -24.64965694238575011, 8.947790433994198267 ) ) ;
#13217 = CARTESIAN_POINT ( 'NONE',  ( -33.62287095715005592, -29.50247984919015209, -1.443849546365062242 ) ) ;
#13219 = EDGE_LOOP ( 'NONE', ( #26439, #89274, #9744, #26729 ) ) ;
#13218 = CARTESIAN_POINT ( 'NONE',  ( -9.505907188867841029, -19.02311915605711690, 11.49999999999999645 ) ) ;
#13220 = EDGE_LOOP ( 'NONE', ( #33542, #21108, #12670, #37227 ) ) ;
#13221 = CARTESIAN_POINT ( 'NONE',  ( -21.91529987491217923, -3.391794311424265018, -1.500000000000002220 ) ) ;
#13222 = CIRCLE ( 'NONE', #91026, 84.76210982660168725 ) ;
#13223 = CARTESIAN_POINT ( 'NONE',  ( -18.82610421443283499, -8.410905081555696938, 11.49999999999998934 ) ) ;
#13224 = ORIENTED_EDGE ( 'NONE', *, *, #74532, .F. ) ;
#13225 = EDGE_LOOP ( 'NONE', ( #99354, #22487, #96559, #98560 ) ) ;
#13226 = CARTESIAN_POINT ( 'NONE',  ( 12.16765770914787304, 5.965225279485572685, -27.57618308014988173 ) ) ;
#13227 = EDGE_CURVE ( 'NONE', #39701, #59550, #90088, .T. ) ;
#13228 = CARTESIAN_POINT ( 'NONE',  ( 3.632573734185411851, -5.876774720514429617, 21.82795992345630509 ) ) ;
#13229 = EDGE_LOOP ( 'NONE', ( #41343, #10517, #36071 ) ) ;
#13230 = ORIENTED_EDGE ( 'NONE', *, *, #78327, .T. ) ;
#13231 = ORIENTED_EDGE ( 'NONE', *, *, #96094, .T. ) ;
#13232 = CARTESIAN_POINT ( 'NONE',  ( -72.52287095715007581, -24.64965694238575011, 8.947790433994200043 ) ) ;
#13233 = LINE ( 'NONE', #20844, #35702 ) ;
#13234 = CARTESIAN_POINT ( 'NONE',  ( 31.79364159983995464, 6.376774720514426953, -11.59305536555894278 ) ) ;
#13235 = CARTESIAN_POINT ( 'NONE',  ( 8.872108392497455753, -18.76566404461018678, -1.500000000000002220 ) ) ;
#13236 = CARTESIAN_POINT ( 'NONE',  ( -14.78470843206283902, -15.91074852019131924, 11.49999999999999645 ) ) ;
#13237 = VERTEX_POINT ( 'NONE', #79598 ) ;
#13238 = CARTESIAN_POINT ( 'NONE',  ( -39.48051905766907765, -25.25935834831543048, 3.941559143231549545 ) ) ;
#13239 = CARTESIAN_POINT ( 'NONE',  ( -98.89667130318164823, -25.24584994799474558, 6.210313119106261048 ) ) ;
#13240 = CARTESIAN_POINT ( 'NONE',  ( -115.5956203964720146, -23.48783264082477018, -1.443836473390087916 ) ) ;
#13241 = CARTESIAN_POINT ( 'NONE',  ( -16.84940295534276800, 14.81145437567392698, -1.500000000000002220 ) ) ;
#13242 = CARTESIAN_POINT ( 'NONE',  ( -51.02503725990638372, -25.26334701977532049, 4.507473529586822458 ) ) ;
#13243 = ORIENTED_EDGE ( 'NONE', *, *, #28984, .T. ) ;
#13244 = CARTESIAN_POINT ( 'NONE',  ( -98.52287095715006160, -23.95044443724992078, 10.65354141964649237 ) ) ;
#13245 = AXIS2_PLACEMENT_3D ( 'NONE', #58883, #43653, #58392 ) ;
#13246 = DIRECTION ( 'NONE',  ( -1.000000000000000000, -0.000000000000000000, -0.000000000000000000 ) ) ;
#13247 = B_SPLINE_CURVE_WITH_KNOTS ( 'NONE', 3,
 ( #16475, #68787, #39823, #61685 ),
 .UNSPECIFIED., .F., .F.,
 ( 4, 4 ),
 ( 0.008354480413380572026, 0.009203042238611652825 ),
 .UNSPECIFIED. ) ;
#13248 = APPROVAL_PERSON_ORGANIZATION ( #84556, #80452, #31270 ) ;
#13249 = ORIENTED_EDGE ( 'NONE', *, *, #61767, .F. ) ;
#13250 = EDGE_LOOP ( 'NONE', ( #30628, #95733, #92875, #87244 ) ) ;
#13251 = B_SPLINE_CURVE_WITH_KNOTS ( 'NONE', 3,
 ( #82430, #20524, #51497, #67230, #28652, #90544 ),
 .UNSPECIFIED., .F., .F.,
 ( 4, 2, 4 ),
 ( 6.391158118952234240E-06, 0.001387004593080775738, 0.002767618028042598960 ),
 .UNSPECIFIED. ) ;
#13252 = CARTESIAN_POINT ( 'NONE',  ( -100.1366382179432293, -25.31290980448949313, 5.258043518187221821 ) ) ;
#13253 = ORIENTED_EDGE ( 'NONE', *, *, #69404, .T. ) ;
#13254 = CARTESIAN_POINT ( 'NONE',  ( -1.825377252022436281, -21.23478267787193730, -1.500000000000002220 ) ) ;
#13255 = ORIENTED_EDGE ( 'NONE', *, *, #23875, .T. ) ;
#13256 = FACE_OUTER_BOUND ( 'NONE', #52916, .T. ) ;
#13257 = CARTESIAN_POINT ( 'NONE',  ( 3.267597511969735802, 21.59432767039258394, 11.49999999999998934 ) ) ;
#13258 = CARTESIAN_POINT ( 'NONE',  ( -124.6228709571500701, -23.47596703998600631, 11.44779298504227860 ) ) ;
#13259 = CARTESIAN_POINT ( 'NONE',  ( -6.316168294299441932, 21.79233575779346310, -1.500000000000002220 ) ) ;
#13260 = CARTESIAN_POINT ( 'NONE',  ( -41.30067620550419605, -25.18430957957208705, 3.692502768481106035 ) ) ;
#13261 = CARTESIAN_POINT ( 'NONE',  ( -28.52287095715007226, -23.32374950011072912, -1.443835813551990643 ) ) ;
#13262 = CARTESIAN_POINT ( 'NONE',  ( 9.922928194174257754, 19.57116106031148561, -1.500000000000002220 ) ) ;
#13263 = CARTESIAN_POINT ( 'NONE',  ( -91.52287095715006160, -29.50247984919015209, -1.443849546365051806 ) ) ;
#13264 = ORIENTED_EDGE ( 'NONE', *, *, #52474, .F. ) ;
#13265 = CARTESIAN_POINT ( 'NONE',  ( -40.41259864834562165, -25.29360172625626291, 5.542179568230306330 ) ) ;
#13266 = ORIENTED_EDGE ( 'NONE', *, *, #90693, .T. ) ;
#13267 = EDGE_CURVE ( 'NONE', #87052, #78138, #54395, .T. ) ;
#13268 = CARTESIAN_POINT ( 'NONE',  ( -84.59178562529271517, -24.15620529776628445, 10.23563542870660292 ) ) ;
#13269 = DIRECTION ( 'NONE',  ( -0.9903949459893287566, 0.09776975748868974025, 0.09776975748868974025 ) ) ;
#13270 = CARTESIAN_POINT ( 'NONE',  ( -0.07959803473139435981, -22.01954088903998397, 0.3010598746230524481 ) ) ;
#13271 = CARTESIAN_POINT ( 'NONE',  ( 6.361473516681357410, -20.28576754457002451, 11.49999999999998934 ) ) ;
#13272 = CARTESIAN_POINT ( 'NONE',  ( -112.6283935189997436, -23.96119346886881729, -0.6495511937831842664 ) ) ;
#13273 = CARTESIAN_POINT ( 'NONE',  ( -26.10669942825130363, -24.75186453689402200, 4.499505972768075956 ) ) ;
#13274 = EDGE_CURVE ( 'NONE', #43699, #64811, #61483, .T. ) ;
#13275 = CARTESIAN_POINT ( 'NONE',  ( -85.51040508421080233, -24.15503026093913519, -0.2815557561904480921 ) ) ;
#13276 = CARTESIAN_POINT ( 'NONE',  ( -33.60984950083365419, -23.73766607897670866, -1.055555164236444909 ) ) ;
#13277 = VECTOR ( 'NONE', #44996, 1000.000000000000000 ) ;
#13278 = B_SPLINE_SURFACE_WITH_KNOTS ( 'NONE', 3, 3, ( 
 ( #55992, #71706, #48874, #49883 ),
 ( #79801, #10298, #42280, #73210 ),
 ( #24514, #55482, #16906, #47869 ),
 ( #34644, #29010, #81310, #51363 ),
 ( #52359, #28512, #65613, #59475 ),
 ( #27025, #50869, #74685, #90416 ),
 ( #58983, #81808, #88929, #5180 ) ),
 .UNSPECIFIED., .F., .F., .F.,
 ( 4, 3, 4 ),
 ( 4, 4 ),
 ( 0.7945040050992235869, 0.8970133687736494554, 0.9995227324480753239 ),
 ( 0.1295269118291874078, 0.1305994346019532237 ),
 .UNSPECIFIED. ) ;
#13279 = CARTESIAN_POINT ( 'NONE',  ( -39.62287095715005592, -24.66019654487199020, 8.947790411086135265 ) ) ;
#13280 = ORIENTED_EDGE ( 'NONE', *, *, #38333, .F. ) ;
#13281 = CARTESIAN_POINT ( 'NONE',  ( 19.11985901488480621, -4.296470200863222288, 11.49999999999999645 ) ) ;
#13282 = CARTESIAN_POINT ( 'NONE',  ( -99.30758664999683560, -25.30967407356133947, 4.614854304310689770 ) ) ;
#13283 = CARTESIAN_POINT ( 'NONE',  ( -70.34543693012690824, -29.50249942614373921, 7.563164501610022405 ) ) ;
#13284 = EDGE_LOOP ( 'NONE', ( #25096, #44203, #54203, #96164 ) ) ;
#13285 = DIRECTION ( 'NONE',  ( 1.000000000000000000, 3.773278334444167608E-23, 8.201307833595939069E-29 ) ) ;
#13286 = CARTESIAN_POINT ( 'NONE',  ( -99.29687923781919778, -25.31439739983868975, 6.149712066081883144 ) ) ;
#13287 = CARTESIAN_POINT ( 'NONE',  ( -62.92287095715006018, -23.47596703998600276, 11.44779298504227683 ) ) ;
#13288 = CARTESIAN_POINT ( 'NONE',  ( -60.52287095715006870, -24.83602698348160587, 1.605859176311257519 ) ) ;
#13289 = CARTESIAN_POINT ( 'NONE',  ( 6.578723047037327909, -18.57437435983987584, 11.49999999999998934 ) ) ;
#13290 = ORIENTED_EDGE ( 'NONE', *, *, #81577, .T. ) ;
#13291 = AXIS2_PLACEMENT_3D ( 'NONE', #90682, #98784, #35898 ) ;
#13292 = AXIS2_PLACEMENT_3D ( 'NONE', #21795, #76089, #5590 ) ;
#13293 = CARTESIAN_POINT ( 'NONE',  ( -5.576923076923074873, -6.376774720514427841, 21.75000000000000711 ) ) ;
#13294 = CARTESIAN_POINT ( 'NONE',  ( 30.60443771307607008, -4.296120514312956828, 26.89827953497908908 ) ) ;
#13295 = SECURITY_CLASSIFICATION_LEVEL ( 'unclassified' ) ;
#13296 = ORIENTED_EDGE ( 'NONE', *, *, #5333, .T. ) ;
#13297 = CARTESIAN_POINT ( 'NONE',  ( -54.52287095715009002, -23.72773821059537269, 11.05748984161097326 ) ) ;
#13298 = CARTESIAN_POINT ( 'NONE',  ( -103.6228709571500985, -23.73934037231757799, 11.05740245334328442 ) ) ;
#13299 = CARTESIAN_POINT ( 'NONE',  ( -120.5228709571500616, -23.47596703998600631, 11.44779298504227860 ) ) ;
#13300 = CARTESIAN_POINT ( 'NONE',  ( -118.5922137762087232, -23.73766607897671221, -1.055555164236448684 ) ) ;
#13301 = CARTESIAN_POINT ( 'NONE',  ( -45.55620429048338593, -24.99156044556202616, 7.747789690856173195 ) ) ;
#13302 = CARTESIAN_POINT ( 'NONE',  ( -69.64006105340874342, -25.24515098634607568, 5.573124385056173580 ) ) ;
#13303 = DIRECTION ( 'NONE',  ( -0.000000000000000000, -1.000000000000000000, -0.000000000000000000 ) ) ;
#13304 = CARTESIAN_POINT ( 'NONE',  ( -0.003041637939312698616, 19.98351707251910980, -1.500000000000002220 ) ) ;
#13305 = CARTESIAN_POINT ( 'NONE',  ( -32.52287095715006160, -24.64898659630528854, 1.056161002820817485 ) ) ;
#13306 = CARTESIAN_POINT ( 'NONE',  ( -0.06514381684952065543, -22.20666209822921999, 9.487281999122094689 ) ) ;
#13307 = ORIENTED_EDGE ( 'NONE', *, *, #11851, .T. ) ;
#13308 = CARTESIAN_POINT ( 'NONE',  ( -29.52287095715004739, -23.86438995984020650, -0.6496299998811901899 ) ) ;
#13309 = CARTESIAN_POINT ( 'NONE',  ( 7.553089130262996775, -6.316227684668181297, -25.84264253713260828 ) ) ;
#13310 = VECTOR ( 'NONE', #79676, 1000.000000000000114 ) ;
#13312 = CARTESIAN_POINT ( 'NONE',  ( -119.6248184345861887, -24.34968618360934656, 0.1864209137778924386 ) ) ;
#13311 = LOCAL_TIME ( 0, 54, 15.00000000000000000, #51380 ) ;
#13313 = CARTESIAN_POINT ( 'NONE',  ( -80.63291137919141249, -24.52399227489127398, 9.353111116836524630 ) ) ;
#13314 = PLANE ( 'NONE',  #93158 ) ;
#13315 = CARTESIAN_POINT ( 'NONE',  ( -81.58822170641624894, -24.34968618360933945, 0.1864209137778954084 ) ) ;
#13316 = CARTESIAN_POINT ( 'NONE',  ( -27.99826093239865443, -24.60093894690410465, 1.648430988000137765 ) ) ;
#13317 = CARTESIAN_POINT ( 'NONE',  ( -1.955883090540335045, -6.376774720514411854, 19.49432735726521315 ) ) ;
#13318 = ORIENTED_EDGE ( 'NONE', *, *, #69941, .T. ) ;
#13319 = CARTESIAN_POINT ( 'NONE',  ( -2.492070857093962921, -5.876774720514409189, 19.17707164986947177 ) ) ;
#13320 = CARTESIAN_POINT ( 'NONE',  ( -127.5554375122736843, -24.34968618360935011, 0.1864209137778923830 ) ) ;
#13321 = VERTEX_POINT ( 'NONE', #48676 ) ;
#13322 = EDGE_CURVE ( 'NONE', #25637, #58202, #18204, .T. ) ;
#13323 = CARTESIAN_POINT ( 'NONE',  ( -18.77428246231291808, -7.638711222589018135, -1.500000000000002220 ) ) ;
#13324 = CARTESIAN_POINT ( 'NONE',  ( -69.92341571696384506, -25.31508615006725194, 4.890982526048191836 ) ) ;
#13325 = DIRECTION ( 'NONE',  ( 0.000000000000000000, -0.7071067811865513475, -0.7071067811865436870 ) ) ;
#13326 = ADVANCED_FACE ( 'NONE', ( #49176 ), #7377, .T. ) ;
#13327 = CARTESIAN_POINT ( 'NONE',  ( -5.366453405989236813, 0.000000000000000000, 0.000000000000000000 ) ) ;
#13328 = EDGE_CURVE ( 'NONE', #66516, #56847, #95328, .T. ) ;
#13329 = VERTEX_POINT ( 'NONE', #79090 ) ;
#13330 = DIRECTION ( 'NONE',  ( 0.000000000000000000, -2.173523156925980399E-06, 0.9999999999976378895 ) ) ;
#13331 = CARTESIAN_POINT ( 'NONE',  ( -105.5228709571500616, -25.00158670708909980, 2.256160236439166411 ) ) ;
#13332 = CARTESIAN_POINT ( 'NONE',  ( 19.70663390988245922, 3.666079223618853966, -1.500000000000002220 ) ) ;
#13333 = EDGE_CURVE ( 'NONE', #11540, #45568, #67372, .T. ) ;
#13334 = CARTESIAN_POINT ( 'NONE',  ( 20.99820426035194032, -0.1900765340283884497, 11.49999999999999645 ) ) ;
#13335 = CARTESIAN_POINT ( 'NONE',  ( -29.24562161810074556, -25.21411260810315369, 5.231851746718979790 ) ) ;
#13336 = CARTESIAN_POINT ( 'NONE',  ( -70.49527151980225881, -24.63419186844611986, 9.035850630976923981 ) ) ;
#13337 = CARTESIAN_POINT ( 'NONE',  ( 0.6065052782250800467, 22.08157775750015617, -1.500000000000002220 ) ) ;
#13338 = EDGE_CURVE ( 'NONE', #50071, #38539, #10585, .T. ) ;
#13339 = B_SPLINE_CURVE_WITH_KNOTS ( 'NONE', 3,
 ( #80219, #87325, #11209, #2112, #64027, #72120 ),
 .UNSPECIFIED., .F., .F.,
 ( 4, 2, 4 ),
 ( 0.000000000000000000, 0.001380764517854763231, 0.002761529035709526462 ),
 .UNSPECIFIED. ) ;
#13340 = CARTESIAN_POINT ( 'NONE',  ( 19.83930831332124001, -5.160774681608516268, 11.49999999999998934 ) ) ;
#13341 = DIRECTION ( 'NONE',  ( -3.773278334453079618E-23, 0.9999999999976377785, 2.173523156925978705E-06 ) ) ;
#13342 = VECTOR ( 'NONE', #73585, 1000.000000000000114 ) ;
#13343 = DIRECTION ( 'NONE',  ( 3.773278334444166432E-23, -1.000000000000000000, 0.000000000000000000 ) ) ;
#13344 = FACE_OUTER_BOUND ( 'NONE', #87300, .T. ) ;
#13345 = ORIENTED_EDGE ( 'NONE', *, *, #35183, .F. ) ;
#13346 = CARTESIAN_POINT ( 'NONE',  ( -87.62287095715004170, -29.50250243563736774, 8.947779886222139822 ) ) ;
#13347 = CARTESIAN_POINT ( 'NONE',  ( -31.48246563699567346, -24.51314013834316086, 0.6176544820404139546 ) ) ;
#13348 = VERTEX_POINT ( 'NONE', #66275 ) ;
#13349 = VERTEX_POINT ( 'NONE', #89590 ) ;
#13350 = CYLINDRICAL_SURFACE ( 'NONE', #89168, 2.500000000000000444 ) ;
#13351 = CARTESIAN_POINT ( 'NONE',  ( -124.9228709571500673, -23.47596703998600987, 11.44779298504228038 ) ) ;
#13353 = ADVANCED_FACE ( 'NONE', ( #35314 ), #82469, .T. ) ;
#13352 = DIRECTION ( 'NONE',  ( 1.000000000000000000, 0.000000000000000000, 0.000000000000000000 ) ) ;
#13354 = CARTESIAN_POINT ( 'NONE',  ( -3.146292006899429783, -20.37002610441940220, -1.500000000000002220 ) ) ;
#13355 = CARTESIAN_POINT ( 'NONE',  ( -20.54952838774410750, 6.582847151591199264, 11.49999999999999645 ) ) ;
#13356 = VERTEX_POINT ( 'NONE', #20071 ) ;
#13357 = CARTESIAN_POINT ( 'NONE',  ( -99.13318064690763265, -25.27852886613005268, 4.186868528538305156 ) ) ;
#13358 = CARTESIAN_POINT ( 'NONE',  ( -55.52287095715006870, -29.50250243563736774, 8.947779886222145151 ) ) ;
#13359 = CARTESIAN_POINT ( 'NONE',  ( 16.92800457317958518, -14.60656088873787262, -1.500000000000002220 ) ) ;
#13360 = CARTESIAN_POINT ( 'NONE',  ( -79.53472330195882023, -25.27874982639352908, 6.603900679166175181 ) ) ;
#13361 = CARTESIAN_POINT ( 'NONE',  ( -65.52287095715006160, -23.48786465467241058, 11.44779295918254647 ) ) ;
#13362 = ORIENTED_EDGE ( 'NONE', *, *, #31110, .F. ) ;
#13363 = B_SPLINE_CURVE_WITH_KNOTS ( 'NONE', 3,
 ( #56758, #87687, #20652, #37395 ),
 .UNSPECIFIED., .F., .F.,
 ( 4, 4 ),
 ( 0.000000000000000000, 0.0001000000000000028644 ),
 .UNSPECIFIED. ) ;
#13364 = CARTESIAN_POINT ( 'NONE',  ( -35.52287095715006870, -24.99132157543083821, 2.256160258750667502 ) ) ;
#13365 = CARTESIAN_POINT ( 'NONE',  ( 30.09341516180546350, -2.682774720514426559, -11.39311774897855933 ) ) ;
#13366 = VECTOR ( 'NONE', #43409, 1000.000000000000114 ) ;
#13367 = CARTESIAN_POINT ( 'NONE',  ( 11.28189403632909915, 17.58240144430209995, -1.500000000000002220 ) ) ;
#13368 = EDGE_LOOP ( 'NONE', ( #57995, #65708, #72116, #67408 ) ) ;
#13370 = ORIENTED_EDGE ( 'NONE', *, *, #39723, .F. ) ;
#13369 = CARTESIAN_POINT ( 'NONE',  ( -86.62359145833659113, -24.65952944569304606, 1.056160979905700126 ) ) ;
#13371 = ORIENTED_EDGE ( 'NONE', *, *, #3410, .F. ) ;
#13372 = CARTESIAN_POINT ( 'NONE',  ( -100.5618449191744475, -23.48786465467241413, 11.44779295918254469 ) ) ;
#13373 = CARTESIAN_POINT ( 'NONE',  ( -20.67868931609407213, -4.308284118179648736, -1.500000000000002220 ) ) ;
#13374 = ORIENTED_EDGE ( 'NONE', *, *, #18950, .T. ) ;
#13375 = CARTESIAN_POINT ( 'NONE',  ( -112.5228709571500616, -24.64965694238408034, 8.947790433994192938 ) ) ;
#13376 = DIRECTION ( 'NONE',  ( -3.773278334453079030E-23, 0.9999999999976377785, 2.173523156925979128E-06 ) ) ;
#13377 = CARTESIAN_POINT ( 'NONE',  ( -81.52287095715006160, -24.65952944569304606, 1.056160979905698794 ) ) ;
#13378 = CARTESIAN_POINT ( 'NONE',  ( -76.51215162630506939, -23.96169478059713143, 10.65365249895718058 ) ) ;
#13379 = CARTESIAN_POINT ( 'NONE',  ( -32.62287095715004881, -23.47593901973091235, -1.443836447539013301 ) ) ;
#13380 = CARTESIAN_POINT ( 'NONE',  ( 21.64095104908334122, -2.195182070091274529, -1.500000000000002220 ) ) ;
#13381 = CARTESIAN_POINT ( 'NONE',  ( -71.64734380851882634, -25.24674250085310234, 5.762066786199834922 ) ) ;
#13383 = ORIENTED_EDGE ( 'NONE', *, *, #77638, .F. ) ;
#13382 = CARTESIAN_POINT ( 'NONE',  ( 10.93216147639808611, 19.43004700418156361, 11.49999999999999645 ) ) ;
#13384 = DIRECTION ( 'NONE',  ( -1.000000000000000000, -0.000000000000000000, -0.000000000000000000 ) ) ;
#13385 = CARTESIAN_POINT ( 'NONE',  ( 15.00349586803797486, 3.316774720514427344, -27.42854230132123305 ) ) ;
#13386 = EDGE_CURVE ( 'NONE', #48183, #1913, #25047, .T. ) ;
#13387 = CARTESIAN_POINT ( 'NONE',  ( -113.6228709571500559, -29.50248528299804818, 1.056150453629043584 ) ) ;
#13388 = VERTEX_POINT ( 'NONE', #74361 ) ;
#13389 = VERTEX_POINT ( 'NONE', #94822 ) ;
#13390 = EDGE_CURVE ( 'NONE', #66516, #6989, #4853, .T. ) ;
#13391 = VECTOR ( 'NONE', #18795, 1000.000000000000000 ) ;
#13392 = ORIENTED_EDGE ( 'NONE', *, *, #51968, .T. ) ;
#13393 = LOCAL_TIME ( 0, 54, 15.00000000000000000, #42545 ) ;
#13394 = CARTESIAN_POINT ( 'NONE',  ( -10.24059822343757808, -5.876774720514426953, 17.91871304725684766 ) ) ;
#13395 = DIRECTION ( 'NONE',  ( 0.000000000000000000, -1.000000000000000000, 0.000000000000000000 ) ) ;
#13396 = LINE ( 'NONE', #75794, #10611 ) ;
#13397 = PLANE ( 'NONE',  #87522 ) ;
#13399 = CARTESIAN_POINT ( 'NONE',  ( -13.40542139710017899, 13.98966777563825481, -1.500000000000002220 ) ) ;
#13398 = AXIS2_PLACEMENT_3D ( 'NONE', #74101, #97431, #27918 ) ;
#13400 = EDGE_CURVE ( 'NONE', #24140, #79832, #55784, .T. ) ;
#13401 = CARTESIAN_POINT ( 'NONE',  ( -45.92287095715005307, -23.47596703998600276, 11.44779298504227683 ) ) ;
#13402 = ORIENTED_EDGE ( 'NONE', *, *, #32383, .T. ) ;
#13403 = CARTESIAN_POINT ( 'NONE',  ( 15.36829964806744364, -11.83880051060199712, 11.49999999999999645 ) ) ;
#13404 = DIRECTION ( 'NONE',  ( -0.9762960071199348056, -0.2164396139380966033, -3.469446951953617147E-16 ) ) ;
#13405 = VECTOR ( 'NONE', #41489, 1000.000000000000114 ) ;
#13406 = EDGE_CURVE ( 'NONE', #47188, #49194, #86708, .T. ) ;
#13407 = ORIENTED_EDGE ( 'NONE', *, *, #11723, .F. ) ;
#13408 = CARTESIAN_POINT ( 'NONE',  ( 2.949406532984364393, -5.876774720514410077, 19.42899254576129664 ) ) ;
#13409 = DIRECTION ( 'NONE',  ( -3.773278334453079618E-23, 0.9999999999976377785, 2.173523156925979552E-06 ) ) ;
#13410 = DIRECTION ( 'NONE',  ( 0.000000000000000000, 1.000000000000000000, 0.000000000000000000 ) ) ;
#13411 = CARTESIAN_POINT ( 'NONE',  ( -87.62287095714999907, -24.33927499327853639, 9.819080762295817166 ) ) ;
#13412 = CARTESIAN_POINT ( 'NONE',  ( -17.52035102510334141, -8.822347199899118309, -1.500000000000002220 ) ) ;
#13413 = B_SPLINE_SURFACE_WITH_KNOTS ( 'NONE', 3, 3, ( 
 ( #14253, #93378, #61954, #8158 ),
 ( #99978, #53342, #53841, #54842 ),
 ( #70554, #92880, #6651, #23359 ),
 ( #85268, #46216, #37607, #77150 ),
 ( #83771, #70053, #539, #31487 ),
 ( #54343, #52835, #15760, #62450 ),
 ( #30487, #84271, #84772, #85783 ),
 ( #1050, #46725, #68556, #16265 ),
 ( #78145, #7654, #99490, #38603 ),
 ( #29985, #22355, #45722, #76645 ),
 ( #7146, #38098, #69052, #61455 ),
 ( #92382, #15260, #69562, #9150 ),
 ( #18272, #64481, #72077, #47728 ),
 ( #71571, #34002, #80172, #93889 ),
 ( #40111, #33003, #2064, #49244 ),
 ( #10663, #41624, #17268, #94391 ),
 ( #55849, #32497, #86278, #48231 ),
 ( #49742, #55346, #78644, #80669 ),
 ( #95395, #71067, #48741, #87276 ),
 ( #87789, #17777, #79661, #11156 ),
 ( #10161, #86777, #79162, #1556 ),
 ( #42132, #2557, #63469, #64978 ),
 ( #73072, #94888, #24873, #9661 ),
 ( #40616, #63978, #25885, #25380 ),
 ( #33494, #56357, #3556, #56857 ) ),
 .UNSPECIFIED., .F., .F., .F.,
 ( 4, 3, 3, 3, 3, 3, 3, 3, 4 ),
 ( 4, 4 ),
 ( 0.0004766824943081664212, 0.1253574377757289138, 0.1877978154164393065, 0.2502381930571496715, 0.4999997036199911871, 0.7497612141828327026, 0.8122015918235430121, 0.8746419694642534326, 0.9995227247456741626 ),
 ( 0.0001139708429040862454, 0.005838217335517809428 ),
 .UNSPECIFIED. ) ;
#13414 = CARTESIAN_POINT ( 'NONE',  ( -37.55620429048340725, -24.64898659630528144, 1.056161002820821260 ) ) ;
#13415 = EDGE_LOOP ( 'NONE', ( #21097, #26239, #98868, #91472 ) ) ;
#13416 = CARTESIAN_POINT ( 'NONE',  ( 20.98156868870745484, 4.911575462371418510, 11.49999999999998934 ) ) ;
#13417 = CARTESIAN_POINT ( 'NONE',  ( -33.56120774392356054, -23.73791477778911130, 11.05961554403171299 ) ) ;
#13418 = LINE ( 'NONE', #83937, #70783 ) ;
#13419 = DIRECTION ( 'NONE',  ( 0.000000000000000000, -1.155373159085149695E-17, 1.000000000000000000 ) ) ;
#13420 = CARTESIAN_POINT ( 'NONE',  ( 26.73860345374794178, -1.477225279485574028, 19.84760796525321780 ) ) ;
#13421 = CARTESIAN_POINT ( 'NONE',  ( 20.85440106035463970, 9.703512019146668166, -1.500000000000002220 ) ) ;
#13422 = CC_DESIGN_PERSON_AND_ORGANIZATION_ASSIGNMENT ( #5694, #36646, ( #91188 ) ) ;
#13423 = CIRCLE ( 'NONE', #39363, 4.300000000000000711 ) ;
#13424 = APPROVAL_STATUS ( 'not_yet_approved' ) ;
#13425 = CARTESIAN_POINT ( 'NONE',  ( -101.7776484685884100, -25.27307239909451653, 3.986250617436227550 ) ) ;
#13426 = DIRECTION ( 'NONE',  ( -3.773278334453079618E-23, 0.9999999999976377785, 2.173523156925979975E-06 ) ) ;
#13427 = CARTESIAN_POINT ( 'NONE',  ( -17.50950832565593984, 9.922426906265528146, 11.49999999999999645 ) ) ;
#13428 = CYLINDRICAL_SURFACE ( 'NONE', #52763, 0.2999999999999981570 ) ;
#13429 = CARTESIAN_POINT ( 'NONE',  ( -32.57080280157106955, -23.48786465467240347, 11.44779295918255535 ) ) ;
#13430 = PRODUCT_DEFINITION_SHAPE ( 'NONE', 'NONE',  #94066 ) ;
#13431 = LINE ( 'NONE', #35789, #37638 ) ;
#13432 = CARTESIAN_POINT ( 'NONE',  ( -29.55620429048338949, -23.40360120717180692, 11.44779300713762638 ) ) ;
#13433 = CARTESIAN_POINT ( 'NONE',  ( -111.0533842133887390, -25.18425641804806503, 3.566050094442076102 ) ) ;
#13434 = CARTESIAN_POINT ( 'NONE',  ( 3.337697395173636394, -19.57427954046807983, -1.500000000000002220 ) ) ;
#13435 = AXIS2_PLACEMENT_3D ( 'NONE', #60454, #21850, #90384 ) ;
#13436 = DIRECTION ( 'NONE',  ( 0.000000000000000000, -1.000000000000000000, -1.020425574104004246E-16 ) ) ;
#13437 = CARTESIAN_POINT ( 'NONE',  ( -3.970774856468506364, -19.35638658347046714, -1.500000000000002220 ) ) ;
#13438 = CYLINDRICAL_SURFACE ( 'NONE', #42691, 0.8160000000000007248 ) ;
#13439 = CIRCLE ( 'NONE', #42670, 6.594667762285751245 ) ;
#13440 = DESIGN_CONTEXT ( 'detailed design', #94551, 'design' ) ;
#13441 = CARTESIAN_POINT ( 'NONE',  ( -0.9540731552372990754, -6.376774720514411854, 19.74568812963596542 ) ) ;
#13442 = CARTESIAN_POINT ( 'NONE',  ( -28.98875734969026041, 5.965225279485572685, 17.86602280011862476 ) ) ;
#13443 = CARTESIAN_POINT ( 'NONE',  ( 7.508984785159893427, -19.29828013722326929, 11.49999999999999645 ) ) ;
#13444 = CARTESIAN_POINT ( 'NONE',  ( 0.6000000000000007550, 0.000000000000000000, 21.89999999999999858 ) ) ;
#13445 = LINE ( 'NONE', #66775, #12418 ) ;
#13446 = DIRECTION ( 'NONE',  ( 0.000000000000000000, -0.9999999999976377785, -2.173523156925979975E-06 ) ) ;
#13447 = CARTESIAN_POINT ( 'NONE',  ( 9.518656604726816184, -20.62229310799655124, 11.49999999999999645 ) ) ;
#13448 = VERTEX_POINT ( 'NONE', #37796 ) ;
#13449 = CARTESIAN_POINT ( 'NONE',  ( -0.2200237740140755516, -5.876774720514409189, 19.17724329193115551 ) ) ;
#13450 = CARTESIAN_POINT ( 'NONE',  ( 30.61220459279984496, 3.931892516571728446, 27.21038724104498385 ) ) ;
#13451 = EDGE_CURVE ( 'NONE', #92742, #58910, #99015, .T. ) ;
#13452 = CARTESIAN_POINT ( 'NONE',  ( -63.63170861370627307, -24.34968618360933590, 0.1864209137778804204 ) ) ;
#13453 = CARTESIAN_POINT ( 'NONE',  ( 32.66876533700883556, -5.965225279485572685, -12.58926540598386445 ) ) ;
#13454 = VERTEX_POINT ( 'NONE', #82960 ) ;
#13455 = ORIENTED_EDGE ( 'NONE', *, *, #19438, .T. ) ;
#13456 = CIRCLE ( 'NONE', #88010, 130.7884398600581335 ) ;
#13457 = LINE ( 'NONE', #65295, #40425 ) ;
#13458 = CARTESIAN_POINT ( 'NONE',  ( -22.79553223295561892, 1.966428799096173075, -1.500000000000002220 ) ) ;
#13459 = PLANE ( 'NONE',  #43837 ) ;
#13460 = CARTESIAN_POINT ( 'NONE',  ( 21.36531308999010648, 3.172564587314818052, -1.500000000000002220 ) ) ;
#13461 = CARTESIAN_POINT ( 'NONE',  ( -123.5204192411642339, -24.15543982623907482, -0.2315651400026561002 ) ) ;
#13462 = CARTESIAN_POINT ( 'NONE',  ( -65.52287095715006160, -23.48783264082476308, -1.443836473390092578 ) ) ;
#13463 = CC_DESIGN_SECURITY_CLASSIFICATION ( #19911, ( #100430 ) ) ;
#13464 = EDGE_CURVE ( 'NONE', #45390, #74792, #81922, .T. ) ;
#13465 = CARTESIAN_POINT ( 'NONE',  ( -1.797493081057526032, -22.44471576765463183, 11.49999999999999645 ) ) ;
#13466 = VERTEX_POINT ( 'NONE', #84460 ) ;
#13467 = CARTESIAN_POINT ( 'NONE',  ( -43.52287095715008292, -23.73907113217667586, -1.053371485781309680 ) ) ;
#13468 = CARTESIAN_POINT ( 'NONE',  ( 20.22059317821533853, 8.664326447042464352, 11.49999999999998934 ) ) ;
#13469 = EDGE_CURVE ( 'NONE', #80664, #44878, #83460, .T. ) ;
#13470 = CARTESIAN_POINT ( 'NONE',  ( -105.5960308574089623, -23.85049219812686871, 10.88485053497526955 ) ) ;
#13471 = CARTESIAN_POINT ( 'NONE',  ( -28.66268959117890347, -24.79700224147869747, 7.176257715543974847 ) ) ;
#13472 = VECTOR ( 'NONE', #23897, 1000.000000000000000 ) ;
#13473 = EDGE_LOOP ( 'NONE', ( #56327, #57465, #34834, #28080 ) ) ;
#13474 = CARTESIAN_POINT ( 'NONE',  ( 4.948119756536996761, -6.376774720514410077, 19.52858994054604125 ) ) ;
#13475 = CARTESIAN_POINT ( 'NONE',  ( -90.55338340485998572, -24.15602025860896163, 10.28564288303535434 ) ) ;
#13476 = EDGE_LOOP ( 'NONE', ( #24794, #32677, #46905, #86541 ) ) ;
#13477 = DIRECTION ( 'NONE',  ( -3.773278334444167608E-23, 1.000000000000000000, 0.000000000000000000 ) ) ;
#13478 = ORIENTED_EDGE ( 'NONE', *, *, #37125, .T. ) ;
#13479 = AXIS2_PLACEMENT_3D ( 'NONE', #65230, #80921, #35257 ) ;
#13480 = ORIENTED_EDGE ( 'NONE', *, *, #72614, .F. ) ;
#13481 = DIRECTION ( 'NONE',  ( 0.000000000000000000, 0.000000000000000000, -1.000000000000000000 ) ) ;
#13482 = LINE ( 'NONE', #90119, #53531 ) ;
#13484 = EDGE_CURVE ( 'NONE', #13594, #88430, #91572, .T. ) ;
#13483 = CARTESIAN_POINT ( 'NONE',  ( 31.59111626279633711, 0.3587747205144265483, 16.27760796525321751 ) ) ;
#13485 = CARTESIAN_POINT ( 'NONE',  ( 11.41020680648336771, 16.95828056793917682, -1.500000000000002220 ) ) ;
#13486 = ORIENTED_EDGE ( 'NONE', *, *, #57280, .T. ) ;
#13487 = DIRECTION ( 'NONE',  ( -0.000000000000000000, 1.000000000000000000, -0.000000000000000000 ) ) ;
#13488 = CARTESIAN_POINT ( 'NONE',  ( -99.52287095715006160, -23.48786465467241769, 11.44779295918254114 ) ) ;
#13489 = FACE_OUTER_BOUND ( 'NONE', #24499, .T. ) ;
#13490 = CARTESIAN_POINT ( 'NONE',  ( -88.62287095715008434, -23.73934037231757443, 11.05740245334328797 ) ) ;
#13491 = ORIENTED_EDGE ( 'NONE', *, *, #49916, .F. ) ;
#13492 = CARTESIAN_POINT ( 'NONE',  ( -123.5228709571500474, -23.47593901973090524, -1.443836447538996204 ) ) ;
#13493 = DIRECTION ( 'NONE',  ( -0.000000000000000000, 1.000000000000000000, -0.000000000000000000 ) ) ;
#13494 = CARTESIAN_POINT ( 'NONE',  ( 20.60118427460899326, -2.865472796819775958, -1.500000000000002220 ) ) ;
#13495 = ORIENTED_EDGE ( 'NONE', *, *, #88785, .F. ) ;
#13497 = EDGE_LOOP ( 'NONE', ( #40420, #39537, #96387, #61781, #45947 ) ) ;
#13496 = CARTESIAN_POINT ( 'NONE',  ( -39.83231326723547028, -25.30536239359308226, 4.922453132992008484 ) ) ;
#13498 = B_SPLINE_SURFACE_WITH_KNOTS ( 'NONE', 3, 3, ( 
 ( #81933, #64749, #97164, #27154 ),
 ( #41892, #19030, #33256, #71835 ),
 ( #2327, #3337, #80938, #11425 ),
 ( #66237, #65738, #64239, #80438 ),
 ( #50005, #11923, #95163, #56622 ),
 ( #4323, #18033, #73820, #49001 ),
 ( #10420, #26148, #10927, #57119 ) ),
 .UNSPECIFIED., .F., .F., .F.,
 ( 4, 3, 4 ),
 ( 4, 4 ),
 ( 0.7945040050992240310, 0.8970133687736498995, 0.9995227324480757680 ),
 ( 0.2895675803802711390, 0.2907139885458068229 ),
 .UNSPECIFIED. ) ;
#13499 = CARTESIAN_POINT ( 'NONE',  ( 30.49880699021233710, -4.793320133135864580, 19.84760796525321425 ) ) ;
#13500 = ORIENTED_EDGE ( 'NONE', *, *, #35183, .T. ) ;
#13501 = ORIENTED_EDGE ( 'NONE', *, *, #24696, .F. ) ;
#13502 = PLANE ( 'NONE',  #64100 ) ;
#13503 = CARTESIAN_POINT ( 'NONE',  ( -120.9228709571500104, -23.47593901973090524, -1.443836447538996426 ) ) ;
#13504 = CARTESIAN_POINT ( 'NONE',  ( -55.52287095715005449, -23.48783264082477018, -1.443836473390094577 ) ) ;
#13505 = CARTESIAN_POINT ( 'NONE',  ( -53.55620429048340014, -23.48783264082478084, -1.443836473390071040 ) ) ;
#13507 = VERTEX_POINT ( 'NONE', #53535 ) ;
#13506 = CARTESIAN_POINT ( 'NONE',  ( -5.843409716339609261, -21.38298466452703650, 11.49999999999999645 ) ) ;
#13508 = CARTESIAN_POINT ( 'NONE',  ( -8.160000000000000142, -10.15233964170348457, 0.003711184059992174607 ) ) ;
#13509 = AXIS2_PLACEMENT_3D ( 'NONE', #10403, #55224, #26638 ) ;
#13510 = CARTESIAN_POINT ( 'NONE',  ( -9.675873947287982446, 20.46574270456686406, 11.49999999999998934 ) ) ;
#13512 = ORIENTED_EDGE ( 'NONE', *, *, #5196, .T. ) ;
#13511 = CARTESIAN_POINT ( 'NONE',  ( -99.60210373809772477, -25.30549553519965045, 4.950166919727378989 ) ) ;
#13513 = EDGE_CURVE ( 'NONE', #47314, #10925, #61648, .T. ) ;
#13514 = VECTOR ( 'NONE', #80851, 1000.000000000000000 ) ;
#13515 = ORIENTED_EDGE ( 'NONE', *, *, #63310, .T. ) ;
#13516 = CARTESIAN_POINT ( 'NONE',  ( -69.55620429048339304, -23.47593901973091235, -1.443836447539006196 ) ) ;
#13517 = EDGE_CURVE ( 'NONE', #78274, #53278, #45418, .T. ) ;
#13518 = B_SPLINE_CURVE_WITH_KNOTS ( 'NONE', 3,
 ( #41120, #95892, #16758, #26387 ),
 .UNSPECIFIED., .F., .F.,
 ( 4, 4 ),
 ( 0.000000000000000000, 1.000000000000000000 ),
 .UNSPECIFIED. ) ;
#13519 = CARTESIAN_POINT ( 'NONE',  ( -19.81368827760683260, -3.497637702615509880, -1.500000000000002220 ) ) ;
#13520 = CARTESIAN_POINT ( 'NONE',  ( -57.64348235002147902, -23.96169478059713143, 10.65365249895718058 ) ) ;
#13521 = VERTEX_POINT ( 'NONE', #75346 ) ;
#13522 = CARTESIAN_POINT ( 'NONE',  ( -40.41373532093560073, -25.29345418465820572, 5.542204922786879706 ) ) ;
#13523 = CARTESIAN_POINT ( 'NONE',  ( -21.31523168734759466, -6.469442287714795015, -1.500000000000002220 ) ) ;
#13524 = VERTEX_POINT ( 'NONE', #98185 ) ;
#13525 = CARTESIAN_POINT ( 'NONE',  ( 0.7603455638109648529, 10.87344814783205038, 0.000000000000000000 ) ) ;
#13526 = CARTESIAN_POINT ( 'NONE',  ( -89.62287095715008434, -24.33927499327854704, 9.819080762295818943 ) ) ;
#13527 = CARTESIAN_POINT ( 'NONE',  ( -26.02028971856659112, -24.71824093682183587, 2.619536031526803033 ) ) ;
#13528 = DIRECTION ( 'NONE',  ( -1.000000000000000000, 0.000000000000000000, 0.000000000000000000 ) ) ;
#13529 = CARTESIAN_POINT ( 'NONE',  ( -43.92287095715004597, -23.47596703998600276, 11.44779298504227683 ) ) ;
#13530 = AXIS2_PLACEMENT_3D ( 'NONE', #48361, #64104, #16388 ) ;
#13531 = CARTESIAN_POINT ( 'NONE',  ( -7.634514033349506512, -17.95459398628807435, -1.500000000000002220 ) ) ;
#13532 = CARTESIAN_POINT ( 'NONE',  ( -17.67684169981329845, 12.20363403927300183, 11.49999999999998934 ) ) ;
#13533 = CARTESIAN_POINT ( 'NONE',  ( -2.786875287040666560, -6.376774720514417183, 20.09505574050193388 ) ) ;
#13534 = CARTESIAN_POINT ( 'NONE',  ( -110.5228709571500616, -29.50248789122583659, 2.256150453626215580 ) ) ;
#13535 = FACE_OUTER_BOUND ( 'NONE', #48490, .T. ) ;
#13536 = CARTESIAN_POINT ( 'NONE',  ( -21.14637036216210575, 8.611126525438130841, -1.500000000000002220 ) ) ;
#13537 = ADVANCED_FACE ( 'NONE', ( #44925 ), #54032, .T. ) ;
#13538 = EDGE_CURVE ( 'NONE', #66877, #89773, #46910, .T. ) ;
#13539 = VECTOR ( 'NONE', #72475, 1000.000000000000000 ) ;
#13540 = MECHANICAL_CONTEXT ( 'NONE', #39445, 'mechanical' ) ;
#13541 = CARTESIAN_POINT ( 'NONE',  ( -96.54561769259652237, -24.66019654487199375, 8.947790411086115725 ) ) ;
#13542 = CARTESIAN_POINT ( 'NONE',  ( -29.55620429048340725, -24.56818223648220112, 1.056161313644432997 ) ) ;
#13543 = CARTESIAN_POINT ( 'NONE',  ( -18.20579941527595480, -8.200869797747142087, 11.49999999999999645 ) ) ;
#13544 = LINE ( 'NONE', #44514, #38710 ) ;
#13545 = AXIS2_PLACEMENT_3D ( 'NONE', #49264, #41643, #35526 ) ;
#13546 = CARTESIAN_POINT ( 'NONE',  ( -57.55620429048338593, -24.64898659630529210, 1.056161002820822814 ) ) ;
#13547 = CARTESIAN_POINT ( 'NONE',  ( -46.62287095715004881, -29.50250786944525672, 11.44777988621624054 ) ) ;
#13548 = ORIENTED_EDGE ( 'NONE', *, *, #14761, .F. ) ;
#13549 = CARTESIAN_POINT ( 'NONE',  ( -89.62287095715004170, -24.64898659630529210, 1.056161002820827921 ) ) ;
#13550 = DIRECTION ( 'NONE',  ( 0.000000000000000000, -1.000000000000000000, 0.000000000000000000 ) ) ;
#13551 = CARTESIAN_POINT ( 'NONE',  ( -21.53672441135761773, -2.854535511010750870, 11.49999999999998934 ) ) ;
#13552 = EDGE_CURVE ( 'NONE', #99423, #21858, #10613, .T. ) ;
#13553 = FACE_OUTER_BOUND ( 'NONE', #4163, .T. ) ;
#13554 = CARTESIAN_POINT ( 'NONE',  ( -0.6043519431218743465, -19.59835197619436187, -1.500000000000002220 ) ) ;
#13555 = EDGE_CURVE ( 'NONE', #33103, #18367, #7330, .T. ) ;
#13556 = CARTESIAN_POINT ( 'NONE',  ( -99.29844387660956784, -25.25464675839173978, 6.219202189682646598 ) ) ;
#13557 = B_SPLINE_CURVE_WITH_KNOTS ( 'NONE', 3,
 ( #4690, #12280, #35640, #3205, #34146, #65112 ),
 .UNSPECIFIED., .F., .F.,
 ( 4, 2, 4 ),
 ( 6.384118678624473124E-06, 0.001386860460828385610, 0.002767336802978146663 ),
 .UNSPECIFIED. ) ;
#13558 = ORIENTED_EDGE ( 'NONE', *, *, #95707, .T. ) ;
#13559 = EDGE_CURVE ( 'NONE', #85635, #62904, #88083, .T. ) ;
#13560 = LINE ( 'NONE', #67871, #33769 ) ;
#13561 = CARTESIAN_POINT ( 'NONE',  ( 3.769931535195356620, -6.376774720514429617, 21.83933825178638699 ) ) ;
#13562 = CARTESIAN_POINT ( 'NONE',  ( -20.41219973434085944, 2.133827299322149429, 11.49999999999999645 ) ) ;
#13563 = DIRECTION ( 'NONE',  ( 0.000000000000000000, 0.000000000000000000, -1.000000000000000000 ) ) ;
#13564 = CARTESIAN_POINT ( 'NONE',  ( -113.6228709571500417, -24.66019654487199730, 8.947790411086121054 ) ) ;
#13565 = ORIENTED_EDGE ( 'NONE', *, *, #64222, .T. ) ;
#13566 = CARTESIAN_POINT ( 'NONE',  ( -109.3584176993576591, -25.27948031066536672, 4.206202526585778756 ) ) ;
#13567 = CARTESIAN_POINT ( 'NONE',  ( -39.81688933929658702, -25.18430914852639191, 3.494186188583478625 ) ) ;
#13568 = FACE_OUTER_BOUND ( 'NONE', #29101, .T. ) ;
#13569 = EDGE_CURVE ( 'NONE', #95644, #24081, #23901, .T. ) ;
#13570 = LINE ( 'NONE', #75464, #59797 ) ;
#13571 = VECTOR ( 'NONE', #70126, 1000.000000000000000 ) ;
#13572 = VERTEX_POINT ( 'NONE', #59652 ) ;
#13573 = CARTESIAN_POINT ( 'NONE',  ( -100.6228709571500559, -24.99156045073393173, 7.747789690856161648 ) ) ;
#13574 = CARTESIAN_POINT ( 'NONE',  ( 0.2859537766682072601, -23.01552763051285666, 11.49999999999999645 ) ) ;
#13575 = CARTESIAN_POINT ( 'NONE',  ( 9.298244000614250382, 20.81247324795305431, 11.49999999999998934 ) ) ;
#13576 = CARTESIAN_POINT ( 'NONE',  ( 3.787259615384621636, -5.876774720514405637, 18.51923076923076650 ) ) ;
#13577 = VECTOR ( 'NONE', #28211, 1000.000000000000114 ) ;
#13578 = CARTESIAN_POINT ( 'NONE',  ( 29.77147767949874435, 6.376774720514426953, 26.15915692125051706 ) ) ;
#13579 = CARTESIAN_POINT ( 'NONE',  ( -120.5228709571500616, -24.82576562948882071, 8.398263436605679644 ) ) ;
#13580 = CARTESIAN_POINT ( 'NONE',  ( -40.52287095715004028, -24.52323809116981579, 9.355190652339427260 ) ) ;
#13581 = LINE ( 'NONE', #17089, #65969 ) ;
#13582 = CARTESIAN_POINT ( 'NONE',  ( 6.492371748702247203, -20.92784845389783399, -1.500000000000002220 ) ) ;
#13583 = EDGE_CURVE ( 'NONE', #55233, #90203, #78341, .T. ) ;
#13584 = FACE_OUTER_BOUND ( 'NONE', #30868, .T. ) ;
#13585 = CARTESIAN_POINT ( 'NONE',  ( -87.52215345038483463, -23.48786465467240703, 11.44779295918254647 ) ) ;
#13586 = DIRECTION ( 'NONE',  ( -3.773278334444167608E-23, 1.000000000000000000, 0.000000000000000000 ) ) ;
#13587 = EDGE_CURVE ( 'NONE', #75398, #18738, #29908, .T. ) ;
#13588 = CARTESIAN_POINT ( 'NONE',  ( -28.62287095715004881, -29.50250243563660391, 8.947779535157950548 ) ) ;
#13589 = CARTESIAN_POINT ( 'NONE',  ( -5.366453405989236813, 2.363568322354391830E-15, -19.30000000000000071 ) ) ;
#13590 = CARTESIAN_POINT ( 'NONE',  ( -61.59189125704997281, -25.08279362854488781, 7.371166896404004909 ) ) ;
#13591 = EDGE_LOOP ( 'NONE', ( #22412, #14413, #99665, #47668 ) ) ;
#13592 = CARTESIAN_POINT ( 'NONE',  ( 19.37909195245082472, -6.530858791768283211, -1.500000000000002220 ) ) ;
#13593 = ORIENTED_EDGE ( 'NONE', *, *, #83463, .F. ) ;
#13594 = VERTEX_POINT ( 'NONE', #9332 ) ;
#13595 = ORIENTED_EDGE ( 'NONE', *, *, #40219, .F. ) ;
#13596 = ORIENTED_EDGE ( 'NONE', *, *, #47865, .F. ) ;
#13597 = CARTESIAN_POINT ( 'NONE',  ( 19.24196208499951055, 12.69117723712289703, 11.49999999999998934 ) ) ;
#13599 = EDGE_CURVE ( 'NONE', #91718, #95103, #93561, .T. ) ;
#13598 = CARTESIAN_POINT ( 'NONE',  ( -61.58760687538916301, -24.34968618360933945, 0.1864209137778810865 ) ) ;
#13600 = CARTESIAN_POINT ( 'NONE',  ( 13.55758662847591900, -15.04642845256218031, -1.500000000000002220 ) ) ;
#13601 = ORIENTED_EDGE ( 'NONE', *, *, #5110, .F. ) ;
#13602 = CARTESIAN_POINT ( 'NONE',  ( -29.96442039715612893, -23.42320092137126153, 11.44779298504228038 ) ) ;
#13603 = DIRECTION ( 'NONE',  ( 1.000000000000000000, 0.000000000000000000, 0.000000000000000000 ) ) ;
#13604 = EDGE_CURVE ( 'NONE', #63916, #79629, #56535, .T. ) ;
#13605 = CARTESIAN_POINT ( 'NONE',  ( -95.54583345656816107, -24.73486907724918282, 1.287355809206966128 ) ) ;
#13606 = CARTESIAN_POINT ( 'NONE',  ( -70.57979237444475018, -24.92564183028979130, 1.928384488918253536 ) ) ;
#13608 = ORIENTED_EDGE ( 'NONE', *, *, #728, .T. ) ;
#13607 = CARTESIAN_POINT ( 'NONE',  ( -12.70309173801008562, -17.24390854791867511, 11.49999999999999645 ) ) ;
#13609 = DIRECTION ( 'NONE',  ( 1.000000000000000000, 3.773278334444166432E-23, 8.201307841325785021E-29 ) ) ;
#13610 = CARTESIAN_POINT ( 'NONE',  ( -41.48648435019234881, -24.51314013834315375, 0.6176544820404115121 ) ) ;
#13611 = ORIENTED_EDGE ( 'NONE', *, *, #12321, .T. ) ;
#13612 = CARTESIAN_POINT ( 'NONE',  ( 18.79598114143782084, -8.675585332008726169, 11.49999999999998934 ) ) ;
#13613 = ORIENTED_EDGE ( 'NONE', *, *, #40388, .F. ) ;
#13614 = LINE ( 'NONE', #53707, #16158 ) ;
#13615 = VERTEX_POINT ( 'NONE', #227 ) ;
#13616 = CARTESIAN_POINT ( 'NONE',  ( 3.879812756903532556, -5.876774720514399419, 18.16163344421570969 ) ) ;
#13617 = ORIENTED_EDGE ( 'NONE', *, *, #23902, .T. ) ;
#13618 = CARTESIAN_POINT ( 'NONE',  ( -18.73635099073748833, 9.434554061794083069, -1.500000000000002220 ) ) ;
#13619 = CARTESIAN_POINT ( 'NONE',  ( 3.689792033372774060, 21.67897595795444587, 11.49999999999999645 ) ) ;
#13620 = CARTESIAN_POINT ( 'NONE',  ( -89.54348241549793386, -24.66019654487199730, 8.947790411086115725 ) ) ;
#13621 = CARTESIAN_POINT ( 'NONE',  ( -22.39070119279581306, -2.479732019442284496, -1.500000000000002220 ) ) ;
#13622 = CARTESIAN_POINT ( 'NONE',  ( 12.86141378215833342, 16.59024694808438127, -1.500000000000002220 ) ) ;
#13623 = CARTESIAN_POINT ( 'NONE',  ( 6.273728352332436309, -6.376774720514415407, 20.10092598260902008 ) ) ;
#13624 = CARTESIAN_POINT ( 'NONE',  ( -72.62287095715005592, -23.72747288104442021, -1.053458166803662888 ) ) ;
#13626 = EDGE_CURVE ( 'NONE', #12687, #5012, #71002, .T. ) ;
#13625 = CARTESIAN_POINT ( 'NONE',  ( -89.52287095715006160, -24.64898659630528854, 1.056161002820827921 ) ) ;
#13627 = EDGE_LOOP ( 'NONE', ( #3487, #42696, #1859, #44218 ) ) ;
#13628 = ORIENTED_EDGE ( 'NONE', *, *, #37915, .T. ) ;
#13629 = EDGE_LOOP ( 'NONE', ( #11765, #2061 ) ) ;
#13630 = CARTESIAN_POINT ( 'NONE',  ( -66.51029118470560775, -23.96119346886880308, -0.6495511937832151306 ) ) ;
#13631 = AXIS2_PLACEMENT_3D ( 'NONE', #83316, #97550, #75698 ) ;
#13632 = B_SPLINE_CURVE_WITH_KNOTS ( 'NONE', 3,
 ( #58207, #81037, #26250, #34862 ),
 .UNSPECIFIED., .F., .F.,
 ( 4, 4 ),
 ( 0.000000000000000000, 9.999999999998897304E-05 ),
 .UNSPECIFIED. ) ;
#13633 = CARTESIAN_POINT ( 'NONE',  ( -0.9917595143200197416, 21.46465604038169772, -1.500000000000002220 ) ) ;
#13634 = EDGE_CURVE ( 'NONE', #40608, #89889, #52841, .T. ) ;
#13635 = CARTESIAN_POINT ( 'NONE',  ( 5.399550031316281640, 0.3587747205144061202, -28.54570968857217395 ) ) ;
#13636 = ORIENTED_EDGE ( 'NONE', *, *, #14840, .T. ) ;
#13637 = CARTESIAN_POINT ( 'NONE',  ( -19.39432879369159224, 8.380699159679657839, 11.49999999999998934 ) ) ;
#13638 = LINE ( 'NONE', #96895, #75700 ) ;
#13639 = CARTESIAN_POINT ( 'NONE',  ( -81.75072539166535535, -25.24685308744632195, 6.293942982122118224 ) ) ;
#13640 = CARTESIAN_POINT ( 'NONE',  ( -83.63635015897777691, -23.96169478059713143, 10.65365249895718058 ) ) ;
#13641 = CARTESIAN_POINT ( 'NONE',  ( 14.61581676225068449, 3.316774720514424679, -27.35847991880143226 ) ) ;
#13642 = CARTESIAN_POINT ( 'NONE',  ( 6.026614999332422182E-17, -23.47596703998571499, 11.44779284984881684 ) ) ;
#13643 = CARTESIAN_POINT ( 'NONE',  ( -13.50798789833325664, 17.53495777034937220, -1.500000000000002220 ) ) ;
#13644 = PLANE ( 'NONE',  #63031 ) ;
#13645 = VECTOR ( 'NONE', #69401, 1000.000000000000000 ) ;
#13646 = CARTESIAN_POINT ( 'NONE',  ( -29.49875734969025842, -5.965225279485572685, 25.61802280011862720 ) ) ;
#13647 = CARTESIAN_POINT ( 'NONE',  ( -64.58953762381672448, -23.47593901973091235, -1.443836447539007972 ) ) ;
#13648 = CARTESIAN_POINT ( 'NONE',  ( -99.52287095715009002, -23.72773821059536914, 11.05748984161097503 ) ) ;
#13649 = CARTESIAN_POINT ( 'NONE',  ( -100.5894454694905562, -24.52300882791526959, 0.6510814631126226049 ) ) ;
#13650 = CARTESIAN_POINT ( 'NONE',  ( 11.34002819025610087, 15.78594478779102950, -1.500000000000002220 ) ) ;
#13651 = CARTESIAN_POINT ( 'NONE',  ( -21.27170209485220198, -2.091907790468015005, -1.500000000000002220 ) ) ;
#13652 = CARTESIAN_POINT ( 'NONE',  ( 14.82775695341588573, -5.152774720514427642, -26.90408793620859385 ) ) ;
#13653 = DIRECTION ( 'NONE',  ( -3.773278334444166432E-23, 1.000000000000000000, 0.000000000000000000 ) ) ;
#13654 = CARTESIAN_POINT ( 'NONE',  ( -40.62287095715004170, -25.00158670708908204, 2.256160236439166411 ) ) ;
#13655 = DIRECTION ( 'NONE',  ( -3.773278334453079030E-23, 0.9999999999976377785, 2.173523156925979128E-06 ) ) ;
#13656 = CARTESIAN_POINT ( 'NONE',  ( -21.41681981171885951, -7.298096547245328303, -1.500000000000002220 ) ) ;
#13657 = EDGE_CURVE ( 'NONE', #27531, #73030, #25565, .T. ) ;
#13658 = ORIENTED_EDGE ( 'NONE', *, *, #18155, .T. ) ;
#13659 = CARTESIAN_POINT ( 'NONE',  ( -108.6228709571500559, -29.50250243563736774, 8.947779886222136270 ) ) ;
#13660 = CARTESIAN_POINT ( 'NONE',  ( 8.978253834636468866, -6.376774720514426953, 0.000000000000000000 ) ) ;
#13661 = CARTESIAN_POINT ( 'NONE',  ( -15.09475962229707591, 12.77647934908296712, 11.49999999999999645 ) ) ;
#13662 = CARTESIAN_POINT ( 'NONE',  ( -59.62287095715005592, -23.73907113216990439, -1.053371485793229256 ) ) ;
#13663 = CARTESIAN_POINT ( 'NONE',  ( -76.55620429048342146, -23.48783264082478084, -1.443836473390065933 ) ) ;
#13664 = ORIENTED_EDGE ( 'NONE', *, *, #42415, .T. ) ;
#13665 = CARTESIAN_POINT ( 'NONE',  ( -53.62287095715005592, -24.64965695001467694, 8.947790433994185832 ) ) ;
#13667 = ADVANCED_FACE ( 'NONE', ( #46906 ), #63145, .F. ) ;
#13666 = CARTESIAN_POINT ( 'NONE',  ( -68.52287095715003318, -23.96127896941631619, -0.6493128931038056884 ) ) ;
#13668 = CARTESIAN_POINT ( 'NONE',  ( -0.6006773669993965559, 21.62980403441659760, -1.500000000000002220 ) ) ;
#13669 = ADVANCED_FACE ( 'NONE', ( #32171 ), #79845, .T. ) ;
#13670 = CARTESIAN_POINT ( 'NONE',  ( -26.49193215146072689, -24.84431178523845674, 6.877568485563839040 ) ) ;
#13671 = CARTESIAN_POINT ( 'NONE',  ( 6.036767712469883307, 18.47306877840545170, -1.500000000000002220 ) ) ;
#13672 = B_SPLINE_CURVE_WITH_KNOTS ( 'NONE', 3,
 ( #70145, #30581, #84365, #21951, #8250, #46819, #52936, #15347, #31579, #631, #77735, #46310 ),
 .UNSPECIFIED., .F., .F.,
 ( 4, 2, 2, 2, 2, 4 ),
 ( 0.000000000000000000, 0.0001663275863830617580, 0.0003326551727661235160, 0.0006653103455322287091, 0.0009979655182983339021, 0.001330620691064439204 ),
 .UNSPECIFIED. ) ;
#13673 = EDGE_CURVE ( 'NONE', #77609, #54376, #10847, .T. ) ;
#13674 = CARTESIAN_POINT ( 'NONE',  ( -82.52287095715003318, -23.73934037231756022, 11.05740245334328620 ) ) ;
#13675 = CARTESIAN_POINT ( 'NONE',  ( -93.52287095715006160, -23.48786465467241769, 11.44779295918254292 ) ) ;
#13676 = CARTESIAN_POINT ( 'NONE',  ( 19.71268880909926580, -1.816447362451163450, -1.500000000000002220 ) ) ;
#13677 = ORIENTED_EDGE ( 'NONE', *, *, #22221, .F. ) ;
#13678 = EDGE_CURVE ( 'NONE', #94726, #100015, #39544, .T. ) ;
#13679 = B_SPLINE_CURVE_WITH_KNOTS ( 'NONE', 3,
 ( #1692, #63604, #78786, #32627 ),
 .UNSPECIFIED., .F., .F.,
 ( 4, 4 ),
 ( 0.000000000000000000, 9.999999999998897304E-05 ),
 .UNSPECIFIED. ) ;
#13680 = VECTOR ( 'NONE', #57759, 1000.000000000000000 ) ;
#13681 = CARTESIAN_POINT ( 'NONE',  ( 17.44645523915803764, -10.38078700900905993, 11.49999999999999645 ) ) ;
#13682 = DIRECTION ( 'NONE',  ( -0.000000000000000000, 2.173523156925979552E-06, -0.9999999999976378895 ) ) ;
#13683 = CARTESIAN_POINT ( 'NONE',  ( -105.6228709571500417, -24.99132157543166954, 2.256160258750667502 ) ) ;
#13684 = EDGE_LOOP ( 'NONE', ( #70318, #99707, #23860, #75491 ) ) ;
#13685 = B_SPLINE_SURFACE_WITH_KNOTS ( 'NONE', 3, 3, ( 
 ( #13096, #74996, #22699, #5995 ),
 ( #29332, #99335, #14601, #53686 ),
 ( #52177, #12608, #44566, #5497 ),
 ( #22202, #20711, #6502, #6997 ),
 ( #37452, #13598, #37944, #5001 ),
 ( #28839, #97839, #90738, #36446 ),
 ( #30326, #68403, #66919, #28333 ) ),
 .UNSPECIFIED., .F., .F., .F.,
 ( 4, 3, 4 ),
 ( 4, 4 ),
 ( 0.0004766839783815518170, 0.1029713700210893451, 0.2054660560637971423 ),
 ( 0.6896694373704013170, 0.6910003741376167241 ),
 .UNSPECIFIED. ) ;
#13686 = CARTESIAN_POINT ( 'NONE',  ( -102.6362921444641501, -23.48786465467241058, 11.44779295918254292 ) ) ;
#13687 = CARTESIAN_POINT ( 'NONE',  ( 14.10331789288738236, -5.152774720514426754, -26.41276880515819769 ) ) ;
#13688 = DIRECTION ( 'NONE',  ( 0.000000000000000000, 0.000000000000000000, 1.000000000000000000 ) ) ;
#13689 = CARTESIAN_POINT ( 'NONE',  ( -41.32836283488544638, -4.132774720514426292, 39.26872235229541985 ) ) ;
#13690 = CARTESIAN_POINT ( 'NONE',  ( -123.6228709571500559, -29.50247984919015209, -1.443849546365046699 ) ) ;
#13691 = CARTESIAN_POINT ( 'NONE',  ( 1.781536345648733199, 20.00535218256611358, 11.49999999999998934 ) ) ;
#13692 = EDGE_CURVE ( 'NONE', #13741, #43203, #72254, .T. ) ;
#13693 = EDGE_CURVE ( 'NONE', #64178, #75014, #58965, .T. ) ;
#13694 = CARTESIAN_POINT ( 'NONE',  ( -28.52287095715007226, -23.32374950011072912, -1.443835813551990643 ) ) ;
#13695 = ORIENTED_EDGE ( 'NONE', *, *, #460, .T. ) ;
#13696 = CARTESIAN_POINT ( 'NONE',  ( -117.6228709571500133, -23.95044443724991368, 10.65354141964649592 ) ) ;
#13697 = CARTESIAN_POINT ( 'NONE',  ( 17.53461989915211916, -14.66684187699354425, 11.49999999999999645 ) ) ;
#13698 = CARTESIAN_POINT ( 'NONE',  ( -49.50841769935764347, -25.31297054157952431, 3.984447646101154650 ) ) ;
#13699 = CARTESIAN_POINT ( 'NONE',  ( -82.58953762381671027, -24.65952944569304606, 1.056160979905701902 ) ) ;
#13700 = CARTESIAN_POINT ( 'NONE',  ( -53.52287095715008292, -23.47593901973090169, -1.443836447538997092 ) ) ;
#13701 = CARTESIAN_POINT ( 'NONE',  ( 0.000000000000000000, -1.473225279485573802, 4.300000000000000711 ) ) ;
#13702 = AXIS2_PLACEMENT_3D ( 'NONE', #26453, #48289, #2619 ) ;
#13703 = ADVANCED_FACE ( 'NONE', ( #18453 ), #34685, .T. ) ;
#13704 = CARTESIAN_POINT ( 'NONE',  ( -32.52287095715004739, -23.47593901973090169, -1.443836447538997092 ) ) ;
#13705 = B_SPLINE_CURVE_WITH_KNOTS ( 'NONE', 3,
 ( #4651, #89381, #19852, #50828, #43220, #66576 ),
 .UNSPECIFIED., .F., .F.,
 ( 4, 2, 4 ),
 ( 1.570887131794952276E-05, 0.001396322306279764325, 0.002776935741241578874 ),
 .UNSPECIFIED. ) ;
#13706 = CARTESIAN_POINT ( 'NONE',  ( -99.62287095715005592, -29.50247984919015209, -1.443849546365050029 ) ) ;
#13707 = ORIENTED_EDGE ( 'NONE', *, *, #49923, .F. ) ;
#13708 = CARTESIAN_POINT ( 'NONE',  ( -14.79517943714664518, -13.99575967537150412, 11.49999999999998934 ) ) ;
#13709 = EDGE_LOOP ( 'NONE', ( #8658, #43954, #7528, #95977 ) ) ;
#13710 = CARTESIAN_POINT ( 'NONE',  ( -6.529369910325518944, -22.02198592821369516, -1.500000000000002220 ) ) ;
#13711 = EDGE_CURVE ( 'NONE', #15369, #3440, #29828, .T. ) ;
#13712 = CARTESIAN_POINT ( 'NONE',  ( -115.5895376238167245, -23.48786465467242479, 11.44779295918253759 ) ) ;
#13713 = AXIS2_PLACEMENT_3D ( 'NONE', #73049, #65452, #36464 ) ;
#13714 = ORIENTED_EDGE ( 'NONE', *, *, #41768, .F. ) ;
#13715 = CARTESIAN_POINT ( 'NONE',  ( -108.6247740409122571, -24.51419770103158768, 9.386484678747162747 ) ) ;
#13716 = EDGE_CURVE ( 'NONE', #71522, #8729, #88975, .T. ) ;
#13717 = CARTESIAN_POINT ( 'NONE',  ( -67.52287095715001897, -23.95044443724991723, 10.65354141964649415 ) ) ;
#13718 = EDGE_CURVE ( 'NONE', #67104, #57214, #41294, .T. ) ;
#13719 = LINE ( 'NONE', #73146, #85266 ) ;
#13721 = EDGE_LOOP ( 'NONE', ( #92403, #5993, #25233, #30946 ) ) ;
#13720 = CARTESIAN_POINT ( 'NONE',  ( -12.29646723538143505, -17.35194501319736560, 11.49999999999999645 ) ) ;
#13722 = VERTEX_POINT ( 'NONE', #73737 ) ;
#13723 = CARTESIAN_POINT ( 'NONE',  ( 12.08182546098005972, -18.57710416600862402, -1.500000000000002220 ) ) ;
#13724 = CARTESIAN_POINT ( 'NONE',  ( 1.647368763193059582, 20.57021071130147405, -1.500000000000002220 ) ) ;
#13725 = VERTEX_POINT ( 'NONE', #42319 ) ;
#13726 = ORIENTED_EDGE ( 'NONE', *, *, #19667, .T. ) ;
#13727 = CARTESIAN_POINT ( 'NONE',  ( 7.462166178408539352, 5.965225279485572685, -27.67315496249664974 ) ) ;
#13728 = CARTESIAN_POINT ( 'NONE',  ( -39.04303308397305727, -25.29008967749855685, 4.215216926603018166 ) ) ;
#13729 = ORIENTED_EDGE ( 'NONE', *, *, #95259, .T. ) ;
#13730 = VERTEX_POINT ( 'NONE', #4233 ) ;
#13731 = LINE ( 'NONE', #7635, #6522 ) ;
#13732 = CARTESIAN_POINT ( 'NONE',  ( -41.49885461251451346, -24.15620529776627734, 10.23563542870660825 ) ) ;
#13733 = DIRECTION ( 'NONE',  ( 0.000000000000000000, -0.9999999999976377785, -2.173523156925979128E-06 ) ) ;
#13734 = CARTESIAN_POINT ( 'NONE',  ( -8.730572200882948053, 18.91488879456464289, -1.500000000000002220 ) ) ;
#13735 = CARTESIAN_POINT ( 'NONE',  ( -19.76859095128058996, -9.124614402804876789, 11.49999999999999645 ) ) ;
#13736 = CARTESIAN_POINT ( 'NONE',  ( -50.88733314876014902, -25.04353333182355357, 7.513223449029553080 ) ) ;
#13737 = CARTESIAN_POINT ( 'NONE',  ( -77.52287095715006160, -23.48786465467241058, 11.44779295918254469 ) ) ;
#13738 = CARTESIAN_POINT ( 'NONE',  ( -115.5149161931255719, -24.73486907724918282, 1.287355809206964352 ) ) ;
#13739 = CARTESIAN_POINT ( 'NONE',  ( -16.84940295534276800, 14.81145437567392698, 11.49999999999998934 ) ) ;
#13740 = CARTESIAN_POINT ( 'NONE',  ( -51.22891850606554698, -25.31296662437967626, 4.264007001526691987 ) ) ;
#13741 = VERTEX_POINT ( 'NONE', #26576 ) ;
#13742 = CARTESIAN_POINT ( 'NONE',  ( -4.568292318365942073, 5.965225279485572685, 30.06720597538392425 ) ) ;
#13743 = CARTESIAN_POINT ( 'NONE',  ( -8.349999999999971223, 27.69999999999999574, 0.000000000000000000 ) ) ;
#13744 = AXIS2_PLACEMENT_3D ( 'NONE', #6821, #45898, #52013 ) ;
#13745 = VERTEX_POINT ( 'NONE', #88473 ) ;
#13746 = B_SPLINE_CURVE_WITH_KNOTS ( 'NONE', 3,
 ( #64316, #64822, #95735, #26224, #88131, #18599, #97727, #19598, #42960, #44450, #91109, #20100, #28722, #29216 ),
 .UNSPECIFIED., .F., .F.,
 ( 4, 2, 2, 2, 2, 2, 4 ),
 ( 2.809234570782672869E-17, 0.0001998554611590488311, 0.0003997109223180695813, 0.0007994218446360915661, 0.001199132766954113605, 0.001398988228113124625, 0.001598843689272135644 ),
 .UNSPECIFIED. ) ;
#13747 = ORIENTED_EDGE ( 'NONE', *, *, #61912, .T. ) ;
#13748 = DIRECTION ( 'NONE',  ( -3.773278334444166432E-23, 1.000000000000000000, 0.000000000000000000 ) ) ;
#13749 = ORIENTED_EDGE ( 'NONE', *, *, #50593, .T. ) ;
#13750 = CARTESIAN_POINT ( 'NONE',  ( -21.26230640008892792, -0.7210608269398429693, -1.500000000000002220 ) ) ;
#13751 = VERTEX_POINT ( 'NONE', #11344 ) ;
#13752 = CARTESIAN_POINT ( 'NONE',  ( -5.366453405989236813, 2.681976490132703452E-15, -21.89999999999999858 ) ) ;
#13753 = CARTESIAN_POINT ( 'NONE',  ( 7.388015978253313243, 19.69965359013245632, -1.500000000000002220 ) ) ;
#13754 = CARTESIAN_POINT ( 'NONE',  ( -35.52287095715006870, -25.00158670708909270, 2.256160236439166411 ) ) ;
#13755 = CARTESIAN_POINT ( 'NONE',  ( -110.8642813400260678, -25.21264688230269968, 3.422668213661852032 ) ) ;
#13756 = CARTESIAN_POINT ( 'NONE',  ( 7.526024287269984292, 1.477225279485574028, 9.032262774691707463 ) ) ;
#13757 = CARTESIAN_POINT ( 'NONE',  ( -21.49438740719132923, 4.340694165963498996, -1.500000000000002220 ) ) ;
#13758 = DIRECTION ( 'NONE',  ( -0.5630016722799275897, 4.164321980682959710E-15, 0.8264557562326038109 ) ) ;
#13759 = ORIENTED_EDGE ( 'NONE', *, *, #17258, .F. ) ;
#13760 = CARTESIAN_POINT ( 'NONE',  ( 29.64418490232317893, -5.621712738193696879, 28.18100406333994457 ) ) ;
#13762 = B_SPLINE_CURVE_WITH_KNOTS ( 'NONE', 3,
 ( #82408, #5287, #36248, #68192 ),
 .UNSPECIFIED., .F., .F.,
 ( 4, 4 ),
 ( 1.387778780781445676E-17, 0.0001000000000000028508 ),
 .UNSPECIFIED. ) ;
#13761 = CARTESIAN_POINT ( 'NONE',  ( -84.58277711012007671, -24.66019654487200441, 8.947790411086119278 ) ) ;
#13763 = LINE ( 'NONE', #61468, #95971 ) ;
#13764 = DIRECTION ( 'NONE',  ( 0.000000000000000000, -0.9999999999976377785, -2.173523156925979975E-06 ) ) ;
#13765 = CARTESIAN_POINT ( 'NONE',  ( 21.14028111218437900, -2.610574537768086234, 11.49999999999998934 ) ) ;
#13766 = DIRECTION ( 'NONE',  ( -0.000000000000000000, -0.000000000000000000, -1.000000000000000000 ) ) ;
#13767 = CARTESIAN_POINT ( 'NONE',  ( -107.5907561945975459, -24.15620529776628800, 10.23563542870659759 ) ) ;
#13768 = AXIS2_PLACEMENT_3D ( 'NONE', #16089, #86106, #47560 ) ;
#13769 = CARTESIAN_POINT ( 'NONE',  ( -29.52287095715006160, -23.38909342368989641, 11.44779306042727285 ) ) ;
#13770 = CARTESIAN_POINT ( 'NONE',  ( -33.65849158002127695, -23.73766607897670866, -1.055555164236444909 ) ) ;
#13771 = CARTESIAN_POINT ( 'NONE',  ( -19.72384299526936857, -10.77339039931002773, -1.500000000000002220 ) ) ;
#13772 = CARTESIAN_POINT ( 'NONE',  ( -110.3139465455115129, -29.50248914370730091, 2.832395270851967073 ) ) ;
#13773 = ORIENTED_EDGE ( 'NONE', *, *, #23318, .F. ) ;
#13774 = ADVANCED_FACE ( 'NONE', ( #97571 ), #81852, .F. ) ;
#13775 = CARTESIAN_POINT ( 'NONE',  ( -98.89303308397306580, -25.26498937201382233, 6.110950154240443410 ) ) ;
#13776 = CARTESIAN_POINT ( 'NONE',  ( -2.340448316220725467, 19.49152957720520618, 11.49999999999999645 ) ) ;
#13777 = LINE ( 'NONE', #82799, #29265 ) ;
#13778 = ADVANCED_FACE ( 'NONE', ( #19942 ), #3252, .F. ) ;
#13779 = DIRECTION ( 'NONE',  ( -0.6599726524652352877, 0.000000000000000000, 0.7512896232465892110 ) ) ;
#13780 = ORIENTED_EDGE ( 'NONE', *, *, #51042, .F. ) ;
#13781 = VECTOR ( 'NONE', #86515, 1000.000000000000000 ) ;
#13782 = ADVANCED_FACE ( 'NONE', ( #57036 ), #73250, .F. ) ;
#13783 = CARTESIAN_POINT ( 'NONE',  ( -69.60169030842801874, -25.30567014228302725, 5.021178964433338443 ) ) ;
#13784 = CARTESIAN_POINT ( 'NONE',  ( -99.33274021282838362, -25.31439685940647877, 5.901068652850602447 ) ) ;
#13785 = EDGE_CURVE ( 'NONE', #32994, #83380, #79423, .T. ) ;
#13786 = AXIS2_PLACEMENT_3D ( 'NONE', #4388, #18103, #34335 ) ;
#13787 = CARTESIAN_POINT ( 'NONE',  ( -122.5228709571500758, -23.47593901973090524, -1.443836447538996204 ) ) ;
#13788 = EDGE_CURVE ( 'NONE', #26222, #19840, #12932, .T. ) ;
#13789 = CARTESIAN_POINT ( 'NONE',  ( -2.117704968268854682, 19.61795684621070990, 11.49999999999998934 ) ) ;
#13790 = ORIENTED_EDGE ( 'NONE', *, *, #41900, .T. ) ;
#13791 = CARTESIAN_POINT ( 'NONE',  ( 5.471383689419965890, 0.3587747205144057872, -29.02273493113404612 ) ) ;
#13792 = CARTESIAN_POINT ( 'NONE',  ( -70.62287095715004170, -23.48783264082478084, -1.443836473390067265 ) ) ;
#13793 = ADVANCED_BREP_SHAPE_REPRESENTATION ( '', ( #75728, #37391 ), #35871 ) ;
#13794 = CALENDAR_DATE ( 2026, 9, 10 ) ;
#13795 = ORIENTED_EDGE ( 'NONE', *, *, #98031, .F. ) ;
#13796 = CARTESIAN_POINT ( 'NONE',  ( -124.5228709571500616, -24.64965694238575722, 8.947790433994191162 ) ) ;
#13797 = CARTESIAN_POINT ( 'NONE',  ( -1.363607173041644582, -6.376774720514420736, 20.50445910983877340 ) ) ;
#13798 = CARTESIAN_POINT ( 'NONE',  ( -55.49176352103356180, -24.52300882791530157, 0.6510814631126364826 ) ) ;
#13799 = CARTESIAN_POINT ( 'NONE',  ( -118.5566399227117245, -23.73766607897671221, -1.055555164236448462 ) ) ;
#13800 = CARTESIAN_POINT ( 'NONE',  ( -7.304748120944324796, -6.376774720514417183, 19.95463486386180563 ) ) ;
#13801 = CARTESIAN_POINT ( 'NONE',  ( -99.62287095715016960, -24.35013146730204170, 9.818937971375104823 ) ) ;
#13802 = FACE_OUTER_BOUND ( 'NONE', #85470, .T. ) ;
#13803 = CARTESIAN_POINT ( 'NONE',  ( 18.25133680241413359, 8.160682379734268466, -1.500000000000002220 ) ) ;
#13804 = EDGE_CURVE ( 'NONE', #36030, #83300, #29550, .T. ) ;
#13805 = DIRECTION ( 'NONE',  ( -3.773278334453080206E-23, 0.9999999999976377785, 2.173523156925979552E-06 ) ) ;
#13806 = CARTESIAN_POINT ( 'NONE',  ( -45.47735399304787052, -24.83644354573577928, 8.397322867130094792 ) ) ;
#13807 = ORIENTED_EDGE ( 'NONE', *, *, #45836, .T. ) ;
#13808 = CARTESIAN_POINT ( 'NONE',  ( -74.58953762381673869, -24.64898659630367561, 1.056161002820383388 ) ) ;
#13809 = CARTESIAN_POINT ( 'NONE',  ( -1.164890887384984586, 4.028272616778474813, -2.677392948487098267E-15 ) ) ;
#13810 = EDGE_CURVE ( 'NONE', #34688, #26860, #60028, .T. ) ;
#13811 = CARTESIAN_POINT ( 'NONE',  ( -119.5202043240208383, -23.96119346886881019, -0.6495511937832018079 ) ) ;
#13812 = AXIS2_PLACEMENT_3D ( 'NONE', #41048, #12948, #33423 ) ;
#13813 = DIRECTION ( 'NONE',  ( -0.4009304992412300317, 6.845827386180410961E-16, -0.9161084732596779245 ) ) ;
#13814 = CARTESIAN_POINT ( 'NONE',  ( -126.8947205558307303, -25.24722654741731276, 6.200372419592135920 ) ) ;
#13815 = CARTESIAN_POINT ( 'NONE',  ( -81.59989050339841299, -23.73766607897671221, -1.055555164236432919 ) ) ;
#13816 = LINE ( 'NONE', #90953, #72397 ) ;
#13817 = CARTESIAN_POINT ( 'NONE',  ( -51.69567503897438598, -25.26279930336529489, 4.127965216627219824 ) ) ;
#13818 = B_SPLINE_CURVE_WITH_KNOTS ( 'NONE', 3,
 ( #37867, #31244, #68817, #23116 ),
 .UNSPECIFIED., .F., .F.,
 ( 4, 4 ),
 ( 0.1706218368772978167, 0.1796282681494135169 ),
 .UNSPECIFIED. ) ;
#13819 = B_SPLINE_CURVE_WITH_KNOTS ( 'NONE', 3,
 ( #17240, #63954, #25855, #40086 ),
 .UNSPECIFIED., .F., .F.,
 ( 4, 4 ),
 ( 2.775557561562891351E-17, 9.999999999996123101E-05 ),
 .UNSPECIFIED. ) ;
#13820 = CARTESIAN_POINT ( 'NONE',  ( -87.62287095715004170, -24.65952944569304606, 1.056160979905700348 ) ) ;
#13821 = CARTESIAN_POINT ( 'NONE',  ( -127.5898613667035875, -24.15543982623907837, -0.2315651400026538520 ) ) ;
#13822 = ORIENTED_EDGE ( 'NONE', *, *, #46423, .T. ) ;
#13823 = CARTESIAN_POINT ( 'NONE',  ( -12.33117494125061242, 16.09929768045241261, -1.500000000000002220 ) ) ;
#13824 = B_SPLINE_CURVE_WITH_KNOTS ( 'NONE', 3,
 ( #92998, #99111, #22973, #99602, #38718, #54454 ),
 .UNSPECIFIED., .F., .F.,
 ( 4, 2, 4 ),
 ( 0.000000000000000000, 0.001380764517854760629, 0.002761529035709521258 ),
 .UNSPECIFIED. ) ;
#13825 = CARTESIAN_POINT ( 'NONE',  ( -122.6250502620820981, -24.15543982623907482, -0.2315651400026565443 ) ) ;
#13826 = CARTESIAN_POINT ( 'NONE',  ( -116.6228709571500559, -29.50247984919015209, -1.443849546365046699 ) ) ;
#13827 = CARTESIAN_POINT ( 'NONE',  ( -34.52287095715006160, -23.47596703998600631, 11.44779298504229459 ) ) ;
#13829 = EDGE_LOOP ( 'NONE', ( #37355, #27458, #22741, #77854 ) ) ;
#13828 = EDGE_CURVE ( 'NONE', #40606, #66289, #8091, .T. ) ;
#13830 = LINE ( 'NONE', #31053, #19329 ) ;
#13831 = PLANE ( 'NONE',  #77775 ) ;
#13832 = CARTESIAN_POINT ( 'NONE',  ( -18.22032804147677254, 8.545885342870345625, -1.500000000000002220 ) ) ;
#13833 = CARTESIAN_POINT ( 'NONE',  ( 12.48895993392301307, -16.95307763291877379, 11.49999999999999645 ) ) ;
#13834 = CARTESIAN_POINT ( 'NONE',  ( 30.54125281784916268, -0.6647747205144264315, 23.11160796525322070 ) ) ;
#13835 = CARTESIAN_POINT ( 'NONE',  ( -70.53621709966942888, -24.83644354573578283, 8.397322867130098345 ) ) ;
#13836 = CARTESIAN_POINT ( 'NONE',  ( -13.14421341422731260, -17.72855101262432242, 11.49999999999998934 ) ) ;
#13837 = EDGE_CURVE ( 'NONE', #16488, #84333, #3256, .T. ) ;
#13838 = VECTOR ( 'NONE', #50509, 1000.000000000000114 ) ;
#13839 = CARTESIAN_POINT ( 'NONE',  ( 2.947869850540926429, 20.32360706268488215, -1.500000000000002220 ) ) ;
#13840 = CARTESIAN_POINT ( 'NONE',  ( -66.52287095715003318, -24.66019654487199375, 8.947790411086119278 ) ) ;
#13841 = VECTOR ( 'NONE', #67163, 1000.000000000000000 ) ;
#13842 = CARTESIAN_POINT ( 'NONE',  ( -59.58953762381671737, -24.64898659630367916, 1.056161002820383166 ) ) ;
#13843 = ORIENTED_EDGE ( 'NONE', *, *, #10142, .F. ) ;
#13844 = CARTESIAN_POINT ( 'NONE',  ( 33.00535138976610483, 5.965225279485572685, -12.97242311383961422 ) ) ;
#13845 = ORIENTED_EDGE ( 'NONE', *, *, #49854, .F. ) ;
#13846 = DIRECTION ( 'NONE',  ( -3.773278334453079618E-23, 0.9999999999976377785, 2.173523156925979975E-06 ) ) ;
#13847 = CARTESIAN_POINT ( 'NONE',  ( -72.52287095715007581, -24.64965694238575011, 8.947790433994200043 ) ) ;
#13848 = VERTEX_POINT ( 'NONE', #51406 ) ;
#13849 = CIRCLE ( 'NONE', #26836, 1.649999999999998579 ) ;
#13850 = ORIENTED_EDGE ( 'NONE', *, *, #22985, .T. ) ;
#13851 = CARTESIAN_POINT ( 'NONE',  ( -4.568292318365942073, 5.965225279485572685, 30.06720597538392425 ) ) ;
#13852 = LINE ( 'NONE', #92470, #50273 ) ;
#13853 = CARTESIAN_POINT ( 'NONE',  ( -76.58157264639545758, -24.65952944569303895, 1.056160979905700792 ) ) ;
#13854 = CARTESIAN_POINT ( 'NONE',  ( 0.1292827521129817636, -20.55975067039486603, -1.500000000000002220 ) ) ;
#13855 = B_SPLINE_CURVE_WITH_KNOTS ( 'NONE', 3,
 ( #79749, #80257, #35089, #86857 ),
 .UNSPECIFIED., .F., .F.,
 ( 4, 4 ),
 ( 0.9311649220781571534, 0.9401713533502727982 ),
 .UNSPECIFIED. ) ;
#13856 = VECTOR ( 'NONE', #48242, 1000.000000000000000 ) ;
#13857 = CARTESIAN_POINT ( 'NONE',  ( -8.750087785235610482, 19.73178376063210138, 11.49999999999999645 ) ) ;
#13858 = ORIENTED_EDGE ( 'NONE', *, *, #99262, .T. ) ;
#13859 = DIRECTION ( 'NONE',  ( -1.000000000000000000, -3.773278334444167608E-23, -8.201307833595939069E-29 ) ) ;
#13860 = CARTESIAN_POINT ( 'NONE',  ( -35.55620429048339304, -23.48783264082477729, -1.443836473390072372 ) ) ;
#13861 = CARTESIAN_POINT ( 'NONE',  ( 18.00092565640838416, -13.26076702590692769, 11.49999999999998934 ) ) ;
#13862 = VECTOR ( 'NONE', #47810, 1000.000000000000114 ) ;
#13863 = CARTESIAN_POINT ( 'NONE',  ( -117.5228709571500332, -24.66019654487200441, 8.947790411086108620 ) ) ;
#13864 = CARTESIAN_POINT ( 'NONE',  ( -84.55446260568123762, -23.96119346886880663, -0.6495511937832096905 ) ) ;
#13865 = EDGE_LOOP ( 'NONE', ( #21488, #38228, #48342 ) ) ;
#13866 = DIRECTION ( 'NONE',  ( -0.000000000000000000, -1.000000000000000000, -0.000000000000000000 ) ) ;
#13867 = DIRECTION ( 'NONE',  ( -3.773278334453079030E-23, 0.9999999999976377785, 2.173523156925979128E-06 ) ) ;
#13868 = CARTESIAN_POINT ( 'NONE',  ( 20.83135763335140922, 1.668377004047274959, 11.49999999999998934 ) ) ;
#13869 = ORIENTED_EDGE ( 'NONE', *, *, #4139, .F. ) ;
#13871 = ORIENTED_EDGE ( 'NONE', *, *, #45884, .T. ) ;
#13870 = CARTESIAN_POINT ( 'NONE',  ( -67.49690699276101213, -24.51419770103159124, 9.386484678747168076 ) ) ;
#13872 = ORIENTED_EDGE ( 'NONE', *, *, #3410, .T. ) ;
#13873 = CARTESIAN_POINT ( 'NONE',  ( -100.6291315273262796, -24.52399227489127398, 9.353111116836521077 ) ) ;
#13874 = CARTESIAN_POINT ( 'NONE',  ( -19.39432879369159224, 8.380699159679657839, -1.500000000000002220 ) ) ;
#13875 = ORIENTED_EDGE ( 'NONE', *, *, #54270, .F. ) ;
#13876 = CARTESIAN_POINT ( 'NONE',  ( -117.6294079147639593, -23.48783264082477018, -1.443836473390081254 ) ) ;
#13877 = CARTESIAN_POINT ( 'NONE',  ( 30.64697572893791744, -5.232796261063619170, 0.6042509527384705148 ) ) ;
#13878 = CARTESIAN_POINT ( 'NONE',  ( -0.2038501785326352067, 21.78777694363981254, -1.500000000000002220 ) ) ;
#13879 = CARTESIAN_POINT ( 'NONE',  ( -76.51686106428668666, -23.73791477778911840, 11.05961554403170766 ) ) ;
#13880 = CARTESIAN_POINT ( 'NONE',  ( -28.47875734969025885, 6.475225279485573360, -0.08597719988137117464 ) ) ;
#13881 = CARTESIAN_POINT ( 'NONE',  ( 14.05712878599199200, -16.60762996970646199, -1.500000000000002220 ) ) ;
#13882 = CARTESIAN_POINT ( 'NONE',  ( -71.60837349177994327, -25.31639633020554925, 5.637668385895925560 ) ) ;
#13884 = ORIENTED_EDGE ( 'NONE', *, *, #82442, .F. ) ;
#13883 = CARTESIAN_POINT ( 'NONE',  ( -0.4079105510268487000, 22.33655531192813370, 11.49999999999999645 ) ) ;
#13885 = CARTESIAN_POINT ( 'NONE',  ( -31.24388727629348494, -29.50248678627064081, 1.747779886239157809 ) ) ;
#13886 = CARTESIAN_POINT ( 'NONE',  ( -123.5562042904833930, -24.65952944569304961, 1.056160979905707453 ) ) ;
#13887 = LINE ( 'NONE', #89036, #95864 ) ;
#13888 = ORIENTED_EDGE ( 'NONE', *, *, #58258, .T. ) ;
#13889 = ORIENTED_EDGE ( 'NONE', *, *, #52, .T. ) ;
#13890 = ORIENTED_EDGE ( 'NONE', *, *, #73487, .F. ) ;
#13891 = AXIS2_PLACEMENT_3D ( 'NONE', #20937, #22422, #84331 ) ;
#13892 = CARTESIAN_POINT ( 'NONE',  ( -20.47705334459678994, -22.77463087841388045, -1.497999999999533038 ) ) ;
#13893 = CARTESIAN_POINT ( 'NONE',  ( -34.62287095715005592, -23.48786465467240347, 11.44779295918255535 ) ) ;
#13894 = CARTESIAN_POINT ( 'NONE',  ( 30.59299694858157892, -5.371884064401012182, 26.41087035901067637 ) ) ;
#13895 = CARTESIAN_POINT ( 'NONE',  ( -75.62287095715004170, -24.99132157543084176, 2.256160258750667502 ) ) ;
#13896 = CARTESIAN_POINT ( 'NONE',  ( 33.41145047975764726, 4.538943570064879474, -12.61568413423376889 ) ) ;
#13897 = CARTESIAN_POINT ( 'NONE',  ( 2.021814659504407579E-13, -19.30000000000000426, -1.500000000000002220 ) ) ;
#13898 = ADVANCED_FACE ( 'NONE', ( #44794 ), #89961, .F. ) ;
#13899 = CARTESIAN_POINT ( 'NONE',  ( -36.58953762381673158, -24.66019654487199375, 8.947790411086137041 ) ) ;
#13900 = EDGE_LOOP ( 'NONE', ( #50358, #25369, #99565, #40477 ) ) ;
#13901 = EDGE_CURVE ( 'NONE', #83680, #38147, #21426, .T. ) ;
#13902 = CARTESIAN_POINT ( 'NONE',  ( 9.746180923669104601, -16.83516941858706417, 11.49999999999999645 ) ) ;
#13903 = CARTESIAN_POINT ( 'NONE',  ( -87.62287095715004170, -23.47596703998600631, 11.44779298504227860 ) ) ;
#13904 = VERTEX_POINT ( 'NONE', #45784 ) ;
#13905 = CARTESIAN_POINT ( 'NONE',  ( 3.362850247043494001, -6.376774720514404748, 18.65880685207958223 ) ) ;
#13906 = ADVANCED_FACE ( 'NONE', ( #52401 ), #7206, .F. ) ;
#13907 = FACE_OUTER_BOUND ( 'NONE', #39491, .T. ) ;
#13908 = FACE_OUTER_BOUND ( 'NONE', #99616, .T. ) ;
#13909 = EDGE_CURVE ( 'NONE', #71272, #9388, #6215, .T. ) ;
#13910 = CARTESIAN_POINT ( 'NONE',  ( -121.2228709571500644, -23.47596703998600631, 11.44779298504227860 ) ) ;
#13911 = CARTESIAN_POINT ( 'NONE',  ( -16.92291128558595048, 9.936001969431544012, -1.500000000000002220 ) ) ;
#13912 = EDGE_CURVE ( 'NONE', #11900, #31349, #98056, .T. ) ;
#13913 = DIRECTION ( 'NONE',  ( -0.000000000000000000, 0.000000000000000000, 1.000000000000000000 ) ) ;
#13914 = ORIENTED_EDGE ( 'NONE', *, *, #63816, .T. ) ;
#13915 = CARTESIAN_POINT ( 'NONE',  ( -5.754811884962036217, -20.78327508566754389, -1.500000000000002220 ) ) ;
#13916 = LINE ( 'NONE', #83428, #22031 ) ;
#13917 = EDGE_CURVE ( 'NONE', #2943, #48981, #76706, .T. ) ;
#13918 = CARTESIAN_POINT ( 'NONE',  ( -70.70074709382635092, -25.12219130706001735, 7.037036740594547091 ) ) ;
#13919 = CARTESIAN_POINT ( 'NONE',  ( -50.52287095715006160, -24.99132157543166599, 2.256160258750667502 ) ) ;
#13920 = CARTESIAN_POINT ( 'NONE',  ( -99.78454658038423020, -25.18439381177101311, 3.502964603859448633 ) ) ;
#13921 = CARTESIAN_POINT ( 'NONE',  ( 17.08057647167376913, 15.47633299359885761, -1.500000000000002220 ) ) ;
#13922 = CIRCLE ( 'NONE', #91706, 130.2784398600581710 ) ;
#13923 = DATE_TIME_ROLE ( 'creation_date' ) ;
#13924 = LINE ( 'NONE', #73840, #51523 ) ;
#13925 = CARTESIAN_POINT ( 'NONE',  ( -49.48969932074964362, -24.51314013834316086, 0.6176544820404130665 ) ) ;
#13926 = CARTESIAN_POINT ( 'NONE',  ( -20.08517628505838815, -1.856936949192496300, 11.49999999999999645 ) ) ;
#13927 = CARTESIAN_POINT ( 'NONE',  ( -109.1001591083545179, -25.10927551888114806, 3.548369107942201062 ) ) ;
#13928 = LINE ( 'NONE', #6325, #8010 ) ;
#13929 = VECTOR ( 'NONE', #85650, 1000.000000000000000 ) ;
#13931 = CARTESIAN_POINT ( 'NONE',  ( -46.52287095715004028, -24.34917612406836795, 0.1852690917426517980 ) ) ;
#13930 = VECTOR ( 'NONE', #91049, 1000.000000000000114 ) ;
#13932 = CARTESIAN_POINT ( 'NONE',  ( 0.000000000000000000, -7.835183881457442823, 0.000000000000000000 ) ) ;
#13933 = CARTESIAN_POINT ( 'NONE',  ( -38.62287095715005592, -24.64898659630528144, 1.056161002820819261 ) ) ;
#13934 = CARTESIAN_POINT ( 'NONE',  ( -0.2410636032128395945, 19.88167143085883737, -1.500000000000002220 ) ) ;
#13935 = CIRCLE ( 'NONE', #99822, 9.999999999999991118 ) ;
#13936 = CARTESIAN_POINT ( 'NONE',  ( -109.5562042904834072, -24.64898659630530275, 1.056161002820833472 ) ) ;
#13937 = CARTESIAN_POINT ( 'NONE',  ( 5.037983044326730386, -19.10262670698400100, -1.500000000000002220 ) ) ;
#13938 = AXIS2_PLACEMENT_3D ( 'NONE', #63405, #88228, #80600 ) ;
#13939 = CARTESIAN_POINT ( 'NONE',  ( -126.6237056494491924, -24.51419770103158413, 9.386484678747162747 ) ) ;
#13940 = CARTESIAN_POINT ( 'NONE',  ( -110.5228709571499763, -24.82576562948881715, 8.398263436605676091 ) ) ;
#13941 = DIRECTION ( 'NONE',  ( 1.000000000000000000, 0.000000000000000000, 0.000000000000000000 ) ) ;
#13942 = CARTESIAN_POINT ( 'NONE',  ( 15.29587703590233971, -13.95322596517325664, 11.49999999999999645 ) ) ;
#13943 = CARTESIAN_POINT ( 'NONE',  ( 0.3244565263465142291, -1.558659884777352067, -8.999999999999998224 ) ) ;
#13944 = CARTESIAN_POINT ( 'NONE',  ( 31.10634905326439181, 4.583458114012134210, -2.800232393899708683 ) ) ;
#13945 = CARTESIAN_POINT ( 'NONE',  ( -106.5947035255675814, -23.73766607897671577, -1.055555164236449572 ) ) ;
#13946 = CARTESIAN_POINT ( 'NONE',  ( -1.179572987637725889, 22.66035800735570049, 11.49999999999999645 ) ) ;
#13947 = ORIENTED_EDGE ( 'NONE', *, *, #93784, .T. ) ;
#13948 = CARTESIAN_POINT ( 'NONE',  ( -91.62287095715005592, -23.72747288104469376, -1.053458166803225682 ) ) ;
#13949 = CARTESIAN_POINT ( 'NONE',  ( 30.60993360729056079, 4.065030569019225659, 27.12046991540520580 ) ) ;
#13950 = CARTESIAN_POINT ( 'NONE',  ( 9.409760114191467295, 17.86087837679851020, -1.500000000000002220 ) ) ;
#13951 = CARTESIAN_POINT ( 'NONE',  ( 8.809764260727234841, -0.02602732333168140261, -3.697389739420774646 ) ) ;
#13952 = CARTESIAN_POINT ( 'NONE',  ( -106.5228709571500758, -29.50250786944525672, 11.44777988621622988 ) ) ;
#13953 = AXIS2_PLACEMENT_3D ( 'NONE', #76394, #37849, #23101 ) ;
#13954 = VERTEX_POINT ( 'NONE', #13820 ) ;
#13955 = B_SPLINE_CURVE_WITH_KNOTS ( 'NONE', 3,
 ( #22583, #29723, #84999, #53075, #21593, #15483 ),
 .UNSPECIFIED., .F., .F.,
 ( 4, 2, 4 ),
 ( 0.000000000000000000, 0.001380764517854765616, 0.002761529035709531232 ),
 .UNSPECIFIED. ) ;
#13956 = ORIENTED_EDGE ( 'NONE', *, *, #80369, .F. ) ;
#13957 = CARTESIAN_POINT ( 'NONE',  ( -0.3982818654701407723, -6.376774720514410077, 19.46306892155547530 ) ) ;
#13958 = CARTESIAN_POINT ( 'NONE',  ( 21.91704834537361180, 6.644925864936762849, -1.500000000000002220 ) ) ;
#13959 = CARTESIAN_POINT ( 'NONE',  ( -29.57433297125452754, -24.58015684836148296, 1.056161296257513982 ) ) ;
#13960 = CARTESIAN_POINT ( 'NONE',  ( -20.99440926880444636, 4.982473936180791263, -1.500000000000002220 ) ) ;
#13961 = CARTESIAN_POINT ( 'NONE',  ( -123.5552300364399798, -24.15543982623907482, -0.2315651400026561002 ) ) ;
#13962 = DIRECTION ( 'NONE',  ( 0.000000000000000000, -1.000000000000000000, 0.000000000000000000 ) ) ;
#13963 = CARTESIAN_POINT ( 'NONE',  ( 12.60132613692001691, 16.66296579206088069, 11.49999999999999645 ) ) ;
#13964 = ORIENTED_EDGE ( 'NONE', *, *, #84526, .T. ) ;
#13965 = CARTESIAN_POINT ( 'NONE',  ( -28.87341653796864804, -25.01351064681628245, 2.972253445286453744 ) ) ;
#13966 = CARTESIAN_POINT ( 'NONE',  ( 13.70243205411677145, -17.22335469805116048, -1.500000000000002220 ) ) ;
#13967 = EDGE_CURVE ( 'NONE', #37863, #66710, #26806, .T. ) ;
#13968 = DIRECTION ( 'NONE',  ( 0.000000000000000000, -1.000000000000000000, 0.000000000000000000 ) ) ;
#13969 = CARTESIAN_POINT ( 'NONE',  ( -41.77018777319382536, -25.10925950928115569, 3.672890040647070808 ) ) ;
#13970 = ORIENTED_EDGE ( 'NONE', *, *, #59755, .F. ) ;
#13971 = FACE_OUTER_BOUND ( 'NONE', #2192, .T. ) ;
#13972 = EDGE_CURVE ( 'NONE', #36478, #29598, #26875, .T. ) ;
#13973 = LINE ( 'NONE', #68276, #86739 ) ;
#13974 = ORIENTED_EDGE ( 'NONE', *, *, #5101, .F. ) ;
#13975 = CARTESIAN_POINT ( 'NONE',  ( -72.49891841213921850, -24.51419770103156281, 9.386484678747185839 ) ) ;
#13976 = ORIENTED_EDGE ( 'NONE', *, *, #21050, .T. ) ;
#13977 = EDGE_LOOP ( 'NONE', ( #53681, #15386, #34749, #92571 ) ) ;
#13978 = CARTESIAN_POINT ( 'NONE',  ( 2.750000000000001332, 26.59999999999999432, 2.100000000000000089 ) ) ;
#13979 = CARTESIAN_POINT ( 'NONE',  ( 13.91401389203221406, -3.316774720514426456, 158.0376437107427137 ) ) ;
#13980 = CARTESIAN_POINT ( 'NONE',  ( -57.59852009964687625, -23.96119346886880663, -0.6495511937832122440 ) ) ;
#13981 = CARTESIAN_POINT ( 'NONE',  ( 7.100489274569507181, 19.11111018586187527, -1.500000000000002220 ) ) ;
#13982 = ORIENTED_EDGE ( 'NONE', *, *, #44106, .T. ) ;
#13983 = CARTESIAN_POINT ( 'NONE',  ( -0.8502773128684013582, -5.876774720514413630, 19.61227901093089798 ) ) ;
#13984 = CARTESIAN_POINT ( 'NONE',  ( -30.59800378598952264, -24.75991027412949563, 1.063373454495736725 ) ) ;
#13985 = CARTESIAN_POINT ( 'NONE',  ( -4.177535645411178500, -6.376774720514415407, 20.17598923696320767 ) ) ;
#13986 = CARTESIAN_POINT ( 'NONE',  ( -25.57847374984697097, -24.89029040080884414, 5.862545262149446934 ) ) ;
#13987 = ORIENTED_EDGE ( 'NONE', *, *, #23244, .T. ) ;
#13988 = CARTESIAN_POINT ( 'NONE',  ( -99.62287095715005592, -23.47596703998600631, 11.44779298504227860 ) ) ;
#13989 = CARTESIAN_POINT ( 'NONE',  ( -29.39543059329891506, -25.26247846418970866, 7.191771738233368794 ) ) ;
#13990 = CARTESIAN_POINT ( 'NONE',  ( 19.16185898538474675, 8.078635803559651052, -1.500000000000002220 ) ) ;
#13991 = VERTEX_POINT ( 'NONE', #20433 ) ;
#13993 = VERTEX_POINT ( 'NONE', #43795 ) ;
#13992 = CARTESIAN_POINT ( 'NONE',  ( -25.92875734969026524, 3.316774720514426456, -0.08597719988137648983 ) ) ;
#13994 = CIRCLE ( 'NONE', #44793, 84.48086791635431325 ) ;
#13995 = CARTESIAN_POINT ( 'NONE',  ( -104.6228709571500559, -29.50247984919015209, -1.443849546365050029 ) ) ;
#13996 = EDGE_LOOP ( 'NONE', ( #40507, #96436, #98762, #31077 ) ) ;
#13997 = ORIENTED_EDGE ( 'NONE', *, *, #53233, .T. ) ;
#13998 = AXIS2_PLACEMENT_3D ( 'NONE', #51804, #35582, #89857 ) ;
#13999 = CARTESIAN_POINT ( 'NONE',  ( 30.32108885906865936, -6.376774720514426953, 3.274824222184972822 ) ) ;
#14000 = CARTESIAN_POINT ( 'NONE',  ( -29.49875734969025842, -5.965225279485572685, 17.86602280011862476 ) ) ;
#14001 = DIRECTION ( 'NONE',  ( 0.000000000000000000, -0.9999999999976377785, -2.173523156925979975E-06 ) ) ;
#14002 = VECTOR ( 'NONE', #26609, 1000.000000000000000 ) ;
#14003 = CARTESIAN_POINT ( 'NONE',  ( -80.58953762381673869, -25.00158670708909270, 2.256160236439166411 ) ) ;
#14004 = CARTESIAN_POINT ( 'NONE',  ( -92.60130859751525634, -23.48786465467241058, 11.44779295918254469 ) ) ;
#14005 = LINE ( 'NONE', #46465, #74059 ) ;
#14007 = ORIENTED_EDGE ( 'NONE', *, *, #89409, .F. ) ;
#14006 = CARTESIAN_POINT ( 'NONE',  ( 2.710298230372018669, -21.94706154713207980, 11.49999999999999645 ) ) ;
#14008 = PLANE ( 'NONE',  #71611 ) ;
#14009 = CARTESIAN_POINT ( 'NONE',  ( -22.43363504178351775, 2.973318333978472339, -1.500000000000002220 ) ) ;
#14010 = AXIS2_PLACEMENT_3D ( 'NONE', #8586, #17191, #15692 ) ;
#14012 = ORIENTED_EDGE ( 'NONE', *, *, #87134, .T. ) ;
#14011 = CARTESIAN_POINT ( 'NONE',  ( -28.70162415927573818, -24.97191045107068064, 7.134260916763030203 ) ) ;
#14013 = ORIENTED_EDGE ( 'NONE', *, *, #75886, .F. ) ;
#14014 = DIRECTION ( 'NONE',  ( -1.000000000000000000, 1.734723475976801178E-15, 0.000000000000000000 ) ) ;
#14015 = CARTESIAN_POINT ( 'NONE',  ( -7.807601069497579260, -18.53474111305376937, -1.500000000000002220 ) ) ;
#14016 = CARTESIAN_POINT ( 'NONE',  ( -9.607008362728935325, -21.85066016484769236, -1.443836447538997536 ) ) ;
#14017 = ORIENTED_EDGE ( 'NONE', *, *, #51529, .F. ) ;
#14018 = FACE_OUTER_BOUND ( 'NONE', #97366, .T. ) ;
#14019 = CARTESIAN_POINT ( 'NONE',  ( 10.24050353823403192, -19.87907451059620456, -1.500000000000002220 ) ) ;
#14020 = EDGE_LOOP ( 'NONE', ( #58663, #75626, #7240, #73800 ) ) ;
#14021 = ORIENTED_EDGE ( 'NONE', *, *, #60319, .F. ) ;
#14022 = CARTESIAN_POINT ( 'NONE',  ( 32.16024265030974050, -5.965225279485572685, 16.27760796525321751 ) ) ;
#14023 = DIRECTION ( 'NONE',  ( -1.000000000000000000, -3.773278334444167608E-23, -8.201307833595939069E-29 ) ) ;
#14024 = DIRECTION ( 'NONE',  ( -2.000709955812756421E-15, 6.669033186042521139E-15, -1.000000000000000000 ) ) ;
#14025 = VECTOR ( 'NONE', #46828, 1000.000000000000114 ) ;
#14026 = CARTESIAN_POINT ( 'NONE',  ( -96.62287095715012697, -23.96177878511309345, 10.65340807706330217 ) ) ;
#14027 = CARTESIAN_POINT ( 'NONE',  ( 19.09806219120973125, -4.162641619376711510, 11.49999999999998934 ) ) ;
#14028 = EDGE_CURVE ( 'NONE', #89948, #30324, #81958, .T. ) ;
#14029 = CARTESIAN_POINT ( 'NONE',  ( -119.6228709571500559, -29.50250786944525672, 11.44777988621622811 ) ) ;
#14030 = CARTESIAN_POINT ( 'NONE',  ( -8.943896628894790979, 19.53434260886740503, -1.500000000000002220 ) ) ;
#14031 = CIRCLE ( 'NONE', #91831, 3.060000000000001830 ) ;
#14032 = CARTESIAN_POINT ( 'NONE',  ( -2.188401442307694289, -6.376774720514411854, 19.46153846153846700 ) ) ;
#14033 = EDGE_CURVE ( 'NONE', #33348, #52199, #6820, .T. ) ;
#14034 = CARTESIAN_POINT ( 'NONE',  ( -120.5228709571500616, -24.83602698348161653, 1.605859176311263736 ) ) ;
#14035 = LINE ( 'NONE', #60739, #99444 ) ;
#14036 = CARTESIAN_POINT ( 'NONE',  ( -7.756741253720922380, -21.46081514045699024, -1.500000000000002220 ) ) ;
#14037 = PERSON_AND_ORGANIZATION ( #70597, #27821 ) ;
#14038 = CARTESIAN_POINT ( 'NONE',  ( -106.5596227115201344, -23.48786465467241769, 11.44779295918253403 ) ) ;
#14039 = LINE ( 'NONE', #67356, #39299 ) ;
#14040 = CARTESIAN_POINT ( 'NONE',  ( 19.63333621495807435, 3.783328549194958867, 11.49999999999999645 ) ) ;
#14041 = DIRECTION ( 'NONE',  ( 0.000000000000000000, -2.173523156925979552E-06, 0.9999999999976378895 ) ) ;
#14042 = FACE_OUTER_BOUND ( 'NONE', #28116, .T. ) ;
#14043 = PLANE ( 'NONE',  #57007 ) ;
#14044 = VERTEX_POINT ( 'NONE', #22911 ) ;
#14045 = ADVANCED_FACE ( 'NONE', ( #61524 ), #39164, .T. ) ;
#14046 = DIRECTION ( 'NONE',  ( 3.773278334444167608E-23, -1.000000000000000000, 0.000000000000000000 ) ) ;
#14047 = CARTESIAN_POINT ( 'NONE',  ( 10.46399479596398052, -3.316774720514422903, -27.03001098546561209 ) ) ;
#14048 = B_SPLINE_CURVE_WITH_KNOTS ( 'NONE', 3,
 ( #4881, #10991, #19092, #73399, #12485, #3894 ),
 .UNSPECIFIED., .F., .F.,
 ( 4, 2, 4 ),
 ( 0.000000000000000000, 0.001380764517853253371, 0.002761529035706506742 ),
 .UNSPECIFIED. ) ;
#14049 = CARTESIAN_POINT ( 'NONE',  ( 20.36105213711617878, 7.643125777291208678, -1.500000000000002220 ) ) ;
#14050 = CARTESIAN_POINT ( 'NONE',  ( -88.88918693012689687, -25.22391110550272941, 6.409327647371936720 ) ) ;
#14051 = CARTESIAN_POINT ( 'NONE',  ( 19.03533760385612439, 4.641190475545474037, -1.500000000000002220 ) ) ;
#14052 = CIRCLE ( 'NONE', #48043, 1.500000000000000666 ) ;
#14053 = CARTESIAN_POINT ( 'NONE',  ( -61.62287095715004881, -24.64898659630528854, 1.056161002820822592 ) ) ;
#14054 = B_SPLINE_CURVE_WITH_KNOTS ( 'NONE', 3,
 ( #68470, #84180, #38013, #22766, #23270, #53753 ),
 .UNSPECIFIED., .F., .F.,
 ( 4, 2, 4 ),
 ( 1.570887131794176733E-05, 0.001396322306279757170, 0.002776935741241572803 ),
 .UNSPECIFIED. ) ;
#14055 = ORIENTED_EDGE ( 'NONE', *, *, #12531, .T. ) ;
#14056 = APPROVAL_ROLE ( '' ) ;
#14057 = DIRECTION ( 'NONE',  ( -3.773278334453079618E-23, 0.9999999999976377785, 2.173523156925979975E-06 ) ) ;
#14058 = CARTESIAN_POINT ( 'NONE',  ( -124.5228709571500616, -23.47596703998600631, 11.44779298504227860 ) ) ;
#14059 = CARTESIAN_POINT ( 'NONE',  ( 4.362881659454829197, 20.01674633476859810, 11.49999999999999645 ) ) ;
#14060 = DIRECTION ( 'NONE',  ( 0.000000000000000000, -1.000000000000000000, 0.000000000000000000 ) ) ;
#14061 = CIRCLE ( 'NONE', #51379, 91.74549126261076992 ) ;
#14062 = CARTESIAN_POINT ( 'NONE',  ( -49.52287095715004739, -24.66019654487198665, 8.947790411086131712 ) ) ;
#14063 = ORIENTED_EDGE ( 'NONE', *, *, #82531, .F. ) ;
#14064 = CARTESIAN_POINT ( 'NONE',  ( -2.768609665556983845, 5.965225279485594001, -29.41086200512614823 ) ) ;
#14065 = CARTESIAN_POINT ( 'NONE',  ( -109.6228709571500559, -29.50250243563736774, 8.947779886222136270 ) ) ;
#14066 = AXIS2_PLACEMENT_3D ( 'NONE', #6410, #36860, #7390 ) ;
#14067 = CARTESIAN_POINT ( 'NONE',  ( -101.6228709571500559, -23.48783264082479505, -1.443836473390062380 ) ) ;
#14068 = AXIS2_PLACEMENT_3D ( 'NONE', #75902, #28745, #6407 ) ;
#14069 = DIRECTION ( 'NONE',  ( 0.000000000000000000, -0.9999999999976377785, -2.173523156925979975E-06 ) ) ;
#14070 = ORIENTED_EDGE ( 'NONE', *, *, #39641, .F. ) ;
#14071 = CARTESIAN_POINT ( 'NONE',  ( 32.56681547219513817, 5.361656835957732348, -1.802091617189351735 ) ) ;
#14072 = AXIS2_PLACEMENT_3D ( 'NONE', #82293, #59970, #12770 ) ;
#14073 = EDGE_CURVE ( 'NONE', #77832, #65146, #9725, .T. ) ;
#14074 = CARTESIAN_POINT ( 'NONE',  ( -10.32085834726444595, 20.65377284989807194, 11.49999999999999645 ) ) ;
#14075 = CARTESIAN_POINT ( 'NONE',  ( -12.29745307268338195, -19.16510367807413218, 11.49999999999998934 ) ) ;
#14076 = CARTESIAN_POINT ( 'NONE',  ( -110.5923908730569707, -24.15602025860899360, 10.28564288303534724 ) ) ;
#14077 = CARTESIAN_POINT ( 'NONE',  ( -88.52287095715009002, -23.48783264082477018, -1.443836473390089692 ) ) ;
#14078 = CARTESIAN_POINT ( 'NONE',  ( -77.52287095715006160, -29.50248528299804818, 1.056150453629038477 ) ) ;
#14079 = CARTESIAN_POINT ( 'NONE',  ( -2.899999999999996358, 33.29999999999999716, 0.000000000000000000 ) ) ;
#14080 = CARTESIAN_POINT ( 'NONE',  ( -110.6263928191107482, -24.63355581998384380, 0.9682620441943931011 ) ) ;
#14081 = CARTESIAN_POINT ( 'NONE',  ( -5.132426408838210108, -21.30661980433056968, -1.500000000000002220 ) ) ;
#14082 = ADVANCED_FACE ( 'NONE', ( #85332 ), #47291, .F. ) ;
#14083 = LINE ( 'NONE', #85103, #77004 ) ;
#14084 = CARTESIAN_POINT ( 'NONE',  ( -50.62287095715005592, -25.00158670708909625, 2.256160236439165967 ) ) ;
#14085 = LINE ( 'NONE', #37934, #22739 ) ;
#14086 = CARTESIAN_POINT ( 'NONE',  ( -78.60051294073809913, -23.73766607897670511, -1.055555164236459342 ) ) ;
#14087 = CARTESIAN_POINT ( 'NONE',  ( -94.62287095714998486, -24.51387760970725083, 9.387446482453411178 ) ) ;
#14088 = PLANE ( 'NONE',  #66471 ) ;
#14089 = ORIENTED_EDGE ( 'NONE', *, *, #65563, .T. ) ;
#14090 = B_SPLINE_CURVE_WITH_KNOTS ( 'NONE', 3,
 ( #38611, #16770, #69571, #22862 ),
 .UNSPECIFIED., .F., .F.,
 ( 4, 4 ),
 ( 0.9694772152566509815, 0.9704779622974166742 ),
 .UNSPECIFIED. ) ;
#14091 = CARTESIAN_POINT ( 'NONE',  ( 11.41020680648336771, 16.95828056793917682, -1.500000000000002220 ) ) ;
#14092 = EDGE_LOOP ( 'NONE', ( #56363, #65467, #74992, #60426 ) ) ;
#14093 = B_SPLINE_CURVE_WITH_KNOTS ( 'NONE', 3,
 ( #81362, #5231, #83344, #90468, #59033, #11843 ),
 .UNSPECIFIED., .F., .F.,
 ( 4, 2, 4 ),
 ( 0.000000000000000000, 0.001380764517853253588, 0.002761529035706507176 ),
 .UNSPECIFIED. ) ;
#14094 = ORIENTED_EDGE ( 'NONE', *, *, #90877, .F. ) ;
#14095 = ORIENTED_EDGE ( 'NONE', *, *, #23529, .T. ) ;
#14096 = EDGE_LOOP ( 'NONE', ( #20714, #14226, #81878, #9383 ) ) ;
#14097 = CARTESIAN_POINT ( 'NONE',  ( -21.75560140871883164, 7.562747417745157463, 11.49999999999998934 ) ) ;
#14098 = CARTESIAN_POINT ( 'NONE',  ( -35.52287095715006870, -25.00158670708909270, 2.256160236439166411 ) ) ;
#14099 = CARTESIAN_POINT ( 'NONE',  ( 18.19722386731275066, -8.884848157732822216, -1.500000000000002220 ) ) ;
#14100 = ORIENTED_EDGE ( 'NONE', *, *, #36750, .T. ) ;
#14101 = VECTOR ( 'NONE', #25983, 1000.000000000000000 ) ;
#14102 = CARTESIAN_POINT ( 'NONE',  ( -54.55620429048340014, -24.64965694238574656, 8.947790433994203596 ) ) ;
#14103 = CARTESIAN_POINT ( 'NONE',  ( -23.59123376470063960, 5.356774720514425603, 23.50402280011862288 ) ) ;
#14104 = DIRECTION ( 'NONE',  ( -3.773278334453080206E-23, 0.9999999999976377785, 2.173523156925979975E-06 ) ) ;
#14105 = CARTESIAN_POINT ( 'NONE',  ( -99.59917429406625899, -23.48786465467241413, 11.44779295918254292 ) ) ;
#14107 = ORIENTED_EDGE ( 'NONE', *, *, #57554, .T. ) ;
#14106 = CARTESIAN_POINT ( 'NONE',  ( -20.93543047832761417, 4.563121699532205255, 11.49999999999999645 ) ) ;
#14108 = CARTESIAN_POINT ( 'NONE',  ( -20.77875734969026311, 6.143225279485574397, 27.31649921512899937 ) ) ;
#14109 = CARTESIAN_POINT ( 'NONE',  ( -105.5228709571500616, -29.50249982740957577, 7.747779886224967605 ) ) ;
#14110 = ORIENTED_EDGE ( 'NONE', *, *, #78539, .T. ) ;
#14111 = VECTOR ( 'NONE', #42402, 1000.000000000000000 ) ;
#14112 = CARTESIAN_POINT ( 'NONE',  ( -19.90621922972506397, 5.769413876575915978, -1.500000000000002220 ) ) ;
#14113 = PRODUCT_DEFINITION ( 'UNKNOWN', '', #47237, #43907 ) ;
#14115 = ORIENTED_EDGE ( 'NONE', *, *, #31121, .F. ) ;
#14114 = FACE_OUTER_BOUND ( 'NONE', #89512, .T. ) ;
#14116 = CARTESIAN_POINT ( 'NONE',  ( -28.57983198641674250, -24.35651115837791281, 0.6176551810875500204 ) ) ;
#14117 = VERTEX_POINT ( 'NONE', #55409 ) ;
#14118 = CARTESIAN_POINT ( 'NONE',  ( 4.403244164709623654, -6.376774720514404748, 18.35516266052912826 ) ) ;
#14119 = VERTEX_POINT ( 'NONE', #69628 ) ;
#14120 = CARTESIAN_POINT ( 'NONE',  ( -5.787726610425443674, -20.20099407548119075, -1.500000000000002220 ) ) ;
#14121 = CARTESIAN_POINT ( 'NONE',  ( -21.86317675896206225, -2.224439152981679602, 11.49999999999999645 ) ) ;
#14122 = CARTESIAN_POINT ( 'NONE',  ( -73.59659219034413979, -23.96169478059713143, 10.65365249895718236 ) ) ;
#14123 = CARTESIAN_POINT ( 'NONE',  ( 6.936750662203477802, 21.44973376661030429, -1.500000000000002220 ) ) ;
#14124 = EDGE_CURVE ( 'NONE', #63088, #45647, #24437, .T. ) ;
#14125 = CARTESIAN_POINT ( 'NONE',  ( -13.85205798638896901, 15.75786377350088507, 11.49999999999998934 ) ) ;
#14126 = CARTESIAN_POINT ( 'NONE',  ( -23.29179552176161749, 5.965225279485594001, -17.29637630388738501 ) ) ;
#14127 = CARTESIAN_POINT ( 'NONE',  ( -89.23534077628077910, -25.26877915520014994, 5.947789088310639904 ) ) ;
#14128 = CARTESIAN_POINT ( 'NONE',  ( 6.326958800731953048, -6.376774720514426065, 21.47849181751607972 ) ) ;
#14129 = VERTEX_POINT ( 'NONE', #84837 ) ;
#14130 = ORIENTED_EDGE ( 'NONE', *, *, #36172, .F. ) ;
#14131 = EDGE_LOOP ( 'NONE', ( #69347, #4997, #87419, #19593 ) ) ;
#14132 = CARTESIAN_POINT ( 'NONE',  ( 0.000000000000000000, -5.356774720496559894, 19.84760796525321425 ) ) ;
#14133 = AXIS2_PLACEMENT_3D ( 'NONE', #18118, #49084, #41974 ) ;
#14134 = CARTESIAN_POINT ( 'NONE',  ( 21.44729954461699251, -1.519088741117538000, -1.500000000000002220 ) ) ;
#14135 = DIRECTION ( 'NONE',  ( -0.7512896232465891000, 0.000000000000000000, -0.6599726524652351767 ) ) ;
#14136 = VERTEX_POINT ( 'NONE', #15317 ) ;
#14137 = CARTESIAN_POINT ( 'NONE',  ( 5.126256225908648823, -20.47799061884807870, 11.49999999999998934 ) ) ;
#14138 = DIRECTION ( 'NONE',  ( -3.773278334453079618E-23, 0.9999999999976377785, 2.173523156925979975E-06 ) ) ;
#14139 = CARTESIAN_POINT ( 'NONE',  ( -64.54880478395197940, -24.15543982623906416, -0.2315651400026674800 ) ) ;
#14140 = CARTESIAN_POINT ( 'NONE',  ( -50.38822539166533687, -25.30267106383720943, 4.736250553104468075 ) ) ;
#14141 = VECTOR ( 'NONE', #61343, 1000.000000000000000 ) ;
#14142 = CARTESIAN_POINT ( 'NONE',  ( 13.80377080874918150, -6.475225279485574248, -27.21172484903264532 ) ) ;
#14143 = CARTESIAN_POINT ( 'NONE',  ( -100.2745382058950128, -25.11141107491615898, 2.838304805050361868 ) ) ;
#14144 = CARTESIAN_POINT ( 'NONE',  ( -5.973063517705734071, 21.31661749205449041, -1.500000000000002220 ) ) ;
#14145 = CARTESIAN_POINT ( 'NONE',  ( -81.59562844260206305, -23.96169478059713498, 10.65365249895718591 ) ) ;
#14146 = ADVANCED_FACE ( 'NONE', ( #93442 ), #47792, .F. ) ;
#14147 = ORIENTED_EDGE ( 'NONE', *, *, #55514, .T. ) ;
#14148 = CARTESIAN_POINT ( 'NONE',  ( -2.711489738547795625, -6.376774720514410077, 19.27798293355755632 ) ) ;
#14149 = CARTESIAN_POINT ( 'NONE',  ( -64.62287095715005592, -23.47593901973091235, -1.443836447539007972 ) ) ;
#14150 = PLANE ( 'NONE',  #27459 ) ;
#14151 = CARTESIAN_POINT ( 'NONE',  ( -100.5576102210739009, -23.85016227208580375, -0.8807180028928297544 ) ) ;
#14152 = CARTESIAN_POINT ( 'NONE',  ( -4.672984603565591755, -18.88948546680484242, -1.500000000000002220 ) ) ;
#14153 = ADVANCED_FACE ( 'NONE', ( #54903 ), #7713, .T. ) ;
#14154 = CARTESIAN_POINT ( 'NONE',  ( 18.99370601119529312, 9.851043883551550806, -1.500000000000002220 ) ) ;
#14155 = CARTESIAN_POINT ( 'NONE',  ( -64.62287095715005592, -24.65952944569304250, 1.056160979905695685 ) ) ;
#14156 = CARTESIAN_POINT ( 'NONE',  ( -90.25584321435293589, -25.31973986624387862, 5.294390042787146200 ) ) ;
#14157 = EDGE_CURVE ( 'NONE', #99250, #26538, #75829, .T. ) ;
#14158 = CARTESIAN_POINT ( 'NONE',  ( -123.5228709571500758, -24.50216790748205398, 0.6166512839542613866 ) ) ;
#14159 = CARTESIAN_POINT ( 'NONE',  ( -36.62287095715005592, -23.48786465467240347, 11.44779295918255180 ) ) ;
#14160 = CARTESIAN_POINT ( 'NONE',  ( -11.22117850230010738, 19.66027149220947123, -1.500000000000002220 ) ) ;
#14161 = ORIENTED_EDGE ( 'NONE', *, *, #93430, .T. ) ;
#14162 = FACE_OUTER_BOUND ( 'NONE', #13591, .T. ) ;
#14163 = CARTESIAN_POINT ( 'NONE',  ( -97.62287095715005592, -24.64898659630367916, 1.056161002820829697 ) ) ;
#14164 = CARTESIAN_POINT ( 'NONE',  ( -14.06767371131996214, 13.90018863433869889, 11.49999999999999645 ) ) ;
#14165 = DIRECTION ( 'NONE',  ( -0.2164396139380965756, 0.9762960071199346945, 0.000000000000000000 ) ) ;
#14166 = ORIENTED_EDGE ( 'NONE', *, *, #8188, .T. ) ;
#14167 = EDGE_CURVE ( 'NONE', #2990, #74103, #31046, .T. ) ;
#14168 = CARTESIAN_POINT ( 'NONE',  ( 3.509873074917118085, -0.3587747205144265483, 29.15869884040363758 ) ) ;
#14169 = DIRECTION ( 'NONE',  ( -1.000000000000000000, -1.413818403454611288E-16, 0.000000000000000000 ) ) ;
#14170 = CARTESIAN_POINT ( 'NONE',  ( -8.642975711230413083, 19.83371042614930957, 11.49999999999998934 ) ) ;
#14171 = VECTOR ( 'NONE', #74547, 1000.000000000000000 ) ;
#14172 = CARTESIAN_POINT ( 'NONE',  ( -27.53165725413984788, -24.78898537453293116, 7.599094992256131498 ) ) ;
#14173 = CARTESIAN_POINT ( 'NONE',  ( 1.664315604108443925, 19.36118569274438528, -1.500000000000002220 ) ) ;
#14174 = CARTESIAN_POINT ( 'NONE',  ( 9.402885806365684829, 5.965225279485572685, 29.04108526060719342 ) ) ;
#14175 = DIRECTION ( 'NONE',  ( 3.773278334444166432E-23, -1.000000000000000000, 0.000000000000000000 ) ) ;
#14176 = CARTESIAN_POINT ( 'NONE',  ( -12.28770250403618114, -15.54288071925545722, -1.500000000000002220 ) ) ;
#14177 = ORIENTED_EDGE ( 'NONE', *, *, #31922, .T. ) ;
#14178 = B_SPLINE_CURVE_WITH_KNOTS ( 'NONE', 3,
 ( #10241, #25968, #78235, #93970, #79244, #9743, #39685, #46812 ),
 .UNSPECIFIED., .F., .F.,
 ( 4, 2, 2, 4 ),
 ( -0.001224554619866334787, -0.0002241820295893544746, 0.0007761905606876258381, 0.002776935741241578007 ),
 .UNSPECIFIED. ) ;
#14179 = VECTOR ( 'NONE', #91796, 1000.000000000000114 ) ;
#14180 = CARTESIAN_POINT ( 'NONE',  ( -19.77321833943668850, 4.698914572609424134, 11.49999999999999645 ) ) ;
#14181 = CARTESIAN_POINT ( 'NONE',  ( -111.6228709571500417, -24.66019654487199730, 8.947790411086124607 ) ) ;
#14182 = CARTESIAN_POINT ( 'NONE',  ( -46.55620429048339304, -24.66019654487198665, 8.947790411086135265 ) ) ;
#14183 = B_SPLINE_CURVE_WITH_KNOTS ( 'NONE', 3,
 ( #57049, #64169, #16959, #47923, #25575, #56044 ),
 .UNSPECIFIED., .F., .F.,
 ( 4, 2, 4 ),
 ( 0.000000000000000000, 0.001380901958385389412, 0.002761803916770778824 ),
 .UNSPECIFIED. ) ;
#14184 = ORIENTED_EDGE ( 'NONE', *, *, #5215, .T. ) ;
#14185 = CARTESIAN_POINT ( 'NONE',  ( -30.62200344337180269, -24.13759587396042150, -0.5132947483565730717 ) ) ;
#14186 = DIRECTION ( 'NONE',  ( -3.773278334453079030E-23, 0.9999999999976377785, 2.173523156925979128E-06 ) ) ;
#14187 = CARTESIAN_POINT ( 'NONE',  ( 22.02124265030973760, 7.743225279485574042, 16.20402280011862217 ) ) ;
#14188 = DIRECTION ( 'NONE',  ( 0.000000000000000000, 1.000000000000000000, -1.084202172485504434E-16 ) ) ;
#14189 = CARTESIAN_POINT ( 'NONE',  ( 29.73860345376319358, -5.356774720496559894, -0.3523920347288969079 ) ) ;
#14190 = CARTESIAN_POINT ( 'NONE',  ( -19.74138705131307248, -3.616033589355840849, 11.49999999999998934 ) ) ;
#14191 = DIRECTION ( 'NONE',  ( 0.1478094111296165969, -0.9890158633619159367, 0.000000000000000000 ) ) ;
#14192 = ORIENTED_EDGE ( 'NONE', *, *, #71929, .T. ) ;
#14193 = CYLINDRICAL_SURFACE ( 'NONE', #34960, 3.570000000000003837 ) ;
#14194 = VECTOR ( 'NONE', #93794, 1000.000000000000000 ) ;
#14195 = CARTESIAN_POINT ( 'NONE',  ( -21.78311099772515647, -6.823855485095160489, 11.49999999999999645 ) ) ;
#14196 = CARTESIAN_POINT ( 'NONE',  ( -102.5228709571500332, -23.94994826722564696, -0.6494450866342718065 ) ) ;
#14197 = CARTESIAN_POINT ( 'NONE',  ( -111.9545715455114987, -25.05712135967895193, 7.447789548357302891 ) ) ;
#14198 = CARTESIAN_POINT ( 'NONE',  ( -114.6228709571500417, -24.65952944569305316, 1.056160979905703234 ) ) ;
#14199 = CARTESIAN_POINT ( 'NONE',  ( 5.641653616409716854, -5.876774720514420736, 20.81030773351227481 ) ) ;
#14200 = VECTOR ( 'NONE', #37209, 1000.000000000000000 ) ;
#14201 = CARTESIAN_POINT ( 'NONE',  ( -15.87499999999997868, 0.000000000000000000, 2.349999999999999645 ) ) ;
#14202 = EDGE_CURVE ( 'NONE', #86782, #32836, #92942, .T. ) ;
#14203 = DIRECTION ( 'NONE',  ( -0.06283980576413539243, 0.000000000000000000, -0.9980236263794188822 ) ) ;
#14204 = ORIENTED_EDGE ( 'NONE', *, *, #50857, .T. ) ;
#14205 = AXIS2_PLACEMENT_3D ( 'NONE', #78549, #87684, #24769 ) ;
#14206 = CARTESIAN_POINT ( 'NONE',  ( 8.194921280291850962, -18.63391395107102610, -1.500000000000002220 ) ) ;
#14207 = EDGE_LOOP ( 'NONE', ( #53184, #48051, #49853, #4882 ) ) ;
#14208 = B_SPLINE_CURVE_WITH_KNOTS ( 'NONE', 3,
 ( #5945, #21655, #14554, #61256 ),
 .UNSPECIFIED., .F., .F.,
 ( 4, 4 ),
 ( 0.000000000000000000, 9.999999999997510880E-05 ),
 .UNSPECIFIED. ) ;
#14209 = CARTESIAN_POINT ( 'NONE',  ( 22.43992371924722917, 4.826111843257130829, -1.500000000000002220 ) ) ;
#14210 = CARTESIAN_POINT ( 'NONE',  ( -95.62287095715005592, -29.50248789122583659, 2.256150453626215580 ) ) ;
#14211 = EDGE_LOOP ( 'NONE', ( #9609, #56190, #35381, #39704 ) ) ;
#14212 = CARTESIAN_POINT ( 'NONE',  ( -101.6228709571500559, -24.64965695001469115, 8.947790433994178727 ) ) ;
#14213 = CARTESIAN_POINT ( 'NONE',  ( -77.60072532662823619, -23.73791477778911840, 11.05961554403170588 ) ) ;
#14214 = CARTESIAN_POINT ( 'NONE',  ( -89.62287095715004170, -24.65952944569305316, 1.056160979905700348 ) ) ;
#14216 = ORIENTED_EDGE ( 'NONE', *, *, #88571, .T. ) ;
#14215 = CARTESIAN_POINT ( 'NONE',  ( -21.25539211000977957, 0.9166567589900279645, 11.49999999999999645 ) ) ;
#14217 = VERTEX_POINT ( 'NONE', #70621 ) ;
#14218 = CARTESIAN_POINT ( 'NONE',  ( 10.53326394202159300, -19.55463526559320542, 11.49999999999998934 ) ) ;
#14219 = CARTESIAN_POINT ( 'NONE',  ( -16.41017380093149214, -12.48182641202616416, 11.49999999999998934 ) ) ;
#14220 = B_SPLINE_CURVE_WITH_KNOTS ( 'NONE', 3,
 ( #15605, #77497, #86625, #7998, #17110, #32338 ),
 .UNSPECIFIED., .F., .F.,
 ( 4, 2, 4 ),
 ( 0.000000000000000000, 0.001380764517854763665, 0.002761529035709527329 ),
 .UNSPECIFIED. ) ;
#14221 = EDGE_CURVE ( 'NONE', #70995, #69928, #49518, .T. ) ;
#14222 = EDGE_LOOP ( 'NONE', ( #272, #51177, #9567, #100085 ) ) ;
#14223 = VERTEX_POINT ( 'NONE', #94455 ) ;
#14224 = DIRECTION ( 'NONE',  ( 3.773278334444167608E-23, -1.000000000000000000, 0.000000000000000000 ) ) ;
#14225 = CARTESIAN_POINT ( 'NONE',  ( 3.181132013147180970, -5.876774720514426065, 21.64201922499777808 ) ) ;
#14226 = ORIENTED_EDGE ( 'NONE', *, *, #60816, .F. ) ;
#14227 = EDGE_CURVE ( 'NONE', #17879, #16795, #66162, .T. ) ;
#14228 = VERTEX_POINT ( 'NONE', #24938 ) ;
#14229 = CARTESIAN_POINT ( 'NONE',  ( -125.2170248000532240, -25.23482019547912714, 3.690485340690513372 ) ) ;
#14230 = CARTESIAN_POINT ( 'NONE',  ( -39.62287095715005592, -24.64965695001468404, 8.947790433994187609 ) ) ;
#14231 = CARTESIAN_POINT ( 'NONE',  ( 17.18838054715250152, -11.71887806637979779, -1.500000000000002220 ) ) ;
#14232 = CARTESIAN_POINT ( 'NONE',  ( 3.468383421097696928, -21.53508805063734854, 11.49999999999999645 ) ) ;
#14233 = CARTESIAN_POINT ( 'NONE',  ( -40.41683116089613748, -25.27806139858977375, 5.082404452748810364 ) ) ;
#14234 = CARTESIAN_POINT ( 'NONE',  ( 29.73860345376319003, -14.82721238576461609, -4.021180035027960287 ) ) ;
#14235 = VECTOR ( 'NONE', #25254, 1000.000000000000000 ) ;
#14236 = CARTESIAN_POINT ( 'NONE',  ( 12.99221220249228281, -18.32192329980629708, 11.49999999999998934 ) ) ;
#14237 = EDGE_CURVE ( 'NONE', #78402, #78496, #75412, .T. ) ;
#14238 = EDGE_CURVE ( 'NONE', #25844, #47437, #41692, .T. ) ;
#14239 = DIRECTION ( 'NONE',  ( 0.4009304992412300872, 0.000000000000000000, 0.9161084732596779245 ) ) ;
#14240 = ORIENTED_EDGE ( 'NONE', *, *, #89824, .T. ) ;
#14241 = DIRECTION ( 'NONE',  ( 0.000000000000000000, 0.000000000000000000, 1.000000000000000000 ) ) ;
#14242 = LINE ( 'NONE', #37093, #76652 ) ;
#14243 = B_SPLINE_SURFACE_WITH_KNOTS ( 'NONE', 3, 3, ( 
 ( #43127, #49255, #65487, #96406 ),
 ( #19764, #73575, #50740, #95903 ),
 ( #34514, #96906, #74076, #56369 ),
 ( #4568, #35517, #27400, #33508 ),
 ( #25392, #64492, #10171, #95408 ),
 ( #80183, #58359, #10673, #41636 ),
 ( #80680, #42143, #26894, #21758 ) ),
 .UNSPECIFIED., .F., .F., .F.,
 ( 4, 3, 4 ),
 ( 4, 4 ),
 ( 0.7945040050992248082, 0.8970133687736505657, 0.9995227324480764342 ),
 ( 0.6796667099735372863, 0.6809932137839499466 ),
 .UNSPECIFIED. ) ;
#14244 = EDGE_CURVE ( 'NONE', #93778, #13213, #73516, .T. ) ;
#14245 = ORIENTED_EDGE ( 'NONE', *, *, #62064, .F. ) ;
#14246 = ORIENTED_EDGE ( 'NONE', *, *, #16136, .T. ) ;
#14247 = PLANE ( 'NONE',  #27973 ) ;
#14248 = VERTEX_POINT ( 'NONE', #64043 ) ;
#14249 = CARTESIAN_POINT ( 'NONE',  ( -6.767052838139933080, -20.26514109264706676, -1.500000000000002220 ) ) ;
#14250 = ORIENTED_EDGE ( 'NONE', *, *, #26109, .F. ) ;
#14251 = CARTESIAN_POINT ( 'NONE',  ( -6.720452724358975338, -5.876774720514411854, 19.46153846153846700 ) ) ;
#14252 = CARTESIAN_POINT ( 'NONE',  ( 8.881738082190086203, 19.07353979602852689, -1.500000000000002220 ) ) ;
#14253 = CARTESIAN_POINT ( 'NONE',  ( -30.64649553399479132, -23.48778889868011177, -1.443836490256471983 ) ) ;
#14254 = CARTESIAN_POINT ( 'NONE',  ( -55.58953762381673869, -23.47593901973091235, -1.443836447539007972 ) ) ;
#14255 = PLANE ( 'NONE',  #30404 ) ;
#14256 = CARTESIAN_POINT ( 'NONE',  ( 9.607415760296678542, -19.69187540195887465, -1.500000000000002220 ) ) ;
#14257 = CARTESIAN_POINT ( 'NONE',  ( -4.686006777320704586, -6.376774720514426953, 29.60911411231905888 ) ) ;
#14258 = ORIENTED_EDGE ( 'NONE', *, *, #37, .T. ) ;
#14259 = CARTESIAN_POINT ( 'NONE',  ( -122.6244483497931554, -24.35071581493544102, 9.817618358456019934 ) ) ;
#14260 = ADVANCED_FACE ( 'NONE', ( #74124 ), #73132, .T. ) ;
#14261 = AXIS2_PLACEMENT_3D ( 'NONE', #83048, #97787, #90181 ) ;
#14262 = CARTESIAN_POINT ( 'NONE',  ( -84.55097372852188187, -24.15620529776628445, 10.23563542870660292 ) ) ;
#14263 = CARTESIAN_POINT ( 'NONE',  ( -128.5228709571501327, -24.51283580621458213, 0.6167428607047164002 ) ) ;
#14264 = CARTESIAN_POINT ( 'NONE',  ( -20.39835522263757639, -24.35407914423024067, 7.291654623549836955 ) ) ;
#14265 = CARTESIAN_POINT ( 'NONE',  ( -7.839647760473957838, 19.78794240023834661, 11.49999999999998934 ) ) ;
#14266 = CARTESIAN_POINT ( 'NONE',  ( -55.62287095715007723, -24.83620972994591725, 8.398175272781369216 ) ) ;
#14267 = CARTESIAN_POINT ( 'NONE',  ( -103.6228709571500417, -24.65952944569304606, 1.056160979905701680 ) ) ;
#14268 = ADVANCED_FACE ( 'NONE', ( #11712 ), #25947, .T. ) ;
#14269 = CARTESIAN_POINT ( 'NONE',  ( 14.44544951633968566, -3.759487683616679288, -28.33948095063585271 ) ) ;
#14270 = VECTOR ( 'NONE', #74720, 1000.000000000000114 ) ;
#14271 = CARTESIAN_POINT ( 'NONE',  ( -33.61928056205821491, -23.48783264082477729, -1.443836473390078368 ) ) ;
#14272 = CARTESIAN_POINT ( 'NONE',  ( -8.346146134265904237, -20.86121191590761015, -1.500000000000002220 ) ) ;
#14273 = ADVANCED_FACE ( 'NONE', ( #79725 ), #57421, .T. ) ;
#14275 = DIRECTION ( 'NONE',  ( -0.000000000000000000, -1.000000000000000000, -0.000000000000000000 ) ) ;
#14274 = B_SPLINE_CURVE_WITH_KNOTS ( 'NONE', 3,
 ( #37300, #90577, #82953, #21549 ),
 .UNSPECIFIED., .F., .F.,
 ( 4, 4 ),
 ( 0.000000000000000000, 9.999999999998897304E-05 ),
 .UNSPECIFIED. ) ;
#14276 = VERTEX_POINT ( 'NONE', #43184 ) ;
#14277 = CARTESIAN_POINT ( 'NONE',  ( -72.58953762381672448, -23.48783264082478084, -1.443836473390067265 ) ) ;
#14278 = CARTESIAN_POINT ( 'NONE',  ( -19.13235715846047214, 4.354950445902704637, 11.49999999999999645 ) ) ;
#14279 = CARTESIAN_POINT ( 'NONE',  ( -68.62287095715005592, -24.64898659630367916, 1.056161002820824368 ) ) ;
#14280 = CIRCLE ( 'NONE', #79114, 3.500000000000000000 ) ;
#14281 = DIRECTION ( 'NONE',  ( 0.7512896232465891000, 0.000000000000000000, 0.6599726524652351767 ) ) ;
#14282 = VERTEX_POINT ( 'NONE', #72636 ) ;
#14283 = ADVANCED_FACE ( 'NONE', ( #33066 ), #94957, .T. ) ;
#14284 = CARTESIAN_POINT ( 'NONE',  ( -70.09875394134060400, -25.30475096868035223, 4.859099491364304413 ) ) ;
#14285 = CARTESIAN_POINT ( 'NONE',  ( -84.58953762381672448, -23.47593901973091235, -1.443836447539004642 ) ) ;
#14286 = CARTESIAN_POINT ( 'NONE',  ( -88.87045360978522979, -25.25787539255926717, 3.590294762828090125 ) ) ;
#14288 = ADVANCED_FACE ( 'NONE', ( #10223 ), #89964, .T. ) ;
#14287 = CARTESIAN_POINT ( 'NONE',  ( 20.57455539870830208, -4.132774720514426292, -18.22080502500661581 ) ) ;
#14289 = CARTESIAN_POINT ( 'NONE',  ( -13.01991350253972080, 14.82018230214031895, 11.49999999999998934 ) ) ;
#14290 = EDGE_CURVE ( 'NONE', #53455, #65243, #17805, .T. ) ;
#14291 = AXIS2_PLACEMENT_3D ( 'NONE', #56904, #64530, #33046 ) ;
#14292 = VERTEX_POINT ( 'NONE', #88859 ) ;
#14293 = DIRECTION ( 'NONE',  ( -3.773278334453079618E-23, 0.9999999999976377785, 2.173523156925978705E-06 ) ) ;
#14294 = CARTESIAN_POINT ( 'NONE',  ( -73.52287095715007581, -29.50250786944525672, 11.44777988621623699 ) ) ;
#14295 = PERSON_AND_ORGANIZATION ( #70597, #27821 ) ;
#14296 = VERTEX_POINT ( 'NONE', #22310 ) ;
#14297 = FACE_OUTER_BOUND ( 'NONE', #71910, .T. ) ;
#14298 = DIRECTION ( 'NONE',  ( 0.9952638024365005887, 0.000000000000000000, 0.09721092304694053943 ) ) ;
#14299 = DIRECTION ( 'NONE',  ( -0.000000000000000000, 0.000000000000000000, 1.000000000000000000 ) ) ;
#14300 = CARTESIAN_POINT ( 'NONE',  ( -99.00488046896290939, -25.03144984087232316, 6.667020479340355799 ) ) ;
#14301 = CARTESIAN_POINT ( 'NONE',  ( -7.294102189209645815, -6.376774720514413630, 19.89644244529368677 ) ) ;
#14302 = B_SPLINE_CURVE_WITH_KNOTS ( 'NONE', 3,
 ( #53051, #59163, #35329, #60172, #6366, #58658, #13965, #90107, #43933, #5863, #97713, #29698, #21080, #99198, #52543, #12966 ),
 .UNSPECIFIED., .F., .F.,
 ( 4, 2, 2, 2, 2, 2, 2, 4 ),
 ( 8.673617379884034509E-19, 0.0008744097536164322079, 0.001748819507232863548, 0.002186024384041078406, 0.002623229260849293479, 0.003060434137657508120, 0.003279036576061615440, 0.003497639014465723194 ),
 .UNSPECIFIED. ) ;
#14303 = CARTESIAN_POINT ( 'NONE',  ( -70.06086327669997615, -25.24515049912487186, 5.348962429823249209 ) ) ;
#14304 = CARTESIAN_POINT ( 'NONE',  ( -112.5228709571500616, -23.47593901973090524, -1.443836447538996426 ) ) ;
#14305 = CARTESIAN_POINT ( 'NONE',  ( 16.79232260237064978, 10.84791536263152523, 11.49999999999998934 ) ) ;
#14306 = CARTESIAN_POINT ( 'NONE',  ( -27.68651082257923335, -29.50248793196339747, 2.274893084117591613 ) ) ;
#14307 = DIRECTION ( 'NONE',  ( -1.000000000000000000, -3.773278334444167608E-23, -8.201307816334959825E-29 ) ) ;
#14308 = ORIENTED_EDGE ( 'NONE', *, *, #27441, .T. ) ;
#14309 = CARTESIAN_POINT ( 'NONE',  ( 6.184520403203634942, -6.376774720514426953, -25.32021290018218451 ) ) ;
#14310 = CARTESIAN_POINT ( 'NONE',  ( -119.6274264067609323, -23.73766607897670511, -1.055555164236450238 ) ) ;
#14311 = CARTESIAN_POINT ( 'NONE',  ( -80.52209456291633671, -23.48786465467241058, 11.44779295918254824 ) ) ;
#14312 = LINE ( 'NONE', #51904, #64022 ) ;
#14313 = CARTESIAN_POINT ( 'NONE',  ( -81.59192521434273715, -24.15543982623907482, -0.2315651400026469686 ) ) ;
#14314 = DIRECTION ( 'NONE',  ( 3.469446951953614189E-15, -1.000000000000000000, 0.000000000000000000 ) ) ;
#14315 = CARTESIAN_POINT ( 'NONE',  ( -1.363607173041644582, -6.376774720514420736, 20.50445910983877340 ) ) ;
#14316 = B_SPLINE_SURFACE_WITH_KNOTS ( 'NONE', 3, 3, ( 
 ( #82750, #73652, #50820, #66066 ),
 ( #51315, #97964, #57449, #88378 ),
 ( #12232, #97483, #43213, #43702 ),
 ( #74151, #81259, #88885, #50323 ),
 ( #18859, #58929, #42719, #4644 ),
 ( #36087, #28463, #4145, #49836 ),
 ( #59428, #35599, #5133, #82255 ) ),
 .UNSPECIFIED., .F., .F., .F.,
 ( 4, 3, 4 ),
 ( 4, 4 ),
 ( 0.7945040049422250616, 0.8970133707663761058, 0.9995227365905272610 ),
 ( 0.06486256430468022305, 0.06976587085265167909 ),
 .UNSPECIFIED. ) ;
#14317 = DIRECTION ( 'NONE',  ( 0.000000000000000000, 0.000000000000000000, -1.000000000000000000 ) ) ;
#14318 = DIRECTION ( 'NONE',  ( -3.773278334444166432E-23, 1.000000000000000000, 0.000000000000000000 ) ) ;
#14319 = ORIENTED_EDGE ( 'NONE', *, *, #20047, .T. ) ;
#14320 = CARTESIAN_POINT ( 'NONE',  ( -19.75413285895528404, 4.560271753130525241, -1.500000000000002220 ) ) ;
#14321 = CARTESIAN_POINT ( 'NONE',  ( -122.5564249815854083, -23.73766607897671221, -1.055555164236450461 ) ) ;
#14322 = DIRECTION ( 'NONE',  ( 3.773278334444166432E-23, -1.000000000000000000, 0.000000000000000000 ) ) ;
#14323 = B_SPLINE_CURVE_WITH_KNOTS ( 'NONE', 3,
 ( #79451, #63761, #30779, #61749 ),
 .UNSPECIFIED., .F., .F.,
 ( 4, 4 ),
 ( 0.000000000000000000, 9.999999999998900014E-05 ),
 .UNSPECIFIED. ) ;
#14324 = VECTOR ( 'NONE', #28297, 1000.000000000000000 ) ;
#14325 = DIRECTION ( 'NONE',  ( 0.000000000000000000, 0.9999999999976377785, 2.173523156925979975E-06 ) ) ;
#14326 = ORIENTED_EDGE ( 'NONE', *, *, #37403, .F. ) ;
#14327 = CARTESIAN_POINT ( 'NONE',  ( -92.62287095715005592, -29.50250243563736774, 8.947779886222139822 ) ) ;
#14328 = PLANE ( 'NONE',  #6533 ) ;
#14329 = CARTESIAN_POINT ( 'NONE',  ( 8.649182803842551337, -18.14983140373652404, -1.500000000000002220 ) ) ;
#14330 = CARTESIAN_POINT ( 'NONE',  ( -1.165634184549018126, -21.02984315360824752, 11.49999999999999645 ) ) ;
#14331 = CARTESIAN_POINT ( 'NONE',  ( -83.52287095715006160, -29.50247984919015209, -1.443849546365053582 ) ) ;
#14332 = CARTESIAN_POINT ( 'NONE',  ( -22.12685673520133989, -0.1325007643398395663, 11.49999999999998934 ) ) ;
#14333 = CARTESIAN_POINT ( 'NONE',  ( 8.954683214801249846, 18.48387022957959047, -1.500000000000002220 ) ) ;
#14334 = CARTESIAN_POINT ( 'NONE',  ( 32.16024265030974050, -5.965225279485572685, 16.27760796525321751 ) ) ;
#14335 = ADVANCED_FACE ( 'NONE', ( #60413 ), #98944, .T. ) ;
#14336 = CARTESIAN_POINT ( 'NONE',  ( -53.62287095715006302, -24.51283580621364422, 0.6167428607019741493 ) ) ;
#14337 = ORIENTED_EDGE ( 'NONE', *, *, #8058, .F. ) ;
#14338 = DIRECTION ( 'NONE',  ( 0.000000000000000000, -0.9999999999976377785, -2.173523156925979975E-06 ) ) ;
#14339 = ORIENTED_EDGE ( 'NONE', *, *, #10467, .T. ) ;
#14340 = CARTESIAN_POINT ( 'NONE',  ( -47.52287095715006160, -23.48783264083458988, -1.443836473374825236 ) ) ;
#14341 = CARTESIAN_POINT ( 'NONE',  ( -102.6228709571500559, -23.47596703998600631, 11.44779298504227683 ) ) ;
#14342 = EDGE_CURVE ( 'NONE', #74207, #57442, #59395, .T. ) ;
#14343 = ORIENTED_EDGE ( 'NONE', *, *, #78208, .T. ) ;
#14344 = AXIS2_PLACEMENT_3D ( 'NONE', #48677, #47667, #31430 ) ;
#14345 = ORIENTED_EDGE ( 'NONE', *, *, #64057, .F. ) ;
#14346 = DIRECTION ( 'NONE',  ( -3.773278334444167608E-23, 1.000000000000000000, 0.000000000000000000 ) ) ;
#14347 = CARTESIAN_POINT ( 'NONE',  ( -5.576923076923074873, -5.876774720514426953, 21.75000000000000711 ) ) ;
#14348 = CARTESIAN_POINT ( 'NONE',  ( -68.62364079698707542, -24.66019654487199375, 8.947790411086122830 ) ) ;
#14349 = CARTESIAN_POINT ( 'NONE',  ( -20.66316395829706209, -0.6310838753663271516, -1.500000000000002220 ) ) ;
#14350 = CARTESIAN_POINT ( 'NONE',  ( 10.40854797073303395, 18.91789161722374146, 11.49999999999999645 ) ) ;
#14351 = ORIENTED_EDGE ( 'NONE', *, *, #56955, .F. ) ;
#14352 = PLANE ( 'NONE',  #66113 ) ;
#14353 = CARTESIAN_POINT ( 'NONE',  ( -96.58953762381671027, -24.64965694238407323, 8.947790433994649462 ) ) ;
#14354 = CARTESIAN_POINT ( 'NONE',  ( 21.65046080595755740, -5.567969076317650590, 11.49999999999998934 ) ) ;
#14355 = ADVANCED_FACE ( 'NONE', ( #58899 ), #44175, .T. ) ;
#14356 = EDGE_CURVE ( 'NONE', #30864, #45617, #6102, .T. ) ;
#14357 = CARTESIAN_POINT ( 'NONE',  ( -48.55620429048339304, -23.48786465467240703, 11.44779295918255357 ) ) ;
#14358 = FACE_OUTER_BOUND ( 'NONE', #28228, .T. ) ;
#14359 = ORIENTED_EDGE ( 'NONE', *, *, #79148, .T. ) ;
#14360 = DIRECTION ( 'NONE',  ( 0.000000000000000000, 0.000000000000000000, -1.000000000000000000 ) ) ;
#14361 = CARTESIAN_POINT ( 'NONE',  ( -49.48507484674644274, -24.66019654487198665, 8.947790411086131712 ) ) ;
#14362 = B_SPLINE_CURVE_WITH_KNOTS ( 'NONE', 3,
 ( #89122, #42956, #19094, #4883, #36829, #73892 ),
 .UNSPECIFIED., .F., .F.,
 ( 4, 2, 4 ),
 ( 0.000000000000000000, 0.001380764517853249685, 0.002761529035706499369 ),
 .UNSPECIFIED. ) ;
#14363 = ADVANCED_FACE ( 'NONE', ( #66544 ), #5103, .T. ) ;
#14364 = CARTESIAN_POINT ( 'NONE',  ( -19.40664508603899563, 7.695215611089875729, -1.500000000000002220 ) ) ;
#14365 = VERTEX_POINT ( 'NONE', #76101 ) ;
#14367 = EDGE_LOOP ( 'NONE', ( #96548, #78755, #11986, #63475 ) ) ;
#14366 = CARTESIAN_POINT ( 'NONE',  ( -86.55835945172226786, -23.73766607897671221, -1.055555164236433141 ) ) ;
#14368 = ORIENTED_EDGE ( 'NONE', *, *, #61154, .T. ) ;
#14369 = CARTESIAN_POINT ( 'NONE',  ( -109.5591694646261658, -23.48786465467241769, 11.44779295918253759 ) ) ;
#14370 = CARTESIAN_POINT ( 'NONE',  ( 17.90021246794804810, -11.17811638239879279, -1.500000000000002220 ) ) ;
#14371 = ORIENTED_EDGE ( 'NONE', *, *, #18729, .F. ) ;
#14372 = CARTESIAN_POINT ( 'NONE',  ( -101.9507253916653440, -25.24282061761981666, 6.236250683194342059 ) ) ;
#14373 = CARTESIAN_POINT ( 'NONE',  ( -100.0836892525862254, -25.12215667151522425, 7.064315935744911457 ) ) ;
#14374 = CARTESIAN_POINT ( 'NONE',  ( 6.392671032147439369, 20.83241601264130693, 11.49999999999998934 ) ) ;
#14375 = FACE_OUTER_BOUND ( 'NONE', #55954, .T. ) ;
#14376 = CARTESIAN_POINT ( 'NONE',  ( -81.58953762381673869, -24.64898659630528854, 1.056161002820825923 ) ) ;
#14377 = CARTESIAN_POINT ( 'NONE',  ( 7.433267315672343223, -5.876774720514418071, 20.43888261666079842 ) ) ;
#14378 = CARTESIAN_POINT ( 'NONE',  ( 21.56942612084361599, 2.798134137018522427, -1.500000000000002220 ) ) ;
#14379 = CARTESIAN_POINT ( 'NONE',  ( -0.6735982426299428338, -6.376774720514410077, 19.16400979764068069 ) ) ;
#14381 = VERTEX_POINT ( 'NONE', #29935 ) ;
#14380 = CARTESIAN_POINT ( 'NONE',  ( 21.63714550250683644, -5.416328558471028565, 11.49999999999999645 ) ) ;
#14382 = CARTESIAN_POINT ( 'NONE',  ( -33.52287095715004739, -23.96127896942118696, -0.6493128930941889365 ) ) ;
#14383 = LINE ( 'NONE', #53969, #3826 ) ;
#14384 = ADVANCED_FACE ( 'NONE', ( #36054 ), #13198, .F. ) ;
#14385 = CARTESIAN_POINT ( 'NONE',  ( 32.51008598047019404, -5.548342165039966467, -1.163674249303449315 ) ) ;
#14386 = VERTEX_POINT ( 'NONE', #82723 ) ;
#14387 = ORIENTED_EDGE ( 'NONE', *, *, #4429, .F. ) ;
#14388 = EDGE_CURVE ( 'NONE', #6499, #97248, #90342, .T. ) ;
#14389 = VERTEX_POINT ( 'NONE', #52787 ) ;
#14390 = DIRECTION ( 'NONE',  ( 0.09824042138329590335, -4.470611911092166224E-17, 0.9951627101165079203 ) ) ;
#14391 = CARTESIAN_POINT ( 'NONE',  ( -9.361133326760958440, -19.03884994183470880, -1.500000000000002220 ) ) ;
#14392 = CARTESIAN_POINT ( 'NONE',  ( 2.589743589743596086, -6.376774720514415407, 20.00140224358974095 ) ) ;
#14393 = CARTESIAN_POINT ( 'NONE',  ( -80.08103705783366877, -25.27791962444818097, 7.514832344495668615 ) ) ;
#14394 = EDGE_CURVE ( 'NONE', #80787, #41257, #35566, .T. ) ;
#14395 = FACE_BOUND ( 'NONE', #89140, .T. ) ;
#14396 = CARTESIAN_POINT ( 'NONE',  ( 33.00535138976593430, 3.570691370340898452, -12.97242311383974744 ) ) ;
#14397 = CARTESIAN_POINT ( 'NONE',  ( -18.23339674026497903, -6.527145932826366348, -1.500000000000002220 ) ) ;
#14398 = CARTESIAN_POINT ( 'NONE',  ( -45.57256808031284123, -23.48783264082476308, -1.443836473390102793 ) ) ;
#14399 = EDGE_LOOP ( 'NONE', ( #50333, #23095, #25819, #50785 ) ) ;
#14400 = CARTESIAN_POINT ( 'NONE',  ( -11.04204518803028456, 15.98388583709530941, 11.49999999999999645 ) ) ;
#14401 = DIRECTION ( 'NONE',  ( -0.000000000000000000, -1.000000000000000000, -0.000000000000000000 ) ) ;
#14402 = VECTOR ( 'NONE', #16767, 1000.000000000000114 ) ;
#14403 = B_SPLINE_CURVE_WITH_KNOTS ( 'NONE', 3,
 ( #25913, #57391, #12677, #65506, #96926, #95925, #66507, #96427 ),
 .UNSPECIFIED., .F., .F.,
 ( 4, 2, 2, 4 ),
 ( 0.0001293435094372204610, 0.002876179024813956854, 0.004249596782502322069, 0.005623014540190688151 ),
 .UNSPECIFIED. ) ;
#14404 = ORIENTED_EDGE ( 'NONE', *, *, #77598, .T. ) ;
#14405 = CARTESIAN_POINT ( 'NONE',  ( 3.121233215686890272, -5.876774720514404748, 18.93204046835445808 ) ) ;
#14406 = CARTESIAN_POINT ( 'NONE',  ( 3.769940963823357638, -6.376774720514402972, 18.16074422543206879 ) ) ;
#14407 = CARTESIAN_POINT ( 'NONE',  ( -70.58592565993524204, -25.30487017711728370, 4.870295994224087544 ) ) ;
#14408 = AXIS2_PLACEMENT_3D ( 'NONE', #67811, #75388, #67302 ) ;
#14410 = ADVANCED_FACE ( 'NONE', ( #59909 ), #14707, .F. ) ;
#14409 = CARTESIAN_POINT ( 'NONE',  ( -0.02075734969026423599, 5.866774720514426278, 22.60902280011862686 ) ) ;
#14411 = CARTESIAN_POINT ( 'NONE',  ( -19.57149217635686966, 1.386223266712492297, -1.500000000000002220 ) ) ;
#14412 = CARTESIAN_POINT ( 'NONE',  ( -66.58953762381672448, -23.48786465467241058, 11.44779295918254647 ) ) ;
#14413 = ORIENTED_EDGE ( 'NONE', *, *, #429, .F. ) ;
#14414 = CARTESIAN_POINT ( 'NONE',  ( -17.67581969798968444, -12.36387604476075097, 11.49999999999998934 ) ) ;
#14415 = AXIS2_PLACEMENT_3D ( 'NONE', #86961, #33176, #65163 ) ;
#14417 = B_SPLINE_CURVE_WITH_KNOTS ( 'NONE', 3,
 ( #16826, #47789, #597, #32552 ),
 .UNSPECIFIED., .F., .F.,
 ( 4, 4 ),
 ( 0.000000000000000000, 0.0001000000000000028644 ),
 .UNSPECIFIED. ) ;
#14416 = CARTESIAN_POINT ( 'NONE',  ( -40.57795575760204088, -24.83618233451450052, 1.606449574219539267 ) ) ;
#14418 = EDGE_CURVE ( 'NONE', #4416, #58649, #20312, .T. ) ;
#14419 = CARTESIAN_POINT ( 'NONE',  ( -99.84936175820153892, -25.18439370342922601, 3.453118441789628346 ) ) ;
#14420 = CARTESIAN_POINT ( 'NONE',  ( 19.24196208499951055, 12.69117723712289703, -1.500000000000002220 ) ) ;
#14421 = APPROVAL_DATE_TIME ( #7814, #68642 ) ;
#14422 = CARTESIAN_POINT ( 'NONE',  ( 22.81105451610979173, -2.682774720540237468, -18.46691820600746681 ) ) ;
#14423 = DIRECTION ( 'NONE',  ( 2.313651251573820309E-16, 1.000000000000000000, 8.068660792749117443E-16 ) ) ;
#14424 = CARTESIAN_POINT ( 'NONE',  ( 19.31759285448427477, -5.727529672960866236, 11.49999999999999645 ) ) ;
#14425 = CARTESIAN_POINT ( 'NONE',  ( -71.52287095715006160, -23.47593901973090169, -1.443836447538996870 ) ) ;
#14426 = DIRECTION ( 'NONE',  ( 0.000000000000000000, -0.9999999999976377785, -2.173523156925979975E-06 ) ) ;
#14427 = AXIS2_PLACEMENT_3D ( 'NONE', #65167, #88980, #2247 ) ;
#14428 = CARTESIAN_POINT ( 'NONE',  ( -94.52287095715006160, -23.48786465467242479, 11.44779295918254292 ) ) ;
#14429 = CARTESIAN_POINT ( 'NONE',  ( 8.160000000000000142, -6.754662360505033547, 8.925641719537455998 ) ) ;
#14430 = CARTESIAN_POINT ( 'NONE',  ( -122.5228709571501327, -23.96177878511310055, 10.65340807706329507 ) ) ;
#14431 = CARTESIAN_POINT ( 'NONE',  ( -1.345660788846553935, -19.86331345790170033, -1.500000000000002220 ) ) ;
#14432 = DIRECTION ( 'NONE',  ( 0.000000000000000000, 2.173523156925980399E-06, -0.9999999999976378895 ) ) ;
#14433 = CARTESIAN_POINT ( 'NONE',  ( -10.52764212615999639, 16.74383705166681580, -1.500000000000002220 ) ) ;
#14434 = CARTESIAN_POINT ( 'NONE',  ( -114.6228709571500559, -29.50247984919015209, -1.443849546365048253 ) ) ;
#14435 = B_SPLINE_CURVE_WITH_KNOTS ( 'NONE', 3,
 ( #66014, #96934, #11198, #65515 ),
 .UNSPECIFIED., .F., .F.,
 ( 4, 4 ),
 ( 0.000000000000000000, 0.0001000000000000167422 ),
 .UNSPECIFIED. ) ;
#14436 = DESIGN_CONTEXT ( 'detailed design', #59603, 'design' ) ;
#14437 = CARTESIAN_POINT ( 'NONE',  ( -123.5895376238167245, -23.47596703998600631, 11.44779298504227683 ) ) ;
#14438 = CARTESIAN_POINT ( 'NONE',  ( -66.52287095715007581, -23.47593901973090524, -1.443836447538997092 ) ) ;
#14439 = CARTESIAN_POINT ( 'NONE',  ( 8.970943996638910178, -18.66293075132952950, 11.49999999999999645 ) ) ;
#14440 = CARTESIAN_POINT ( 'NONE',  ( -58.52287095715006870, -23.94994826722565406, -0.6494450866342742490 ) ) ;
#14441 = CARTESIAN_POINT ( 'NONE',  ( -49.52475239181693212, -25.25138750780670449, 5.557101021734769830 ) ) ;
#14442 = AXIS2_PLACEMENT_3D ( 'NONE', #76436, #84062, #59241 ) ;
#14443 = CARTESIAN_POINT ( 'NONE',  ( 10.71911242904675987, 20.06137936439360203, 11.49999999999999645 ) ) ;
#14444 = EDGE_LOOP ( 'NONE', ( #22312, #27575, #76560, #74144 ) ) ;
#14445 = CARTESIAN_POINT ( 'NONE',  ( -60.62287095715004881, -24.63287334234180292, 0.9662140553045425184 ) ) ;
#14446 = CARTESIAN_POINT ( 'NONE',  ( -52.52287095715006870, -23.47596703998600631, 11.44779298504229104 ) ) ;
#14447 = CARTESIAN_POINT ( 'NONE',  ( 16.36621611169882229, 11.82581248522330064, 11.49999999999998934 ) ) ;
#14448 = CARTESIAN_POINT ( 'NONE',  ( 8.160000000000000142, 0.000000000000000000, 0.000000000000000000 ) ) ;
#14449 = CARTESIAN_POINT ( 'NONE',  ( -95.62287095715007013, -24.62226745350436730, 0.9660975649728198444 ) ) ;
#14450 = ORIENTED_EDGE ( 'NONE', *, *, #2074, .T. ) ;
#14451 = B_SPLINE_CURVE_WITH_KNOTS ( 'NONE', 3,
 ( #50029, #97680, #56644, #33789 ),
 .UNSPECIFIED., .F., .F.,
 ( 4, 4 ),
 ( 0.000000000000000000, 0.0001000000000000167422 ),
 .UNSPECIFIED. ) ;
#14452 = EDGE_LOOP ( 'NONE', ( #63582, #66439, #98198, #7338 ) ) ;
#14453 = DIRECTION ( 'NONE',  ( 0.000000000000000000, 0.000000000000000000, -1.000000000000000000 ) ) ;
#14454 = CARTESIAN_POINT ( 'NONE',  ( -12.24191887126339751, 19.33842681661653984, 11.49999999999998934 ) ) ;
#14455 = CARTESIAN_POINT ( 'NONE',  ( -41.68231076359069220, -25.22297927556520492, 3.502281763462448350 ) ) ;
#14456 = CARTESIAN_POINT ( 'NONE',  ( 3.837509532605410278, -21.31939230324424628, -1.500000000000002220 ) ) ;
#14457 = CARTESIAN_POINT ( 'NONE',  ( 32.60294298177596062, 6.376774720514426953, -11.48871326860665043 ) ) ;
#14458 = DIRECTION ( 'NONE',  ( 1.000000000000000000, 0.000000000000000000, 0.000000000000000000 ) ) ;
#14459 = CARTESIAN_POINT ( 'NONE',  ( -12.66259425867894350, -16.64798919286708667, 11.49999999999999645 ) ) ;
#14460 = ORIENTED_EDGE ( 'NONE', *, *, #77131, .F. ) ;
#14461 = FACE_OUTER_BOUND ( 'NONE', #62843, .T. ) ;
#14462 = CARTESIAN_POINT ( 'NONE',  ( -9.458160343781703006, 19.84743614482962926, 11.49999999999998934 ) ) ;
#14463 = CARTESIAN_POINT ( 'NONE',  ( -105.5573383875179303, -23.85049219812686871, 10.88485053497526955 ) ) ;
#14464 = CARTESIAN_POINT ( 'NONE',  ( -28.74184145762639631, -25.21724881489072345, 7.085837703947976074 ) ) ;
#14465 = VERTEX_POINT ( 'NONE', #45179 ) ;
#14466 = CARTESIAN_POINT ( 'NONE',  ( 4.856316114246853388, -6.376774720514408301, 19.03119074624055074 ) ) ;
#14467 = CARTESIAN_POINT ( 'NONE',  ( -90.59124612480250960, -24.40133493613050675, 9.663955038902805939 ) ) ;
#14468 = VERTEX_POINT ( 'NONE', #21313 ) ;
#14469 = CARTESIAN_POINT ( 'NONE',  ( -72.49563018961239891, -24.66019654487199730, 8.947790411086121054 ) ) ;
#14470 = EDGE_CURVE ( 'NONE', #22648, #54228, #74610, .T. ) ;
#14471 = VERTEX_POINT ( 'NONE', #37554 ) ;
#14472 = CIRCLE ( 'NONE', #12804, 3.570000000000003837 ) ;
#14473 = B_SPLINE_CURVE_WITH_KNOTS ( 'NONE', 3,
 ( #9906, #55096, #72825, #78407, #48488, #94643, #2311, #33242, #24619, #88044, #56607, #18518, #9403, #40364, #40857, #64734, #49491, #24126, #63213 ),
 .UNSPECIFIED., .F., .F.,
 ( 4, 1, 1, 1, 1, 1, 1, 1, 1, 1, 1, 1, 1, 1, 1, 1, 4 ),
 ( 0.000000000000000000, 0.06815824415599770758, 0.1347066022023564180, 0.2018649976035981897, 0.2707882662774624971, 0.3400242943604918633, 0.4080827390537212218, 0.4768131952581446398, 0.5473460643070942044, 0.5856397954238958814, 0.6288649531777639190, 0.6771532033637904791, 0.7308028113651051649, 0.7898066155325015325, 0.8543250087420142247, 0.9243651340575425035, 1.000000000000000000 ),
 .UNSPECIFIED. ) ;
#14474 = EDGE_CURVE ( 'NONE', #84745, #73391, #22623, .T. ) ;
#14475 = B_SPLINE_CURVE_WITH_KNOTS ( 'NONE', 3,
 ( #18376, #42733, #27989, #66583 ),
 .UNSPECIFIED., .F., .F.,
 ( 4, 4 ),
 ( 0.000000000000000000, 0.0004038461538461851630 ),
 .UNSPECIFIED. ) ;
#14476 = VERTEX_POINT ( 'NONE', #99439 ) ;
#14477 = CARTESIAN_POINT ( 'NONE',  ( -59.58953762381672448, -23.47593901973091235, -1.443836447539007972 ) ) ;
#14478 = CARTESIAN_POINT ( 'NONE',  ( -9.278253834636469577, -6.376774720514426953, 18.51871304725684553 ) ) ;
#14479 = CARTESIAN_POINT ( 'NONE',  ( -57.61196719931660937, -23.48783264082477018, -1.443836473390095243 ) ) ;
#14480 = CARTESIAN_POINT ( 'NONE',  ( -8.751980504941329286, -18.49744413911281882, -1.500000000000002220 ) ) ;
#14481 = EDGE_CURVE ( 'NONE', #46348, #10120, #44406, .T. ) ;
#14482 = ORIENTED_EDGE ( 'NONE', *, *, #50639, .T. ) ;
#14483 = CARTESIAN_POINT ( 'NONE',  ( -93.55620429048337883, -24.64965694238574656, 8.947790433994196491 ) ) ;
#14484 = CIRCLE ( 'NONE', #43681, 252.4458649670781085 ) ;
#14485 = DIRECTION ( 'NONE',  ( 0.000000000000000000, 0.000000000000000000, -1.000000000000000000 ) ) ;
#14486 = EDGE_CURVE ( 'NONE', #34072, #9990, #80700, .T. ) ;
#14487 = CARTESIAN_POINT ( 'NONE',  ( -4.213970605900704491, -6.376774720514415407, 20.02963804100705758 ) ) ;
#14488 = DIRECTION ( 'NONE',  ( 0.000000000000000000, 0.000000000000000000, -1.000000000000000000 ) ) ;
#14489 = VERTEX_POINT ( 'NONE', #32442 ) ;
#14490 = PLANE ( 'NONE',  #61442 ) ;
#14491 = VECTOR ( 'NONE', #39668, 1000.000000000000000 ) ;
#14492 = CARTESIAN_POINT ( 'NONE',  ( -64.55620429048339304, -23.48786465467241058, 11.44779295918254824 ) ) ;
#14493 = AXIS2_PLACEMENT_3D ( 'NONE', #74010, #20203, #51170 ) ;
#14494 = CARTESIAN_POINT ( 'NONE',  ( 20.75994597877129877, -1.272245555857973054, 11.49999999999998934 ) ) ;
#14495 = VERTEX_POINT ( 'NONE', #85728 ) ;
#14497 = ORIENTED_EDGE ( 'NONE', *, *, #10028, .T. ) ;
#14496 = CARTESIAN_POINT ( 'NONE',  ( -101.5228709571500758, -29.50250786944525672, 11.44777988621623166 ) ) ;
#14498 = AXIS2_PLACEMENT_3D ( 'NONE', #16377, #70675, #16883 ) ;
#14500 = ADVANCED_FACE ( 'NONE', ( #70508 ), #94334, .T. ) ;
#14499 = CARTESIAN_POINT ( 'NONE',  ( -50.40445135320379677, -25.12217862631780108, 7.101635560799164359 ) ) ;
#14501 = ORIENTED_EDGE ( 'NONE', *, *, #85401, .T. ) ;
#14502 = ORIENTED_EDGE ( 'NONE', *, *, #46224, .T. ) ;
#14503 = CARTESIAN_POINT ( 'NONE',  ( -107.5228709571500758, -29.50250243563736774, 8.947779886222136270 ) ) ;
#14504 = DIRECTION ( 'NONE',  ( -0.000000000000000000, 1.000000000000000000, -0.000000000000000000 ) ) ;
#14505 = CARTESIAN_POINT ( 'NONE',  ( -119.4728709570018879, -25.30556169000782418, 4.803960565675224892 ) ) ;
#14506 = CARTESIAN_POINT ( 'NONE',  ( -100.5925999562403490, -25.03152448450452638, 7.559861489817380154 ) ) ;
#14507 = CARTESIAN_POINT ( 'NONE',  ( -92.50480874862623182, -24.66019654487200441, 8.947790411086117501 ) ) ;
#14508 = CARTESIAN_POINT ( 'NONE',  ( -73.58953762381673869, -24.66019654487199020, 8.947790411086135265 ) ) ;
#14510 = ORIENTED_EDGE ( 'NONE', *, *, #89344, .F. ) ;
#14509 = CARTESIAN_POINT ( 'NONE',  ( 12.08182546098005972, -18.57710416600862402, 11.49999999999999645 ) ) ;
#14511 = LINE ( 'NONE', #61707, #56990 ) ;
#14512 = CARTESIAN_POINT ( 'NONE',  ( -11.22117850230010738, 19.66027149220947123, 11.49999999999998934 ) ) ;
#14514 = ORIENTED_EDGE ( 'NONE', *, *, #25631, .F. ) ;
#14513 = CARTESIAN_POINT ( 'NONE',  ( -115.6323228635793896, -23.48786465467241769, 11.44779295918253581 ) ) ;
#14515 = VERTEX_POINT ( 'NONE', #77600 ) ;
#14516 = CARTESIAN_POINT ( 'NONE',  ( -99.55620429048339304, -24.65952944569304961, 1.056160979905704345 ) ) ;
#14517 = B_SPLINE_CURVE_WITH_KNOTS ( 'NONE', 3,
 ( #20859, #66582, #21351, #51832, #97494, #52327 ),
 .UNSPECIFIED., .F., .F.,
 ( 4, 2, 4 ),
 ( 0.000000000000000000, 0.001380901958385383774, 0.002761803916770767548 ),
 .UNSPECIFIED. ) ;
#14518 = B_SPLINE_CURVE_WITH_KNOTS ( 'NONE', 3,
 ( #77300, #16916, #76794, #94037, #71213, #62107 ),
 .UNSPECIFIED., .F., .F.,
 ( 4, 2, 4 ),
 ( 0.000000000000000000, 0.001380901958385387894, 0.002761803916770775788 ),
 .UNSPECIFIED. ) ;
#14519 = CARTESIAN_POINT ( 'NONE',  ( -20.09103079077430820, 1.113595961413322177, 11.49999999999998934 ) ) ;
#14520 = B_SPLINE_SURFACE_WITH_KNOTS ( 'NONE', 3, 1, ( 
 ( #24685, #70886 ),
 ( #10977, #55668 ),
 ( #57173, #48045 ),
 ( #32309, #25190 ),
 ( #16573, #93700 ),
 ( #56167, #17586 ),
 ( #48558, #88109 ),
 ( #62786, #49552 ),
 ( #33812, #79485 ),
 ( #78975, #95713 ),
 ( #63283, #55168 ),
 ( #40926, #24191 ),
 ( #79981, #41942 ),
 ( #72884, #47548 ),
 ( #94200, #39923 ),
 ( #17081, #9472 ),
 ( #2372, #40432 ),
 ( #33303, #95214 ),
 ( #56670, #18087 ) ),
 .UNSPECIFIED., .F., .F., .F.,
 ( 4, 1, 1, 1, 1, 1, 1, 1, 1, 1, 1, 1, 1, 1, 1, 1, 4 ),
 ( 2, 2 ),
 ( 0.000000000000000000, 0.06535138202659385165, 0.1279160318306120925, 0.1883602055716991353, 0.2472160772654510563, 0.3056301291974100054, 0.3637698398318218729, 0.4226609139127802117, 0.4826872940903894071, 0.5433002212395561248, 0.6041179553231045274, 0.6649648912652841304, 0.7274134941125618425, 0.7914676251494242587, 0.8580554427290951747, 0.9270368146149470245, 1.000000000000000000 ),
 ( 0.000000000000000000, 1.000000000000000000 ),
 .UNSPECIFIED. ) ;
#14521 = CARTESIAN_POINT ( 'NONE',  ( 3.421177667410919110, 0.3587747205144265483, 28.69411518427638441 ) ) ;
#14522 = ORIENTED_EDGE ( 'NONE', *, *, #4079, .F. ) ;
#14523 = CARTESIAN_POINT ( 'NONE',  ( -126.5228709571501753, -23.96127896941633750, -0.6493128931037959184 ) ) ;
#14524 = CARTESIAN_POINT ( 'NONE',  ( 17.53502452033532677, 13.85421504792973479, -1.500000000000002220 ) ) ;
#14525 = VERTEX_POINT ( 'NONE', #62403 ) ;
#14526 = ORIENTED_EDGE ( 'NONE', *, *, #84910, .F. ) ;
#14527 = CARTESIAN_POINT ( 'NONE',  ( -34.62287095715005592, -23.47593901973091235, -1.443836447539013301 ) ) ;
#14528 = DIRECTION ( 'NONE',  ( 0.9975640502598241977, -0.06975647374412546897, -0.000000000000000000 ) ) ;
#14529 = DIRECTION ( 'NONE',  ( -3.773278334453080206E-23, 0.9999999999976377785, 2.173523156925979975E-06 ) ) ;
#14530 = EDGE_CURVE ( 'NONE', #26199, #22449, #26045, .T. ) ;
#14531 = CARTESIAN_POINT ( 'NONE',  ( -47.62287095715004881, -24.64898659630367916, 1.056161002820821038 ) ) ;
#14532 = PLANE ( 'NONE',  #25338 ) ;
#14533 = CARTESIAN_POINT ( 'NONE',  ( -4.042178566331402045, 19.10766070095605684, -1.500000000000002220 ) ) ;
#14534 = CARTESIAN_POINT ( 'NONE',  ( -43.52287095715006160, -29.50250786944525672, 11.44777988621624232 ) ) ;
#14535 = CARTESIAN_POINT ( 'NONE',  ( 7.480126432006339421, -20.11416664461015458, 11.49999999999998934 ) ) ;
#14536 = CARTESIAN_POINT ( 'NONE',  ( -2.373828433815573735, -5.876774720514408301, 19.48240003225459915 ) ) ;
#14537 = DIRECTION ( 'NONE',  ( -3.773278334453079618E-23, 0.9999999999976377785, 2.173523156925978705E-06 ) ) ;
#14538 = DIRECTION ( 'NONE',  ( -3.773278334453080206E-23, 0.9999999999976377785, 2.173523156925979975E-06 ) ) ;
#14540 = EDGE_CURVE ( 'NONE', #55726, #11050, #61905, .T. ) ;
#14539 = CIRCLE ( 'NONE', #8027, 1.699999999999999289 ) ;
#14541 = CARTESIAN_POINT ( 'NONE',  ( -2.380104427745746154, 22.76713797270899065, -1.500000000000002220 ) ) ;
#14542 = EDGE_CURVE ( 'NONE', #98254, #96767, #15212, .T. ) ;
#14543 = PERSON_AND_ORGANIZATION ( #70597, #27821 ) ;
#14544 = CARTESIAN_POINT ( 'NONE',  ( -0.02075734969026423599, 5.965225279485572685, -0.08597719988137648983 ) ) ;
#14545 = LINE ( 'NONE', #21647, #60409 ) ;
#14546 = CARTESIAN_POINT ( 'NONE',  ( -14.92271332039470444, 13.28099397388983327, 11.49999999999999645 ) ) ;
#14547 = CYLINDRICAL_SURFACE ( 'NONE', #84131, 18.35000000000000142 ) ;
#14548 = CIRCLE ( 'NONE', #71273, 2.040000000000000036 ) ;
#14549 = CARTESIAN_POINT ( 'NONE',  ( -123.6228709571500559, -23.47593901973091235, -1.443836447538997536 ) ) ;
#14550 = CARTESIAN_POINT ( 'NONE',  ( 0.8635838190919263857, -3.990505948720460605, -8.999999999999998224 ) ) ;
#14551 = B_SPLINE_CURVE_WITH_KNOTS ( 'NONE', 3,
 ( #19288, #66004, #44138, #43639, #21278, #74577 ),
 .UNSPECIFIED., .F., .F.,
 ( 4, 2, 4 ),
 ( 6.384118678619858489E-06, 0.001386860460828383441, 0.002767336802978146663 ),
 .UNSPECIFIED. ) ;
#14552 = ORIENTED_EDGE ( 'NONE', *, *, #82424, .F. ) ;
#14553 = FACE_OUTER_BOUND ( 'NONE', #65727, .T. ) ;
#14554 = CARTESIAN_POINT ( 'NONE',  ( -70.55620429048339304, -23.48786465467240703, 11.44779295918254647 ) ) ;
#14555 = CARTESIAN_POINT ( 'NONE',  ( -8.443908442993951269, 20.02826104456839218, 11.49999999999998934 ) ) ;
#14556 = DIRECTION ( 'NONE',  ( 0.000000000000000000, 0.000000000000000000, -1.000000000000000000 ) ) ;
#14558 = CIRCLE ( 'NONE', #50212, 28.96799999999999642 ) ;
#14557 = B_SPLINE_CURVE_WITH_KNOTS ( 'NONE', 3,
 ( #87598, #40919, #96697, #27199, #95704, #58154 ),
 .UNSPECIFIED., .F., .F.,
 ( 4, 2, 4 ),
 ( 6.384118678609746610E-06, 0.001386860460828372816, 0.002767336802978135821 ),
 .UNSPECIFIED. ) ;
#14559 = CARTESIAN_POINT ( 'NONE',  ( -15.96901387740391343, -11.39031854172415947, -1.500000000000002220 ) ) ;
#14560 = CARTESIAN_POINT ( 'NONE',  ( -55.52287095715005449, -29.50249982740957577, 7.747779886224967605 ) ) ;
#14561 = VECTOR ( 'NONE', #11859, 1000.000000000000000 ) ;
#14562 = SECURITY_CLASSIFICATION_LEVEL ( 'unclassified' ) ;
#14563 = VECTOR ( 'NONE', #6207, 1000.000000000000000 ) ;
#14564 = DIRECTION ( 'NONE',  ( -0.000000000000000000, 1.000000000000000000, -0.000000000000000000 ) ) ;
#14565 = CARTESIAN_POINT ( 'NONE',  ( 3.251543564379332008, -6.376774720514424288, 21.68810402963413964 ) ) ;
#14566 = CARTESIAN_POINT ( 'NONE',  ( -19.23287947355762384, -7.152392467615741545, 11.49999999999999645 ) ) ;
#14567 = CARTESIAN_POINT ( 'NONE',  ( 30.60113388085891017, 4.386958714992013952, 26.76092701747204927 ) ) ;
#14568 = CARTESIAN_POINT ( 'NONE',  ( -53.62287095715005592, -23.47596703998600276, 11.44779298504227683 ) ) ;
#14569 = AXIS2_PLACEMENT_3D ( 'NONE', #24510, #16903, #55989 ) ;
#14570 = VERTEX_POINT ( 'NONE', #99929 ) ;
#14571 =( NAMED_UNIT ( * ) SI_UNIT ( $, .STERADIAN. ) SOLID_ANGLE_UNIT ( ) );
#14572 = CARTESIAN_POINT ( 'NONE',  ( -51.55620429048340014, -23.47593901973091235, -1.443836447539009749 ) ) ;
#14573 = DIRECTION ( 'NONE',  ( -0.000000000000000000, 1.000000000000000000, -0.000000000000000000 ) ) ;
#14574 = CARTESIAN_POINT ( 'NONE',  ( -44.62287095715004881, -29.50247984919015209, -1.443849546365060466 ) ) ;
#14575 = DIRECTION ( 'NONE',  ( 0.000000000000000000, 0.000000000000000000, 1.000000000000000000 ) ) ;
#14576 = CARTESIAN_POINT ( 'NONE',  ( -124.6228709571500701, -24.66019654487200086, 8.947790411086121054 ) ) ;
#14577 = ADVANCED_FACE ( 'NONE', ( #15712 ), #63415, .T. ) ;
#14578 = CARTESIAN_POINT ( 'NONE',  ( 1.702247502073919394, 23.03039350466679025, 11.49999999999999645 ) ) ;
#14579 = CARTESIAN_POINT ( 'NONE',  ( -2.657479817400386413, -22.66247145590962120, 11.49999999999998934 ) ) ;
#14580 = DIRECTION ( 'NONE',  ( -3.773278334453079618E-23, 0.9999999999976377785, 2.173523156925979975E-06 ) ) ;
#14581 = CARTESIAN_POINT ( 'NONE',  ( -105.6228709571500417, -24.99132157543166954, 2.256160258750667502 ) ) ;
#14582 = CARTESIAN_POINT ( 'NONE',  ( -123.5228709571501042, -23.96127896941632685, -0.6493128931037979168 ) ) ;
#14583 = DIRECTION ( 'NONE',  ( -1.000000000000000000, -3.773278334444167608E-23, -8.201307833595939069E-29 ) ) ;
#14584 = CARTESIAN_POINT ( 'NONE',  ( -110.6256086358791748, -24.73486907724917572, 1.287355809206965240 ) ) ;
#14585 = CARTESIAN_POINT ( 'NONE',  ( 16.40513048700843513, 14.50174154637248591, -1.500000000000002220 ) ) ;
#14586 = CARTESIAN_POINT ( 'NONE',  ( -54.52287095715005449, -23.48783264082476308, -1.443836473390096797 ) ) ;
#14587 = CARTESIAN_POINT ( 'NONE',  ( -50.62287095715004170, -23.48783264082478084, -1.443836473390070596 ) ) ;
#14588 = DIRECTION ( 'NONE',  ( -0.000000000000000000, 2.173523156925979552E-06, -0.9999999999976378895 ) ) ;
#14589 = DIRECTION ( 'NONE',  ( -1.000000000000000000, -0.000000000000000000, -0.000000000000000000 ) ) ;
#14590 = PLANE ( 'NONE',  #17702 ) ;
#14591 = LINE ( 'NONE', #5987, #33992 ) ;
#14592 = ORIENTED_EDGE ( 'NONE', *, *, #79352, .F. ) ;
#14593 = B_SPLINE_CURVE_WITH_KNOTS ( 'NONE', 3,
 ( #73291, #42361, #10380, #96127, #19486, #9879 ),
 .UNSPECIFIED., .F., .F.,
 ( 4, 2, 4 ),
 ( -8.871155308958663375E-06, 0.0009003829173646808823, 0.001809636990038320306 ),
 .UNSPECIFIED. ) ;
#14594 = EDGE_CURVE ( 'NONE', #35733, #63436, #92830, .T. ) ;
#14595 = CARTESIAN_POINT ( 'NONE',  ( 10.07161678670223637, 17.78519941539584792, 11.49999999999998934 ) ) ;
#14596 = ORIENTED_EDGE ( 'NONE', *, *, #43436, .F. ) ;
#14597 = ORIENTED_EDGE ( 'NONE', *, *, #8933, .T. ) ;
#14598 = ORIENTED_EDGE ( 'NONE', *, *, #47851, .F. ) ;
#14599 = EDGE_LOOP ( 'NONE', ( #92966, #3016, #23895, #61299 ) ) ;
#14600 = CARTESIAN_POINT ( 'NONE',  ( -20.21456430084473155, -11.12997698910670152, -1.500000000000002220 ) ) ;
#14601 = CARTESIAN_POINT ( 'NONE',  ( -61.55970283376174734, -23.73766607897670156, -1.055555164236459342 ) ) ;
#14602 = CARTESIAN_POINT ( 'NONE',  ( 19.68333694646799614, 4.735253856516091098, -1.500000000000002220 ) ) ;
#14603 = ADVANCED_FACE ( 'NONE', ( #30937 ), #27248, .T. ) ;
#14604 = ORIENTED_EDGE ( 'NONE', *, *, #3918, .T. ) ;
#14605 = CARTESIAN_POINT ( 'NONE',  ( -122.5228709571501042, -23.72747288104470442, -1.053458166803224794 ) ) ;
#14606 = LINE ( 'NONE', #36951, #78959 ) ;
#14607 = EDGE_CURVE ( 'NONE', #1549, #89739, #40061, .T. ) ;
#14608 = CARTESIAN_POINT ( 'NONE',  ( -28.52287095715005805, -24.48903441264110015, 8.947790432046794251 ) ) ;
#14609 = CARTESIAN_POINT ( 'NONE',  ( -70.59202623176527425, -24.40034930558990922, 0.3402023900116040167 ) ) ;
#14611 = ORIENTED_EDGE ( 'NONE', *, *, #71060, .F. ) ;
#14610 = CARTESIAN_POINT ( 'NONE',  ( 10.45947017991876926, -18.73710855793504848, 11.49999999999999645 ) ) ;
#14612 = PLANE ( 'NONE',  #58190 ) ;
#14613 = CARTESIAN_POINT ( 'NONE',  ( 15.52291915823239599, 3.595107466738254764, -28.22347026866548347 ) ) ;
#14614 = ADVANCED_FACE ( 'NONE', ( #10103 ), #57791, .T. ) ;
#14615 = ORIENTED_EDGE ( 'NONE', *, *, #64753, .F. ) ;
#14616 = ADVANCED_FACE ( 'NONE', ( #56304, #42570 ), #87735, .F. ) ;
#14617 = B_SPLINE_CURVE_WITH_KNOTS ( 'NONE', 3,
 ( #95942, #86824, #79712, #65526 ),
 .UNSPECIFIED., .F., .F.,
 ( 4, 4 ),
 ( 5.880066517545130343E-09, 0.0003976749849169158076 ),
 .UNSPECIFIED. ) ;
#14618 = CARTESIAN_POINT ( 'NONE',  ( -19.40401905104624802, 7.283777608679691262, 11.49999999999998934 ) ) ;
#14619 = AXIS2_PLACEMENT_3D ( 'NONE', #66307, #98213, #67800 ) ;
#14621 = ORIENTED_EDGE ( 'NONE', *, *, #44564, .T. ) ;
#14620 = CARTESIAN_POINT ( 'NONE',  ( 31.93426202889373400, 5.965225279485572685, 6.907000118922836940 ) ) ;
#14622 = CARTESIAN_POINT ( 'NONE',  ( -91.52287095715009002, -23.73934037231757443, 11.05740245334328442 ) ) ;
#14623 = ORIENTED_EDGE ( 'NONE', *, *, #26180, .T. ) ;
#14624 = CARTESIAN_POINT ( 'NONE',  ( 4.966983519792414370, -6.376774720514415407, 19.83633487160803099 ) ) ;
#14625 = ADVANCED_FACE ( 'NONE', ( #18219 ), #88238, .F. ) ;
#14626 = DIRECTION ( 'NONE',  ( 0.000000000000000000, 0.000000000000000000, -1.000000000000000000 ) ) ;
#14627 = CARTESIAN_POINT ( 'NONE',  ( -17.28599015371049674, 13.57978550619682956, 11.49999999999999645 ) ) ;
#14628 = LINE ( 'NONE', #85142, #49600 ) ;
#14629 = CARTESIAN_POINT ( 'NONE',  ( 9.831018646898828095, -20.30805102056165623, 11.49999999999998934 ) ) ;
#14630 = CARTESIAN_POINT ( 'NONE',  ( -8.674659061502078217, -19.08593140856894621, -1.500000000000002220 ) ) ;
#14631 = CARTESIAN_POINT ( 'NONE',  ( 16.00000000000000000, 0.000000000000000000, 0.000000000000000000 ) ) ;
#14632 = CARTESIAN_POINT ( 'NONE',  ( 1.600000000000000755, 0.000000000000000000, 24.00000000000000000 ) ) ;
#14633 = ORIENTED_EDGE ( 'NONE', *, *, #63259, .F. ) ;
#14634 = VECTOR ( 'NONE', #6042, 1000.000000000000227 ) ;
#14635 = ORIENTED_EDGE ( 'NONE', *, *, #97220, .T. ) ;
#14636 = VECTOR ( 'NONE', #67157, 1000.000000000000114 ) ;
#14637 = B_SPLINE_CURVE_WITH_KNOTS ( 'NONE', 3,
 ( #55014, #46391, #53021, #77322 ),
 .UNSPECIFIED., .F., .F.,
 ( 4, 4 ),
 ( 0.000000000000000000, 9.999999999998897304E-05 ),
 .UNSPECIFIED. ) ;
#14638 = ORIENTED_EDGE ( 'NONE', *, *, #53289, .T. ) ;
#14639 = CARTESIAN_POINT ( 'NONE',  ( -78.62287095715005592, -29.50248528299804818, 1.056150453629038477 ) ) ;
#14640 = VECTOR ( 'NONE', #45134, 1000.000000000000114 ) ;
#14641 = CARTESIAN_POINT ( 'NONE',  ( -14.25192491085926072, -16.12266454619898326, -1.500000000000002220 ) ) ;
#14642 = CARTESIAN_POINT ( 'NONE',  ( -90.62287095715004170, -23.47596703998600631, 11.44779298504227860 ) ) ;
#14643 = ORIENTED_EDGE ( 'NONE', *, *, #7604, .T. ) ;
#14644 = CARTESIAN_POINT ( 'NONE',  ( -21.11812214938331422, 0.5215410354952813021, 11.49999999999998934 ) ) ;
#14645 = CARTESIAN_POINT ( 'NONE',  ( -31.52287095715006160, -29.50250243563736774, 8.947779886222150481 ) ) ;
#14646 = DIRECTION ( 'NONE',  ( -3.773278334453079030E-23, 0.9999999999976377785, 2.173523156925979128E-06 ) ) ;
#14647 = CARTESIAN_POINT ( 'NONE',  ( 11.69063526134919684, -3.622774720514426949, -29.65990201929480108 ) ) ;
#14648 = PLANE ( 'NONE',  #21582 ) ;
#14649 = CARTESIAN_POINT ( 'NONE',  ( -1.122631020312409245, -5.876774720514411854, 19.41635569784906679 ) ) ;
#14650 = CARTESIAN_POINT ( 'NONE',  ( 9.120982285578694615, 20.23247719416018242, -1.500000000000002220 ) ) ;
#14651 = CARTESIAN_POINT ( 'NONE',  ( -81.55862828805493336, -23.73791477778911840, 11.05961554403170943 ) ) ;
#14652 = EDGE_CURVE ( 'NONE', #70610, #71832, #28561, .T. ) ;
#14653 = ORIENTED_EDGE ( 'NONE', *, *, #79561, .F. ) ;
#14654 = CARTESIAN_POINT ( 'NONE',  ( -51.66594184980125704, -25.24860094318730219, 5.409172948272988002 ) ) ;
#14655 = DIRECTION ( 'NONE',  ( -3.773278334453079618E-23, 0.9999999999976377785, 2.173523156925979975E-06 ) ) ;
#14656 = CARTESIAN_POINT ( 'NONE',  ( -8.160000000000000142, 0.000000000000000000, 0.000000000000000000 ) ) ;
#14657 = ADVANCED_FACE ( 'NONE', ( #27330 ), #34941, .T. ) ;
#14659 = B_SPLINE_CURVE_WITH_KNOTS ( 'NONE', 3,
 ( #60735, #50252, #11669, #50750 ),
 .UNSPECIFIED., .F., .F.,
 ( 4, 4 ),
 ( 0.000000000000000000, 9.999999999998897304E-05 ),
 .UNSPECIFIED. ) ;
#14658 = CARTESIAN_POINT ( 'NONE',  ( -119.6228709571500559, -24.64898659630368627, 1.056161002820833028 ) ) ;
#14660 = CARTESIAN_POINT ( 'NONE',  ( -8.858824863812619910, -17.32749669425128047, -1.500000000000002220 ) ) ;
#14661 = CARTESIAN_POINT ( 'NONE',  ( -18.60337119584764665, 10.53494341765418874, 11.49999999999998934 ) ) ;
#14662 = FACE_OUTER_BOUND ( 'NONE', #47596, .T. ) ;
#14663 = DIRECTION ( 'NONE',  ( -0.000000000000000000, 0.000000000000000000, -1.000000000000000000 ) ) ;
#14664 = CARTESIAN_POINT ( 'NONE',  ( -122.5562042904833930, -24.64965694238575367, 8.947790433994191162 ) ) ;
#14665 = CARTESIAN_POINT ( 'NONE',  ( 22.02124265030973760, -6.143225279485574397, 16.20402280011862217 ) ) ;
#14666 = CARTESIAN_POINT ( 'NONE',  ( -0.4833002549469566644, -22.66139224067150337, -1.500000000000002220 ) ) ;
#14667 = ORIENTED_EDGE ( 'NONE', *, *, #75188, .T. ) ;
#14668 = EDGE_CURVE ( 'NONE', #56734, #22424, #65424, .T. ) ;
#14669 = CARTESIAN_POINT ( 'NONE',  ( -110.5228709571500616, -25.00182538069145366, 7.747789668545101094 ) ) ;
#14670 = CARTESIAN_POINT ( 'NONE',  ( -62.62287095715003460, -24.51387760970724372, 9.387446482453428942 ) ) ;
#14671 = CARTESIAN_POINT ( 'NONE',  ( -18.24533751216517885, 7.751685665592884078, 11.49999999999999645 ) ) ;
#14672 = PLANE ( 'NONE',  #57081 ) ;
#14673 = ORIENTED_EDGE ( 'NONE', *, *, #74314, .T. ) ;
#14674 = EDGE_CURVE ( 'NONE', #49194, #66916, #87878, .T. ) ;
#14675 = CARTESIAN_POINT ( 'NONE',  ( -5.903826827417286260, -5.876774720514418071, 20.39230070883895252 ) ) ;
#14676 = CARTESIAN_POINT ( 'NONE',  ( -57.52287095715003318, -23.48783264082476663, -1.443836473390093911 ) ) ;
#14677 = CARTESIAN_POINT ( 'NONE',  ( 19.51036611237648088, 9.378288983258578071, 11.49999999999998934 ) ) ;
#14678 = CARTESIAN_POINT ( 'NONE',  ( -49.14425558977711006, -25.10935316468142986, 3.703948968546024290 ) ) ;
#14679 = CARTESIAN_POINT ( 'NONE',  ( -16.21482014894483470, 10.69450053600103345, -1.500000000000002220 ) ) ;
#14680 = PLANE ( 'NONE',  #85397 ) ;
#14681 = CARTESIAN_POINT ( 'NONE',  ( -82.62287095715005592, -24.51387760970725793, 9.387446482453437824 ) ) ;
#14682 = CARTESIAN_POINT ( 'NONE',  ( -14.51517298184297289, -13.48802281452852725, -1.500000000000002220 ) ) ;
#14683 = ORIENTED_EDGE ( 'NONE', *, *, #97272, .F. ) ;
#14684 = CARTESIAN_POINT ( 'NONE',  ( -20.07547297788957152, 3.163885811906596679, 11.49999999999999645 ) ) ;
#14685 = CARTESIAN_POINT ( 'NONE',  ( -106.6228709571500559, -24.64898659630368627, 1.056161002820831474 ) ) ;
#14686 = AXIS2_PLACEMENT_3D ( 'NONE', #90633, #60700, #21110 ) ;
#14687 = APPROVAL ( #38259, 'UNSPECIFIED' ) ;
#14688 = CARTESIAN_POINT ( 'NONE',  ( 33.63447098073278596, -3.363532777116247541, -11.63841935007238426 ) ) ;
#14689 = EDGE_LOOP ( 'NONE', ( #52649, #99041, #30132, #25753 ) ) ;
#14690 = CARTESIAN_POINT ( 'NONE',  ( -30.63234162661936111, -23.86952536761623023, -1.017619990082605508 ) ) ;
#14691 = CARTESIAN_POINT ( 'NONE',  ( 30.93860345374796239, -5.965225279485572685, 26.43402280011862615 ) ) ;
#14692 = CARTESIAN_POINT ( 'NONE',  ( -49.74369414166532977, -25.31601817158193057, 4.940877927940857894 ) ) ;
#14693 = CARTESIAN_POINT ( 'NONE',  ( -40.58501377093656970, -24.63419186844611630, 9.035850630976923981 ) ) ;
#14694 = CARTESIAN_POINT ( 'NONE',  ( -32.99388727629348494, -25.11010231571544082, 2.831122766524410750 ) ) ;
#14695 = CARTESIAN_POINT ( 'NONE',  ( -19.91332876899582160, 2.521106391696132931, -1.500000000000002220 ) ) ;
#14696 = FACE_OUTER_BOUND ( 'NONE', #99076, .T. ) ;
#14697 = VERTEX_POINT ( 'NONE', #80113 ) ;
#14698 = CARTESIAN_POINT ( 'NONE',  ( 22.02124265030973760, -6.143225279485574397, 16.20402280011862217 ) ) ;
#14699 = VECTOR ( 'NONE', #22383, 1000.000000000000114 ) ;
#14700 = CARTESIAN_POINT ( 'NONE',  ( 19.54225192528841859, -11.95493969655435151, 11.49999999999999645 ) ) ;
#14701 = CARTESIAN_POINT ( 'NONE',  ( 15.30562342774392093, -16.77826389816909725, 11.49999999999998934 ) ) ;
#14702 = CARTESIAN_POINT ( 'NONE',  ( -49.76261995625480949, -25.31297168719047619, 4.511523210314938304 ) ) ;
#14703 = CARTESIAN_POINT ( 'NONE',  ( -7.749999999999996447, 24.84999999999999787, 0.000000000000000000 ) ) ;
#14704 = CARTESIAN_POINT ( 'NONE',  ( -38.48002663928881617, -24.66019654487199375, 8.947790411086119278 ) ) ;
#14705 = AXIS2_PLACEMENT_3D ( 'NONE', #37082, #83252, #13733 ) ;
#14706 = CARTESIAN_POINT ( 'NONE',  ( -71.58953762381672448, -24.64898659630528854, 1.056161002820822370 ) ) ;
#14707 = CYLINDRICAL_SURFACE ( 'NONE', #67330, 91.74549126261076992 ) ;
#14708 = CARTESIAN_POINT ( 'NONE',  ( -34.52287095715006160, -24.65952944569303895, 1.056160979905690134 ) ) ;
#14709 = ORIENTED_EDGE ( 'NONE', *, *, #20096, .T. ) ;
#14710 = CARTESIAN_POINT ( 'NONE',  ( -14.79517943714664518, -13.99575967537150412, -1.500000000000002220 ) ) ;
#14711 = ORIENTED_EDGE ( 'NONE', *, *, #16471, .F. ) ;
#14712 = ADVANCED_FACE ( 'NONE', ( #41061 ), #18296, .T. ) ;
#14713 = CARTESIAN_POINT ( 'NONE',  ( 7.334040449947802465, -21.76207178258647090, -1.500000000000002220 ) ) ;
#14714 = CARTESIAN_POINT ( 'NONE',  ( -119.5228709571500758, -24.65952944569305316, 1.056160979905705899 ) ) ;
#14715 = ORIENTED_EDGE ( 'NONE', *, *, #77253, .F. ) ;
#14716 = CARTESIAN_POINT ( 'NONE',  ( -38.62287095715005592, -24.33832256526968507, 0.1851278514119830965 ) ) ;
#14717 = CARTESIAN_POINT ( 'NONE',  ( -116.5228709571500332, -24.66019654487200086, 8.947790411086113949 ) ) ;
#14718 = CARTESIAN_POINT ( 'NONE',  ( -51.48599270264783456, -24.66019654487199730, 8.947790411086117501 ) ) ;
#14720 = ORIENTED_EDGE ( 'NONE', *, *, #48598, .F. ) ;
#14719 = CARTESIAN_POINT ( 'NONE',  ( 20.49604761983493972, 5.601127818285958071, 11.49999999999999645 ) ) ;
#14721 = EDGE_CURVE ( 'NONE', #69556, #37181, #28323, .T. ) ;
#14722 = VERTEX_POINT ( 'NONE', #37439 ) ;
#14723 = CARTESIAN_POINT ( 'NONE',  ( 21.93305185196877360, -3.456643806985262302, 11.49999999999998934 ) ) ;
#14724 = ADVANCED_FACE ( 'NONE', ( #13584 ), #81617, .T. ) ;
#14725 = CARTESIAN_POINT ( 'NONE',  ( -7.709890279958820258, -19.11728055126480186, 11.49999999999998934 ) ) ;
#14726 = EDGE_LOOP ( 'NONE', ( #15138, #22998, #81646, #48844 ) ) ;
#14727 = ORIENTED_EDGE ( 'NONE', *, *, #34101, .T. ) ;
#14728 = CARTESIAN_POINT ( 'NONE',  ( -109.7388188129343831, -25.27682897105086823, 5.649347691802135252 ) ) ;
#14729 = CARTESIAN_POINT ( 'NONE',  ( -36.58953762381673158, -24.64898659630367916, 1.056161002820378725 ) ) ;
#14730 = ORIENTED_EDGE ( 'NONE', *, *, #88150, .F. ) ;
#14731 = CARTESIAN_POINT ( 'NONE',  ( -91.58852912192975282, -24.34968618360934656, 0.1864209137778843617 ) ) ;
#14732 = ORIENTED_EDGE ( 'NONE', *, *, #76913, .T. ) ;
#14733 = CARTESIAN_POINT ( 'NONE',  ( 30.56736729430419430, 3.651218969664528302, 25.10220481361090705 ) ) ;
#14734 = CARTESIAN_POINT ( 'NONE',  ( -88.58953762381669605, -24.66019654487199375, 8.947790411086117501 ) ) ;
#14735 = CARTESIAN_POINT ( 'NONE',  ( -20.33245250387252767, 4.503473919074798104, -1.500000000000002220 ) ) ;
#14736 = EDGE_CURVE ( 'NONE', #22224, #93401, #98319, .T. ) ;
#14737 = CARTESIAN_POINT ( 'NONE',  ( -12.70408864715453667, 17.69581422525067183, 11.49999999999999645 ) ) ;
#14738 = CARTESIAN_POINT ( 'NONE',  ( -100.4326965455115044, -25.18492896333868103, 3.293943116708551777 ) ) ;
#14739 = CARTESIAN_POINT ( 'NONE',  ( -78.64730139296283085, -23.48786465467241058, 11.44779295918254469 ) ) ;
#14740 = CARTESIAN_POINT ( 'NONE',  ( -15.54266751046811557, -16.22994250641250957, -1.500000000000002220 ) ) ;
#14741 = B_SPLINE_CURVE_WITH_KNOTS ( 'NONE', 3,
 ( #67366, #20173, #12566, #14050 ),
 .UNSPECIFIED., .F., .F.,
 ( 4, 4 ),
 ( 2.186341471430182952E-11, 0.0004637143556766918197 ),
 .UNSPECIFIED. ) ;
#14742 = CARTESIAN_POINT ( 'NONE',  ( -50.64790834543075704, -25.26334744936552212, 4.705120468826944347 ) ) ;
#14743 = ORIENTED_EDGE ( 'NONE', *, *, #33752, .T. ) ;
#14744 = CARTESIAN_POINT ( 'NONE',  ( -65.05438548721848235, -5.356774720514425603, 27.45402280011862572 ) ) ;
#14745 = CARTESIAN_POINT ( 'NONE',  ( -38.52287095715006870, -23.47596703998600631, 11.44779298504229281 ) ) ;
#14746 = ORIENTED_EDGE ( 'NONE', *, *, #42120, .F. ) ;
#14747 = ORIENTED_EDGE ( 'NONE', *, *, #60450, .F. ) ;
#14748 = VECTOR ( 'NONE', #72218, 1000.000000000000000 ) ;
#14749 = CARTESIAN_POINT ( 'NONE',  ( -46.55318986248427393, -23.96169478059712432, 10.65365249895718414 ) ) ;
#14750 = VERTEX_POINT ( 'NONE', #66417 ) ;
#14751 = CARTESIAN_POINT ( 'NONE',  ( -0.3244385709253747585, -21.36021439428519386, -1.500000000000002220 ) ) ;
#14752 = ORIENTED_EDGE ( 'NONE', *, *, #59234, .T. ) ;
#14753 = CARTESIAN_POINT ( 'NONE',  ( -18.19455084753484542, -10.52586660885228298, -1.500000000000002220 ) ) ;
#14754 = DIRECTION ( 'NONE',  ( 0.000000000000000000, 0.9999999999976377785, 2.173523156925979128E-06 ) ) ;
#14755 = FACE_OUTER_BOUND ( 'NONE', #58885, .T. ) ;
#14756 = CARTESIAN_POINT ( 'NONE',  ( -1.351711525931510449, 21.94731587555429186, -1.500000000000002220 ) ) ;
#14757 = CARTESIAN_POINT ( 'NONE',  ( -87.64316148452599009, -23.48783264082478084, -1.443836473390063713 ) ) ;
#14758 = VERTEX_POINT ( 'NONE', #50670 ) ;
#14759 = DIRECTION ( 'NONE',  ( -0.7071067811865442421, 0.000000000000000000, -0.7071067811865507924 ) ) ;
#14760 = EDGE_CURVE ( 'NONE', #86370, #18719, #45481, .T. ) ;
#14761 = EDGE_CURVE ( 'NONE', #74060, #61556, #35447, .T. ) ;
#14762 = FACE_OUTER_BOUND ( 'NONE', #52222, .T. ) ;
#14763 = CIRCLE ( 'NONE', #30998, 1.699999999999994849 ) ;
#14764 = CARTESIAN_POINT ( 'NONE',  ( -127.2228709571500360, -23.47596703998600631, 11.44779298504227860 ) ) ;
#14765 =( GEOMETRIC_REPRESENTATION_CONTEXT ( 3 ) GLOBAL_UNCERTAINTY_ASSIGNED_CONTEXT ( ( #73365 ) ) GLOBAL_UNIT_ASSIGNED_CONTEXT ( ( #89951, #63274, #66650 ) ) REPRESENTATION_CONTEXT ( 'NONE', 'WORKASPACE' ) );
#14766 = CARTESIAN_POINT ( 'NONE',  ( -20.42270456864569184, -23.87886260247287495, 8.909134979017293787 ) ) ;
#14767 = CARTESIAN_POINT ( 'NONE',  ( -4.730540317195566224, 20.75322969461001676, 11.49999999999998934 ) ) ;
#14768 = DIRECTION ( 'NONE',  ( -3.773278334444167608E-23, 1.000000000000000000, 0.000000000000000000 ) ) ;
#14769 = CARTESIAN_POINT ( 'NONE',  ( -100.4381051993576506, -29.50248914370730091, 2.832395270851967073 ) ) ;
#14770 = EDGE_CURVE ( 'NONE', #12582, #63531, #86722, .T. ) ;
#14771 = LINE ( 'NONE', #53857, #50296 ) ;
#14772 = CARTESIAN_POINT ( 'NONE',  ( -85.62287095715009855, -24.62285846362214059, 9.038163152653529764 ) ) ;
#14773 = CARTESIAN_POINT ( 'NONE',  ( 15.74396088501716839, 16.14010210793005839, -1.500000000000002220 ) ) ;
#14774 = EDGE_CURVE ( 'NONE', #41750, #77030, #43558, .T. ) ;
#14775 = B_SPLINE_CURVE_WITH_KNOTS ( 'NONE', 3,
 ( #54435, #45821, #85369, #53942 ),
 .UNSPECIFIED., .F., .F.,
 ( 4, 4 ),
 ( 0.007591229774494646920, 0.009012827652035957510 ),
 .UNSPECIFIED. ) ;
#14776 = CARTESIAN_POINT ( 'NONE',  ( -101.3738023147422780, -25.27307239909452008, 3.986250617436227550 ) ) ;
#14777 = EDGE_LOOP ( 'NONE', ( #79395, #20224, #27756, #37916 ) ) ;
#14778 = DIRECTION ( 'NONE',  ( -0.000000000000000000, 1.000000000000000000, -0.000000000000000000 ) ) ;
#14779 = CARTESIAN_POINT ( 'NONE',  ( -10.75157073690095721, 16.42123490324765811, 11.49999999999999645 ) ) ;
#14780 = PLANE ( 'NONE',  #42267 ) ;
#14781 = DIRECTION ( 'NONE',  ( 0.000000000000000000, 1.000000000000000000, 0.000000000000000000 ) ) ;
#14782 = ORIENTED_EDGE ( 'NONE', *, *, #90005, .F. ) ;
#14783 = B_SPLINE_CURVE_WITH_KNOTS ( 'NONE', 3,
 ( #38880, #78935, #69842, #46501 ),
 .UNSPECIFIED., .F., .F.,
 ( 4, 4 ),
 ( 0.7693278071035449805, 0.7703285541443105622 ),
 .UNSPECIFIED. ) ;
#14784 = CARTESIAN_POINT ( 'NONE',  ( -88.63863195549789964, -23.73791477778912196, 11.05961554403170588 ) ) ;
#14785 = CARTESIAN_POINT ( 'NONE',  ( -125.5800465235194849, -25.31863276151772979, 6.461862851402581320 ) ) ;
#14786 = CARTESIAN_POINT ( 'NONE',  ( -124.5891619642989525, -24.51419770103158768, 9.386484678747164523 ) ) ;
#14787 = CARTESIAN_POINT ( 'NONE',  ( 7.987771016649366729, -18.01272016045900415, -1.500000000000002220 ) ) ;
#14788 = ORIENTED_EDGE ( 'NONE', *, *, #25488, .T. ) ;
#14789 = CARTESIAN_POINT ( 'NONE',  ( 10.68713020350585197, 3.316774720514176877, -28.05292731652309257 ) ) ;
#14790 = DIRECTION ( 'NONE',  ( 1.000000000000000000, -2.209838822900391329E-16, 0.000000000000000000 ) ) ;
#14791 = EDGE_CURVE ( 'NONE', #90885, #13954, #49076, .T. ) ;
#14792 = EDGE_CURVE ( 'NONE', #24496, #94960, #66906, .T. ) ;
#14793 = PERSON_AND_ORGANIZATION ( #70597, #27821 ) ;
#14794 = ORIENTED_EDGE ( 'NONE', *, *, #71716, .T. ) ;
#14795 = CARTESIAN_POINT ( 'NONE',  ( 12.92500000000000249, 14.50000000000000000, 11.24599928863594300 ) ) ;
#14796 = DIRECTION ( 'NONE',  ( -3.773278334453079618E-23, 0.9999999999976377785, 2.173523156925979975E-06 ) ) ;
#14797 = CARTESIAN_POINT ( 'NONE',  ( -55.53718012664960924, -24.63355581998386157, 0.9682620441943822209 ) ) ;
#14798 = CARTESIAN_POINT ( 'NONE',  ( -100.0332803147414324, -25.03145169341005527, 7.519340699400126837 ) ) ;
#14799 = CARTESIAN_POINT ( 'NONE',  ( 5.864177746775673050, -6.376774720514426065, 21.69926562011473337 ) ) ;
#14800 = CARTESIAN_POINT ( 'NONE',  ( 10.54059822343757880, -5.876774720514426953, 22.82308057603841078 ) ) ;
#14801 = CARTESIAN_POINT ( 'NONE',  ( -43.55620429048338593, -23.48786465467240347, 11.44779295918255180 ) ) ;
#14802 = CARTESIAN_POINT ( 'NONE',  ( -19.26508835251014773, 5.270845654819066084, -1.500000000000002220 ) ) ;
#14803 = CARTESIAN_POINT ( 'NONE',  ( 27.53860345374808105, 5.356774720496559894, 19.84760796525321780 ) ) ;
#14804 = CARTESIAN_POINT ( 'NONE',  ( -45.50996254517149708, -23.85049219812685095, 10.88485053497527133 ) ) ;
#14805 = ORIENTED_EDGE ( 'NONE', *, *, #61577, .F. ) ;
#14806 = ADVANCED_FACE ( 'NONE', ( #59276 ), #35937, .F. ) ;
#14807 = EDGE_CURVE ( 'NONE', #24461, #96004, #39346, .T. ) ;
#14808 = CARTESIAN_POINT ( 'NONE',  ( -66.52287095715009002, -24.34917612406836795, 0.1852690917426535466 ) ) ;
#14809 = CARTESIAN_POINT ( 'NONE',  ( -80.59639368748227639, -24.15602025860896163, 10.28564288303536145 ) ) ;
#14810 = CARTESIAN_POINT ( 'NONE',  ( -120.6228709571500559, -24.15431212366390668, -0.2830839119428921191 ) ) ;
#14811 = CARTESIAN_POINT ( 'NONE',  ( -39.48568060755304288, -24.51314013834315730, 0.6176544820404118452 ) ) ;
#14812 = B_SPLINE_CURVE_WITH_KNOTS ( 'NONE', 3,
 ( #25972, #25468, #56444, #17864, #78737, #94481 ),
 .UNSPECIFIED., .F., .F.,
 ( 4, 2, 4 ),
 ( 0.000000000000000000, 0.001380901958385384858, 0.002761803916770769717 ),
 .UNSPECIFIED. ) ;
#14813 = AXIS2_PLACEMENT_3D ( 'NONE', #67247, #91557, #98166 ) ;
#14814 = CARTESIAN_POINT ( 'NONE',  ( -27.75512989467660674, -25.26026286428627188, 1.629582517731039459 ) ) ;
#14815 = CARTESIAN_POINT ( 'NONE',  ( -1.363607173041644582, -5.876774720514419847, 20.50445910983877340 ) ) ;
#14816 = DIRECTION ( 'NONE',  ( -3.773278334453079030E-23, 0.9999999999976377785, 2.173523156925979128E-06 ) ) ;
#14817 = CARTESIAN_POINT ( 'NONE',  ( -89.62287095715004170, -24.66019654487199020, 8.947790411086128159 ) ) ;
#14818 = EDGE_LOOP ( 'NONE', ( #32329, #80215, #81795, #94245 ) ) ;
#14819 =( REPRESENTATION_RELATIONSHIP ('NONE','NONE', #96270, #26923 ) REPRESENTATION_RELATIONSHIP_WITH_TRANSFORMATION ( #37908 )SHAPE_REPRESENTATION_RELATIONSHIP( ) );
#14820 = CARTESIAN_POINT ( 'NONE',  ( -5.286950244708777724, -19.55949958832428948, -1.500000000000002220 ) ) ;
#14821 = ADVANCED_FACE ( 'NONE', ( #67902 ), #98823, .T. ) ;
#14822 = CARTESIAN_POINT ( 'NONE',  ( -76.62287095715004170, -24.51387760970723662, 9.387446482453412955 ) ) ;
#14823 = CARTESIAN_POINT ( 'NONE',  ( -109.6228709571500559, -29.50248528299804818, 1.056150453629043584 ) ) ;
#14824 = CARTESIAN_POINT ( 'NONE',  ( -83.55620429048339304, -23.48783264082478439, -1.443836473390066377 ) ) ;
#14825 = EDGE_LOOP ( 'NONE', ( #15732, #18634, #54679, #60296 ) ) ;
#14826 = CARTESIAN_POINT ( 'NONE',  ( 32.16024265030974050, -5.965225279485572685, 14.03360796525321774 ) ) ;
#14827 = AXIS2_PLACEMENT_3D ( 'NONE', #50885, #29024, #82318 ) ;
#14828 = CARTESIAN_POINT ( 'NONE',  ( 0.3675393366473880818, 20.13074986235200470, -1.500000000000002220 ) ) ;
#14829 = CARTESIAN_POINT ( 'NONE',  ( -19.97109070424261645, 6.737033823242594366, 11.49999999999999645 ) ) ;
#14830 = LOCAL_TIME ( 0, 54, 15.00000000000000000, #77431 ) ;
#14831 = LINE ( 'NONE', #83854, #2869 ) ;
#14832 = CARTESIAN_POINT ( 'NONE',  ( 6.025212951983072607, -21.27585971943098642, -1.500000000000002220 ) ) ;
#14833 = EDGE_CURVE ( 'NONE', #52438, #28254, #21690, .T. ) ;
#14834 = CARTESIAN_POINT ( 'NONE',  ( -10.66544979547405347, 17.54311462378693420, -1.500000000000002220 ) ) ;
#14835 = CARTESIAN_POINT ( 'NONE',  ( -96.52287095715007581, -23.72747288104470798, -1.053458166803225904 ) ) ;
#14836 = CARTESIAN_POINT ( 'NONE',  ( -60.61726270389971205, -23.48783264082476308, -1.443836473390097686 ) ) ;
#14837 = ORIENTED_EDGE ( 'NONE', *, *, #46233, .F. ) ;
#14838 = LINE ( 'NONE', #75737, #10193 ) ;
#14839 = ORIENTED_EDGE ( 'NONE', *, *, #9450, .F. ) ;
#14840 = EDGE_CURVE ( 'NONE', #1763, #38912, #14083, .T. ) ;
#14841 = CARTESIAN_POINT ( 'NONE',  ( -5.923037968371668072, -6.376774720514413630, 19.62288733224861303 ) ) ;
#14842 = CARTESIAN_POINT ( 'NONE',  ( -64.52287095715006160, -24.64965694238407323, 8.947790433994201820 ) ) ;
#14843 = VERTEX_POINT ( 'NONE', #30822 ) ;
#14844 = VERTEX_POINT ( 'NONE', #37932 ) ;
#14845 = VERTEX_POINT ( 'NONE', #31316 ) ;
#14846 = DIRECTION ( 'NONE',  ( 3.773278334444166432E-23, -1.000000000000000000, 0.000000000000000000 ) ) ;
#14847 = LINE ( 'NONE', #53436, #84286 ) ;
#14848 = CARTESIAN_POINT ( 'NONE',  ( -68.54058893247888307, -24.51419770103157347, 9.386484678747180510 ) ) ;
#14849 = CARTESIAN_POINT ( 'NONE',  ( -18.09956831669839872, 9.893135806712603397, -1.500000000000002220 ) ) ;
#14850 = EDGE_CURVE ( 'NONE', #63555, #24333, #9158, .T. ) ;
#14851 = CARTESIAN_POINT ( 'NONE',  ( -21.62496174240652991, 0.2022338437372764308, 11.49999999999999645 ) ) ;
#14852 = VERTEX_POINT ( 'NONE', #91705 ) ;
#14853 = CARTESIAN_POINT ( 'NONE',  ( -81.52287095715001897, -24.66019654487199375, 8.947790411086126383 ) ) ;
#14854 = CARTESIAN_POINT ( 'NONE',  ( -57.62287095715006302, -23.95044443724992433, 10.65354141964650125 ) ) ;
#14855 = CARTESIAN_POINT ( 'NONE',  ( -21.16225983376422448, 7.283793490815352989, -1.500000000000002220 ) ) ;
#14856 = EDGE_CURVE ( 'NONE', #45943, #68317, #76978, .T. ) ;
#14857 = CARTESIAN_POINT ( 'NONE',  ( -62.52287095715006160, -24.65952944569304606, 1.056160979905695463 ) ) ;
#14858 = DIRECTION ( 'NONE',  ( 1.000000000000000000, 3.773278334444167608E-23, 8.201307833595939069E-29 ) ) ;
#14859 = ORIENTED_EDGE ( 'NONE', *, *, #38995, .F. ) ;
#14860 = DIRECTION ( 'NONE',  ( -4.335561085774420994E-16, -0.000000000000000000, 1.000000000000000000 ) ) ;
#14861 = CARTESIAN_POINT ( 'NONE',  ( -49.60653733798429244, -23.73791477778911840, 11.05961554403170943 ) ) ;
#14862 = FACE_OUTER_BOUND ( 'NONE', #19971, .T. ) ;
#14863 = CARTESIAN_POINT ( 'NONE',  ( -20.92377055399060737, -0.003182555231893603818, 11.49999999999998934 ) ) ;
#14864 = ORIENTED_EDGE ( 'NONE', *, *, #50802, .T. ) ;
#14866 = ORIENTED_EDGE ( 'NONE', *, *, #98392, .T. ) ;
#14865 = CARTESIAN_POINT ( 'NONE',  ( -67.65234729852470252, -23.48786465467241058, 11.44779295918254824 ) ) ;
#14867 = ORIENTED_EDGE ( 'NONE', *, *, #53452, .T. ) ;
#14868 = AXIS2_PLACEMENT_3D ( 'NONE', #88537, #79913, #1302 ) ;
#14869 = PLANE ( 'NONE',  #50338 ) ;
#14870 = CARTESIAN_POINT ( 'NONE',  ( 13.39648796734645231, 16.42122281929413319, -1.500000000000002220 ) ) ;
#14871 = ORIENTED_EDGE ( 'NONE', *, *, #61127, .T. ) ;
#14872 = DIRECTION ( 'NONE',  ( -0.000000000000000000, 1.000000000000000000, -0.000000000000000000 ) ) ;
#14873 = CARTESIAN_POINT ( 'NONE',  ( -100.4005007646339891, -25.12215675090913081, 7.100843682671821533 ) ) ;
#14874 = CARTESIAN_POINT ( 'NONE',  ( 4.771108217193557266, 21.26182814020628697, -1.500000000000002220 ) ) ;
#14875 = CARTESIAN_POINT ( 'NONE',  ( -56.62287095715005592, -24.64965695001468404, 8.947790433994185832 ) ) ;
#14876 = FACE_OUTER_BOUND ( 'NONE', #16854, .T. ) ;
#14877 = B_SPLINE_CURVE_WITH_KNOTS ( 'NONE', 3,
 ( #39418, #93693, #854, #31808, #24677, #4228 ),
 .UNSPECIFIED., .F., .F.,
 ( 4, 2, 4 ),
 ( 0.000000000000000000, 0.001380764517854760195, 0.002761529035709520390 ),
 .UNSPECIFIED. ) ;
#14878 = LINE ( 'NONE', #38218, #85443 ) ;
#14879 = CARTESIAN_POINT ( 'NONE',  ( -5.042499505632127565, 21.24692939306837758, -1.500000000000002220 ) ) ;
#14880 = CARTESIAN_POINT ( 'NONE',  ( -78.94548380723361447, -25.26800482900744527, 6.082637674949305406 ) ) ;
#14881 = VERTEX_POINT ( 'NONE', #45559 ) ;
#14882 = PLANE ( 'NONE',  #63179 ) ;
#14883 = DIRECTION ( 'NONE',  ( 1.000000000000000000, 0.000000000000000000, 0.000000000000000000 ) ) ;
#14884 = CARTESIAN_POINT ( 'NONE',  ( -43.62287095715004881, -24.50216790748099527, 0.6166512839513605959 ) ) ;
#14885 = ORIENTED_EDGE ( 'NONE', *, *, #3697, .F. ) ;
#14886 = ORIENTED_EDGE ( 'NONE', *, *, #59191, .F. ) ;
#14887 = ADVANCED_FACE ( 'NONE', ( #15585 ), #96084, .T. ) ;
#14888 = ORIENTED_EDGE ( 'NONE', *, *, #27562, .T. ) ;
#14889 = CARTESIAN_POINT ( 'NONE',  ( -44.62287095715004881, -23.47593901973091235, -1.443836447539011525 ) ) ;
#14890 = CARTESIAN_POINT ( 'NONE',  ( 15.74494995282791088, 14.18698661492608615, -1.500000000000002220 ) ) ;
#14891 = CARTESIAN_POINT ( 'NONE',  ( -94.62287095715009855, -23.96127896941632685, -0.6493128931037828178 ) ) ;
#14892 = CARTESIAN_POINT ( 'NONE',  ( -95.62287095714997065, -24.82576562982392332, 8.398263435472967942 ) ) ;
#14893 = FACE_OUTER_BOUND ( 'NONE', #33612, .T. ) ;
#14895 = CARTESIAN_POINT ( 'NONE',  ( 32.85081302853786411, 5.152774720514582185, -13.10817780685225031 ) ) ;
#14894 = B_SPLINE_CURVE_WITH_KNOTS ( 'NONE', 3,
 ( #55083, #8895, #1789, #32728 ),
 .UNSPECIFIED., .F., .F.,
 ( 4, 4 ),
 ( 0.007591229774494646920, 0.009012827652035957510 ),
 .UNSPECIFIED. ) ;
#14896 = DIRECTION ( 'NONE',  ( 0.000000000000000000, -0.9999999999976377785, -2.173523156925979975E-06 ) ) ;
#14897 = CARTESIAN_POINT ( 'NONE',  ( -51.49344744762370851, -25.31373635202942296, 5.229250005650915689 ) ) ;
#14898 = VERTEX_POINT ( 'NONE', #46550 ) ;
#14899 = CARTESIAN_POINT ( 'NONE',  ( 17.65527434030279252, -8.155491144718855168, 11.49999999999999645 ) ) ;
#14900 = PLANE ( 'NONE',  #30928 ) ;
#14901 = ORIENTED_EDGE ( 'NONE', *, *, #52752, .T. ) ;
#14902 = CARTESIAN_POINT ( 'NONE',  ( -113.6228709571500559, -24.64965695001469115, 8.947790433994176951 ) ) ;
#14903 = DIRECTION ( 'NONE',  ( 0.000000000000000000, 2.173523156925980399E-06, -0.9999999999976378895 ) ) ;
#14904 = FACE_OUTER_BOUND ( 'NONE', #91911, .T. ) ;
#14905 = VECTOR ( 'NONE', #77948, 1000.000000000000000 ) ;
#14906 = CARTESIAN_POINT ( 'NONE',  ( -34.62287095715005592, -23.48786465467240347, 11.44779295918255535 ) ) ;
#14907 = CARTESIAN_POINT ( 'NONE',  ( -19.13235715846047214, 4.354950445902704637, 11.49999999999998934 ) ) ;
#14908 = DIRECTION ( 'NONE',  ( -3.773278334453079030E-23, 0.9999999999976377785, 2.173523156925979128E-06 ) ) ;
#14910 = ORIENTED_EDGE ( 'NONE', *, *, #21399, .T. ) ;
#14909 = CC_DESIGN_APPROVAL ( #53771, ( #65234 ) ) ;
#14911 = CARTESIAN_POINT ( 'NONE',  ( 13.05104812959431548, -17.15854754814989391, 11.49999999999998934 ) ) ;
#14912 = CARTESIAN_POINT ( 'NONE',  ( 10.11704143035998271, 0.6681657214399121525, 19.30000000000000071 ) ) ;
#14913 = CARTESIAN_POINT ( 'NONE',  ( -73.62287095715005592, -23.47593901973091235, -1.443836447539006196 ) ) ;
#14914 = CARTESIAN_POINT ( 'NONE',  ( -65.58953762381672448, -25.00182538069145721, 7.747789668545095765 ) ) ;
#14915 = CARTESIAN_POINT ( 'NONE',  ( 21.10734164270438029, -9.282589649079691085, -1.500000000000002220 ) ) ;
#14916 = EDGE_CURVE ( 'NONE', #38339, #82766, #98639, .T. ) ;
#14917 = COORDINATED_UNIVERSAL_TIME_OFFSET ( 0, 0, .AHEAD. ) ;
#14918 = DIRECTION ( 'NONE',  ( 0.000000000000000000, 0.000000000000000000, -1.000000000000000000 ) ) ;
#14919 = CARTESIAN_POINT ( 'NONE',  ( -94.62287095715005592, -29.50247984919015209, -1.443849546365051806 ) ) ;
#14920 = CARTESIAN_POINT ( 'NONE',  ( 11.17094659993960803, -16.83544227557131023, 11.49999999999999645 ) ) ;
#14921 = CARTESIAN_POINT ( 'NONE',  ( -121.5915921659258743, -23.73791477778912196, 11.05961554403169878 ) ) ;
#14922 = CARTESIAN_POINT ( 'NONE',  ( -64.62287095715002749, -23.96177878511307568, 10.65340807706330217 ) ) ;
#14923 = CARTESIAN_POINT ( 'NONE',  ( -109.3584176993576591, -25.27948031066536672, 4.206202526585778756 ) ) ;
#14924 = DIRECTION ( 'NONE',  ( 3.773278334444166432E-23, -1.000000000000000000, 0.000000000000000000 ) ) ;
#14925 = CARTESIAN_POINT ( 'NONE',  ( -110.4389802415574309, -25.18425583253951672, 3.296667852188002623 ) ) ;
#14926 = CARTESIAN_POINT ( 'NONE',  ( 9.006517291608927778, -17.75031788249398446, -1.500000000000002220 ) ) ;
#14928 = ADVANCED_FACE ( 'NONE', ( #77479 ), #38930, .T. ) ;
#14927 = DIRECTION ( 'NONE',  ( -0.000000000000000000, -0.000000000000000000, -1.000000000000000000 ) ) ;
#14929 = CARTESIAN_POINT ( 'NONE',  ( -17.81549539028256746, -8.563599010019245839, -1.500000000000002220 ) ) ;
#14930 = EDGE_CURVE ( 'NONE', #14389, #12137, #62796, .T. ) ;
#14931 = CARTESIAN_POINT ( 'NONE',  ( -56.53763200549867207, -24.51314013834315730, 0.6176544820404098468 ) ) ;
#14932 = ADVANCED_FACE ( 'NONE', ( #24202 ), #78481, .F. ) ;
#14933 = EDGE_CURVE ( 'NONE', #6012, #76643, #58764, .T. ) ;
#14934 = DIRECTION ( 'NONE',  ( 3.773278334444167608E-23, -1.000000000000000000, 0.000000000000000000 ) ) ;
#14935 = B_SPLINE_CURVE_WITH_KNOTS ( 'NONE', 3,
 ( #85665, #11417, #42392, #17150, #78030, #8542 ),
 .UNSPECIFIED., .F., .F.,
 ( 4, 2, 4 ),
 ( 0.000000000000000000, 0.001380901958385387027, 0.002761803916770774053 ),
 .UNSPECIFIED. ) ;
#14936 = CARTESIAN_POINT ( 'NONE',  ( -42.52287095715007581, -24.33832256527049154, 0.1851278514138574860 ) ) ;
#14937 = CARTESIAN_POINT ( 'NONE',  ( -9.011640028862021978, 18.61544202926687674, 11.49999999999999645 ) ) ;
#14938 = CARTESIAN_POINT ( 'NONE',  ( 8.971512145086528278, -9.528487854913501920, 6.500000000000001776 ) ) ;
#14939 = CARTESIAN_POINT ( 'NONE',  ( -50.37830952628071657, -25.25138672683397800, 5.197789126111715063 ) ) ;
#14940 = CARTESIAN_POINT ( 'NONE',  ( 2.290073164716609710, 22.57640404599860418, 11.49999999999999645 ) ) ;
#14941 = CIRCLE ( 'NONE', #99178, 0.8160000000000008358 ) ;
#14942 = ORIENTED_EDGE ( 'NONE', *, *, #47111, .T. ) ;
#14943 = B_SPLINE_SURFACE_WITH_KNOTS ( 'NONE', 3, 1, ( 
 ( #96231, #97224 ),
 ( #58662, #64810 ),
 ( #2893, #33823 ),
 ( #89610, #19089 ),
 ( #34829, #26713 ),
 ( #57674, #95724 ),
 ( #50060, #11481 ),
 ( #73395, #3891 ),
 ( #65799, #96716 ),
 ( #27217, #75867 ),
 ( #75368, #6863 ),
 ( #28209, #21084 ),
 ( #52050, #37815 ),
 ( #68770, #36325 ),
 ( #14464, #21574 ),
 ( #61174, #13471 ),
 ( #60672, #99687 ),
 ( #20586, #45446 ),
 ( #14967, #30192 ),
 ( #91100, #28713 ),
 ( #83481, #38305 ),
 ( #67284, #76360 ),
 ( #29702, #6369 ) ),
 .UNSPECIFIED., .F., .F., .F.,
 ( 4, 1, 1, 1, 1, 1, 1, 1, 1, 1, 1, 1, 1, 1, 1, 1, 1, 1, 1, 1, 4 ),
 ( 2, 2 ),
 ( 0.000000000000000000, 0.07295106587586651370, 0.1415836941865448451, 0.2059264601708667708, 0.2653013571846051799, 0.3205972327139279821, 0.3718165030988102027, 0.4187897697094515315, 0.4616987286157640535, 0.5021335821035650682, 0.5408043152926476083, 0.5781805253279657109, 0.6142968652075138092, 0.6496782432647868477, 0.6842994600896368240, 0.7183589527723606150, 0.7520808646475963810, 0.8176524386023842350, 0.8797220764054374254, 0.9399655597309863886, 1.000000000000000000 ),
 ( 0.000000000000000000, 1.000000000000000000 ),
 .UNSPECIFIED. ) ;
#14944 = CARTESIAN_POINT ( 'NONE',  ( -67.52287095715006160, -24.33832256527049154, 0.1851278514138614828 ) ) ;
#14945 = CARTESIAN_POINT ( 'NONE',  ( -74.62287095715005592, -24.35013146730203815, 9.818937971375111928 ) ) ;
#14946 = CARTESIAN_POINT ( 'NONE',  ( 18.63370447891095694, 7.782165041754079304, 11.49999999999998934 ) ) ;
#14947 = EDGE_CURVE ( 'NONE', #20637, #42580, #24697, .T. ) ;
#14948 = LINE ( 'NONE', #93565, #33861 ) ;
#14949 = CARTESIAN_POINT ( 'NONE',  ( -95.62287095715008434, -24.91544648472619983, 1.928969306349227475 ) ) ;
#14950 = VERTEX_POINT ( 'NONE', #64807 ) ;
#14951 = ORIENTED_EDGE ( 'NONE', *, *, #42293, .T. ) ;
#14952 = EDGE_CURVE ( 'NONE', #70257, #17515, #91446, .T. ) ;
#14953 = CARTESIAN_POINT ( 'NONE',  ( 0.2885822020289898759, -5.876774720514415407, 19.94806476610988710 ) ) ;
#14954 = CARTESIAN_POINT ( 'NONE',  ( 19.54225192528841859, -11.95493969655435151, -1.500000000000002220 ) ) ;
#14955 = CARTESIAN_POINT ( 'NONE',  ( -40.89256867414531627, -25.13235034710942273, 2.898563804593949023 ) ) ;
#14956 = CARTESIAN_POINT ( 'NONE',  ( -14.23256820581467785, 16.29125061305494526, -1.500000000000002220 ) ) ;
#14957 = LINE ( 'NONE', #7850, #30146 ) ;
#14958 = CARTESIAN_POINT ( 'NONE',  ( -34.60129100296713744, -23.96119346886880663, -0.6495511937831990323 ) ) ;
#14959 = AXIS2_PLACEMENT_3D ( 'NONE', #37537, #44653, #75579 ) ;
#14960 = CARTESIAN_POINT ( 'NONE',  ( -20.67734376658059858, -3.193854526364364954, 11.49999999999999645 ) ) ;
#14961 = EDGE_LOOP ( 'NONE', ( #51251, #53558, #88541, #40082 ) ) ;
#14962 = CARTESIAN_POINT ( 'NONE',  ( -69.42561217104606897, -25.31612484405095387, 5.145891826979088535 ) ) ;
#14963 = AXIS2_PLACEMENT_3D ( 'NONE', #87720, #26318, #26814 ) ;
#14964 = CARTESIAN_POINT ( 'NONE',  ( -21.70078857174656761, -3.768841730229552045, 11.49999999999998934 ) ) ;
#14965 = ADVANCED_FACE ( 'NONE', ( #41951 ), #96229, .F. ) ;
#14966 = CARTESIAN_POINT ( 'NONE',  ( -105.6251633804084804, -24.83644354573579349, 8.397322867130096569 ) ) ;
#14967 = CARTESIAN_POINT ( 'NONE',  ( -28.29841854899664710, -25.21724961408747845, 7.453534148297638495 ) ) ;
#14968 = ORIENTED_EDGE ( 'NONE', *, *, #87977, .T. ) ;
#14969 = CARTESIAN_POINT ( 'NONE',  ( -28.98875734969026396, 5.965225279485572685, -0.08597719988137648983 ) ) ;
#14970 = CARTESIAN_POINT ( 'NONE',  ( 7.160000000000000142, 7.891155995661682354, 5.788828319098143993 ) ) ;
#14971 = VERTEX_POINT ( 'NONE', #18585 ) ;
#14972 = CARTESIAN_POINT ( 'NONE',  ( -72.55911193603030540, -23.73791477778911840, 11.05961554403170943 ) ) ;
#14973 = ORIENTED_EDGE ( 'NONE', *, *, #50259, .F. ) ;
#14974 = VERTEX_POINT ( 'NONE', #32824 ) ;
#14975 = CARTESIAN_POINT ( 'NONE',  ( -61.64687923781921342, -25.18035200424451858, 3.255061677420811428 ) ) ;
#14976 = CARTESIAN_POINT ( 'NONE',  ( -101.4571681947234083, -25.10935903412801906, 3.296845841340303451 ) ) ;
#14977 = CARTESIAN_POINT ( 'NONE',  ( -4.141025641025641413, -6.376774720514420736, 20.67377804487180271 ) ) ;
#14978 = CARTESIAN_POINT ( 'NONE',  ( -20.16212974941129588, 3.559051167911782887, -1.500000000000002220 ) ) ;
#14979 = EDGE_CURVE ( 'NONE', #57577, #71190, #18858, .T. ) ;
#14980 = B_SPLINE_CURVE_WITH_KNOTS ( 'NONE', 3,
 ( #16532, #63241, #61742, #47508, #70340, #94163 ),
 .UNSPECIFIED., .F., .F.,
 ( 4, 2, 4 ),
 ( 0.000000000000000000, 0.001380901958385383340, 0.002761803916770766681 ),
 .UNSPECIFIED. ) ;
#14981 = ORIENTED_EDGE ( 'NONE', *, *, #67253, .F. ) ;
#14982 = LINE ( 'NONE', #82502, #23405 ) ;
#14983 = CARTESIAN_POINT ( 'NONE',  ( 0.7734273019049007214, 3.892732205269316292, -2.677392948487098267E-15 ) ) ;
#14984 = DIRECTION ( 'NONE',  ( 0.7640209514960704107, 0.000000000000000000, -0.6451914333552789538 ) ) ;
#14985 = CARTESIAN_POINT ( 'NONE',  ( 6.212073114426278408, 21.40951068830820958, -1.500000000000002220 ) ) ;
#14986 = EDGE_CURVE ( 'NONE', #73864, #61563, #56682, .T. ) ;
#14988 = DIRECTION ( 'NONE',  ( 0.9822594791677485837, 0.000000000000000000, -0.1875268396392986980 ) ) ;
#14987 = VECTOR ( 'NONE', #12788, 1000.000000000000114 ) ;
#14989 = CARTESIAN_POINT ( 'NONE',  ( -88.62287095715004170, -23.48786465467241769, 11.44779295918254114 ) ) ;
#14990 = ORIENTED_EDGE ( 'NONE', *, *, #77131, .T. ) ;
#14991 = CARTESIAN_POINT ( 'NONE',  ( -29.80803119424227177, -25.23992228501141000, 4.571394149977143329 ) ) ;
#14992 = CARTESIAN_POINT ( 'NONE',  ( 7.749999999999998224, 25.69999999999999574, 2.100000000000000089 ) ) ;
#14993 = SECURITY_CLASSIFICATION ( '', '', #24419 ) ;
#14994 = CARTESIAN_POINT ( 'NONE',  ( -4.186882374726557110, 20.40937146592452223, 11.49999999999998934 ) ) ;
#14995 = ORIENTED_EDGE ( 'NONE', *, *, #47485, .T. ) ;
#14997 = EDGE_LOOP ( 'NONE', ( #63003, #6864, #15973, #91273 ) ) ;
#14996 = CARTESIAN_POINT ( 'NONE',  ( -42.52287095715004739, -24.35013146730202749, 9.818937971375117257 ) ) ;
#14998 = VECTOR ( 'NONE', #1834, 1000.000000000000227 ) ;
#14999 = CARTESIAN_POINT ( 'NONE',  ( -4.926336369345162502, 0.3587747205143967943, -28.61095484066305161 ) ) ;
#15000 = EDGE_LOOP ( 'NONE', ( #13362, #670, #22298, #35145 ) ) ;
#15001 = ORIENTED_EDGE ( 'NONE', *, *, #31783, .T. ) ;
#15002 = CARTESIAN_POINT ( 'NONE',  ( -80.52287095715006160, -29.50250786944525672, 11.44777988621623521 ) ) ;
#15003 = LINE ( 'NONE', #66732, #97194 ) ;
#15004 = CARTESIAN_POINT ( 'NONE',  ( 5.659515148182856947, -5.356774720517040400, -27.47062408582486270 ) ) ;
#15005 = AXIS2_PLACEMENT_3D ( 'NONE', #82770, #67073, #78019 ) ;
#15006 = LINE ( 'NONE', #55086, #85778 ) ;
#15007 = CARTESIAN_POINT ( 'NONE',  ( -33.52287095715006160, -29.50248528299804818, 1.056150453629029817 ) ) ;
#15008 = LINE ( 'NONE', #29238, #70802 ) ;
#15010 = EDGE_LOOP ( 'NONE', ( #78188, #19633, #55982, #29639 ) ) ;
#15009 = CARTESIAN_POINT ( 'NONE',  ( 22.09269804725545683, -1.632937629565654580, 11.49999999999999645 ) ) ;
#15011 = DIRECTION ( 'NONE',  ( -0.000000000000000000, -1.000000000000000000, -0.000000000000000000 ) ) ;
#15012 = CARTESIAN_POINT ( 'NONE',  ( -1.322449806865925614, 22.60218017400935864, 11.49999999999998934 ) ) ;
#15014 = ORIENTED_EDGE ( 'NONE', *, *, #17155, .F. ) ;
#15013 = CARTESIAN_POINT ( 'NONE',  ( -124.5562042904833930, -23.47593901973091235, -1.443836447538997536 ) ) ;
#15015 = ORIENTED_EDGE ( 'NONE', *, *, #87125, .T. ) ;
#15016 = CARTESIAN_POINT ( 'NONE',  ( -67.62287095715008434, -23.47596703998600276, 11.44779298504227505 ) ) ;
#15017 = VECTOR ( 'NONE', #4691, 1000.000000000000114 ) ;
#15018 = CARTESIAN_POINT ( 'NONE',  ( 13.10547390533899836, 15.29217475743441312, -1.500000000000002220 ) ) ;
#15019 = LINE ( 'NONE', #61225, #52196 ) ;
#15020 = ORIENTED_EDGE ( 'NONE', *, *, #98126, .F. ) ;
#15021 = DIRECTION ( 'NONE',  ( -1.000000000000000000, 0.000000000000000000, 0.000000000000000000 ) ) ;
#15022 = CARTESIAN_POINT ( 'NONE',  ( 20.54922051473491607, -8.805037660420627077, -1.500000000000002220 ) ) ;
#15023 = ORIENTED_EDGE ( 'NONE', *, *, #7045, .F. ) ;
#15024 = ORIENTED_EDGE ( 'NONE', *, *, #42237, .F. ) ;
#15025 = CARTESIAN_POINT ( 'NONE',  ( -101.5158928754072605, -25.25341126112779122, 6.338294183601393073 ) ) ;
#15027 = CARTESIAN_POINT ( 'NONE',  ( -121.6228709571500417, -29.50250243563736774, 8.947779886222134493 ) ) ;
#15026 = AXIS2_PLACEMENT_3D ( 'NONE', #80879, #58059, #19466 ) ;
#15028 = CARTESIAN_POINT ( 'NONE',  ( -85.62287095715005592, -23.47596703998600631, 11.44779298504227860 ) ) ;
#15029 = DIRECTION ( 'NONE',  ( 0.000000000000000000, -2.173523156925979552E-06, 0.9999999999976378895 ) ) ;
#15030 = CARTESIAN_POINT ( 'NONE',  ( 15.00000000000000355, 19.30000000000000071, 0.000000000000000000 ) ) ;
#15031 = B_SPLINE_CURVE_WITH_KNOTS ( 'NONE', 3,
 ( #99861, #28876, #45114, #5531, #68936, #99375, #76032, #59329 ),
 .UNSPECIFIED., .F., .F.,
 ( 4, 2, 2, 4 ),
 ( -0.001240355328176877226, -0.0002398155169399624007, 0.0007607242942969524250, 0.002761803916770786196 ),
 .UNSPECIFIED. ) ;
#15032 = CARTESIAN_POINT ( 'NONE',  ( 19.26631176993168282, 3.279242639417544236, 11.49999999999998934 ) ) ;
#15033 = VECTOR ( 'NONE', #84439, 1000.000000000000000 ) ;
#15034 = CARTESIAN_POINT ( 'NONE',  ( -5.837039262820512775, -5.876774720514413630, 19.76512419871795245 ) ) ;
#15035 = CARTESIAN_POINT ( 'NONE',  ( -18.34654256122676941, -11.15389649534839833, 11.49999999999998934 ) ) ;
#15036 = FACE_OUTER_BOUND ( 'NONE', #31704, .T. ) ;
#15037 = CARTESIAN_POINT ( 'NONE',  ( 27.53860345374808105, -1.682774720514426114, -8.321925749325325583 ) ) ;
#15038 = FACE_BOUND ( 'NONE', #37865, .T. ) ;
#15039 = CARTESIAN_POINT ( 'NONE',  ( 0.7049041324096299022, -22.85584899170066109, -1.500000000000002220 ) ) ;
#15040 = CALENDAR_DATE ( 2026, 9, 10 ) ;
#15041 = PLANE ( 'NONE',  #15856 ) ;
#15042 = CARTESIAN_POINT ( 'NONE',  ( -127.5895376238167245, -23.47593901973091235, -1.443836447538995760 ) ) ;
#15043 = CARTESIAN_POINT ( 'NONE',  ( -19.32702923155483177, -5.217993511516596961, 11.49999999999999645 ) ) ;
#15044 = CARTESIAN_POINT ( 'NONE',  ( -79.09669456484505190, -25.31594480037252382, 5.260499919381111944 ) ) ;
#15045 = FACE_OUTER_BOUND ( 'NONE', #33845, .T. ) ;
#15046 = EDGE_CURVE ( 'NONE', #33754, #63555, #76887, .T. ) ;
#15047 = ADVANCED_FACE ( 'NONE', ( #829 ), #40973, .T. ) ;
#15048 = DIRECTION ( 'NONE',  ( -0.000000000000000000, 1.000000000000000000, -0.000000000000000000 ) ) ;
#15049 = LINE ( 'NONE', #67360, #69955 ) ;
#15050 = ORIENTED_EDGE ( 'NONE', *, *, #1879, .T. ) ;
#15051 = CARTESIAN_POINT ( 'NONE',  ( -109.5228709571500758, -24.50216790748205042, 0.6166512839542608315 ) ) ;
#15052 = CARTESIAN_POINT ( 'NONE',  ( -115.6228709571500275, -23.85229601348996908, 10.88205029486208275 ) ) ;
#15053 = ADVANCED_FACE ( 'NONE', ( #31274 ), #84560, .F. ) ;
#15054 = CARTESIAN_POINT ( 'NONE',  ( 16.02445091669267185, 14.69945503153335764, 11.49999999999998934 ) ) ;
#15055 = CARTESIAN_POINT ( 'NONE',  ( 30.93860345374796594, 0.6647747205144264315, 19.84760796525321780 ) ) ;
#15056 = CARTESIAN_POINT ( 'NONE',  ( 11.71876819965036809, 15.69520123712499249, -1.500000000000002220 ) ) ;
#15057 = EDGE_CURVE ( 'NONE', #93291, #94842, #32278, .T. ) ;
#15058 = CARTESIAN_POINT ( 'NONE',  ( -113.6228709571500559, -29.50247984919015209, -1.443849546365048253 ) ) ;
#15059 = EDGE_CURVE ( 'NONE', #52488, #18110, #32154, .T. ) ;
#15060 = VECTOR ( 'NONE', #13550, 1000.000000000000000 ) ;
#15061 = CARTESIAN_POINT ( 'NONE',  ( -110.1668890976376360, -25.27925955908359157, 5.541054292275473969 ) ) ;
#15062 = COORDINATED_UNIVERSAL_TIME_OFFSET ( 0, 0, .AHEAD. ) ;
#15063 = CARTESIAN_POINT ( 'NONE',  ( 18.09022303007301247, 14.20294132079179938, -1.500000000000002220 ) ) ;
#15064 = LINE ( 'NONE', #46032, #22428 ) ;
#15065 = CARTESIAN_POINT ( 'NONE',  ( 2.832419239133125544, -6.376774720514422512, 21.23415460623727213 ) ) ;
#15066 = CARTESIAN_POINT ( 'NONE',  ( -4.863915844574979275, 19.94883092034378791, 11.49999999999999645 ) ) ;
#15067 = CARTESIAN_POINT ( 'NONE',  ( -39.56136241089613748, -25.30385213834873781, 5.536731319770037629 ) ) ;
#15068 = CARTESIAN_POINT ( 'NONE',  ( -33.62287095715005592, -29.50247984919015209, -1.443849546365062242 ) ) ;
#15069 = B_SPLINE_CURVE_WITH_KNOTS ( 'NONE', 3,
 ( #89992, #35215, #36704, #50943 ),
 .UNSPECIFIED., .F., .F.,
 ( 4, 4 ),
 ( 0.3100072930973782892, 0.3190137243694937119 ),
 .UNSPECIFIED. ) ;
#15070 = VECTOR ( 'NONE', #35043, 1000.000000000000114 ) ;
#15071 = ORIENTED_EDGE ( 'NONE', *, *, #216, .F. ) ;
#15072 = CARTESIAN_POINT ( 'NONE',  ( -62.52287095715009002, -24.33927499327855415, 9.819080762295815390 ) ) ;
#15073 = PLANE ( 'NONE',  #25074 ) ;
#15074 = CARTESIAN_POINT ( 'NONE',  ( -125.6236347618411031, -24.92592662359561828, 8.075495903018000021 ) ) ;
#15075 = DIRECTION ( 'NONE',  ( 0.000000000000000000, -0.000000000000000000, -1.000000000000000000 ) ) ;
#15076 = AXIS2_PLACEMENT_3D ( 'NONE', #12652, #43118, #76039 ) ;
#15077 = EDGE_CURVE ( 'NONE', #96155, #47456, #95063, .T. ) ;
#15078 = CARTESIAN_POINT ( 'NONE',  ( -34.62287095715005592, -29.50250243563736774, 8.947779886222150481 ) ) ;
#15079 = CARTESIAN_POINT ( 'NONE',  ( 32.15269211224249091, 4.540774720514427543, 3.401810532325273861 ) ) ;
#15080 = EDGE_CURVE ( 'NONE', #41466, #11793, #24655, .T. ) ;
#15081 = CARTESIAN_POINT ( 'NONE',  ( 15.83906049732654608, 16.74391201645830662, 11.49999999999999645 ) ) ;
#15082 = CARTESIAN_POINT ( 'NONE',  ( -16.48365427610503886, -15.78576583860491489, 11.49999999999998934 ) ) ;
#15083 = CARTESIAN_POINT ( 'NONE',  ( 4.451706829556401956, -5.876774720514407413, 18.91922570401084513 ) ) ;
#15084 = B_SPLINE_SURFACE_WITH_KNOTS ( 'NONE', 3, 3, ( 
 ( #1821, #9414, #32257, #64238 ),
 ( #79426, #94149, #18032, #86543 ),
 ( #32757, #94657, #88056, #80437 ),
 ( #17030, #39872, #95162, #96165 ),
 ( #25135, #56118, #87043, #34272 ),
 ( #17534, #41381, #26655, #19029 ),
 ( #87550, #49000, #10926, #72335 ) ),
 .UNSPECIFIED., .F., .F., .F.,
 ( 4, 3, 4 ),
 ( 4, 4 ),
 ( 0.7945040050992235869, 0.8970133687736495665, 0.9995227324480755460 ),
 ( 0.1795396207514014797, 0.1806352327094073451 ),
 .UNSPECIFIED. ) ;
#15085 = CARTESIAN_POINT ( 'NONE',  ( -5.053929855541893446, -6.376774720514408301, 19.14848118821636547 ) ) ;
#15086 = LINE ( 'NONE', #61284, #79226 ) ;
#15087 = CARTESIAN_POINT ( 'NONE',  ( 1.585521478320181865, 22.38520322874704149, 11.49999999999999645 ) ) ;
#15088 = PLANE ( 'NONE',  #67414 ) ;
#15089 = PLANE ( 'NONE',  #10894 ) ;
#15090 = CARTESIAN_POINT ( 'NONE',  ( -21.55542221127511482, -4.010009934288176758, -1.500000000000002220 ) ) ;
#15091 = B_SPLINE_CURVE_WITH_KNOTS ( 'NONE', 3,
 ( #8026, #7030, #92757, #22736, #53722, #84651 ),
 .UNSPECIFIED., .F., .F.,
 ( 4, 2, 4 ),
 ( 1.570755371633836552E-05, 0.001396183895866087536, 0.002776660238015836446 ),
 .UNSPECIFIED. ) ;
#15092 = CARTESIAN_POINT ( 'NONE',  ( -5.115065434581078208, -6.376774720514410077, 19.15054976246387497 ) ) ;
#15093 = B_SPLINE_CURVE_WITH_KNOTS ( 'NONE', 3,
 ( #12611, #81633, #43573, #82128 ),
 .UNSPECIFIED., .F., .F.,
 ( 4, 4 ),
 ( 0.3890439316126428348, 0.3900446786534081389 ),
 .UNSPECIFIED. ) ;
#15094 = CARTESIAN_POINT ( 'NONE',  ( -87.58323056378104354, -24.66019654487200441, 8.947790411086112172 ) ) ;
#15095 = CARTESIAN_POINT ( 'NONE',  ( -33.52287095715006160, -24.66019654487198665, 8.947790411086131712 ) ) ;
#15096 = CARTESIAN_POINT ( 'NONE',  ( -48.87380231474225667, -25.25252557466923520, 6.137092008254006359 ) ) ;
#15097 = CARTESIAN_POINT ( 'NONE',  ( -117.6228709571500559, -23.47593901973091235, -1.443836447538997536 ) ) ;
#15098 = ORIENTED_EDGE ( 'NONE', *, *, #48935, .T. ) ;
#15099 = CARTESIAN_POINT ( 'NONE',  ( -11.47117155886032158, -16.94740806926979815, -1.500000000000002220 ) ) ;
#15100 = ORIENTED_EDGE ( 'NONE', *, *, #2828, .F. ) ;
#15101 = ORIENTED_EDGE ( 'NONE', *, *, #54767, .T. ) ;
#15102 = ORIENTED_EDGE ( 'NONE', *, *, #86072, .F. ) ;
#15103 = ORIENTED_EDGE ( 'NONE', *, *, #19962, .F. ) ;
#15104 = CARTESIAN_POINT ( 'NONE',  ( -22.28253579152010033, 6.022996098971622914, -1.500000000000002220 ) ) ;
#15105 = CARTESIAN_POINT ( 'NONE',  ( -41.47729125475370182, -25.30524842186639844, 5.093185296294494790 ) ) ;
#15106 = CARTESIAN_POINT ( 'NONE',  ( 19.34776771173714849, 6.126202725962671458, -1.500000000000002220 ) ) ;
#15107 = AXIS2_PLACEMENT_3D ( 'NONE', #87514, #63189, #772 ) ;
#15108 = ORIENTED_EDGE ( 'NONE', *, *, #9431, .T. ) ;
#15109 = CARTESIAN_POINT ( 'NONE',  ( -28.20246834257805091, -25.12682770457861281, 5.848370260082334404 ) ) ;
#15110 = FACE_OUTER_BOUND ( 'NONE', #12491, .T. ) ;
#15111 = EDGE_CURVE ( 'NONE', #64856, #98355, #93800, .T. ) ;
#15112 = CARTESIAN_POINT ( 'NONE',  ( -28.52287095715005805, -23.31185441368106126, 11.44779303854528685 ) ) ;
#15113 = CARTESIAN_POINT ( 'NONE',  ( -99.63196111833542545, -23.96169478059713498, 10.65365249895717703 ) ) ;
#15115 = ORIENTED_EDGE ( 'NONE', *, *, #59567, .T. ) ;
#15114 = CARTESIAN_POINT ( 'NONE',  ( -20.78045986758521835, -5.208592277829342088, 11.49999999999999645 ) ) ;
#15116 = CARTESIAN_POINT ( 'NONE',  ( -100.5228709571500758, -23.47593901973090524, -1.443836447538996648 ) ) ;
#15118 = VECTOR ( 'NONE', #20425, 1000.000000000000000 ) ;
#15117 = CARTESIAN_POINT ( 'NONE',  ( -111.5228709571500616, -23.47593901973090524, -1.443836447538996204 ) ) ;
#15119 = ORIENTED_EDGE ( 'NONE', *, *, #56365, .F. ) ;
#15120 = CARTESIAN_POINT ( 'NONE',  ( -4.968023186724614959, -20.10795263665959709, 11.49999999999998934 ) ) ;
#15121 = EDGE_CURVE ( 'NONE', #94877, #53498, #707, .T. ) ;
#15122 = ORIENTED_EDGE ( 'NONE', *, *, #76000, .T. ) ;
#15124 = ORIENTED_EDGE ( 'NONE', *, *, #64696, .F. ) ;
#15123 = CARTESIAN_POINT ( 'NONE',  ( -123.6228709571500701, -23.96127896941632685, -0.6493128931037793761 ) ) ;
#15125 = DIRECTION ( 'NONE',  ( -2.501730345825856179E-15, 6.879758451021104590E-15, -1.000000000000000000 ) ) ;
#15126 = VERTEX_POINT ( 'NONE', #38886 ) ;
#15127 = VERTEX_POINT ( 'NONE', #41401 ) ;
#15128 = CARTESIAN_POINT ( 'NONE',  ( 4.740341618695937065, -5.876774720514402972, 18.75174579344860248 ) ) ;
#15129 = CARTESIAN_POINT ( 'NONE',  ( -76.52287095715007581, -23.96177878511308634, 10.65340807706329684 ) ) ;
#15130 = CARTESIAN_POINT ( 'NONE',  ( 5.197331492371871420, 21.31670716312865466, 11.49999999999999645 ) ) ;
#15131 = LINE ( 'NONE', #30354, #25239 ) ;
#15132 = CARTESIAN_POINT ( 'NONE',  ( 6.619388286264371146, -21.57091762011834390, -1.500000000000002220 ) ) ;
#15133 = CARTESIAN_POINT ( 'NONE',  ( -16.09219062524700661, 13.46031615953476468, -1.500000000000002220 ) ) ;
#15134 = CARTESIAN_POINT ( 'NONE',  ( -26.91814428177455909, 0.3587747205144265483, 29.98490496616818746 ) ) ;
#15135 = VECTOR ( 'NONE', #92192, 1000.000000000000114 ) ;
#15136 = DIRECTION ( 'NONE',  ( 0.000000000000000000, -2.173523156925980399E-06, 0.9999999999976378895 ) ) ;
#15137 = ORIENTED_EDGE ( 'NONE', *, *, #49814, .T. ) ;
#15138 = ORIENTED_EDGE ( 'NONE', *, *, #55520, .F. ) ;
#15139 = ORIENTED_EDGE ( 'NONE', *, *, #22351, .T. ) ;
#15140 = CARTESIAN_POINT ( 'NONE',  ( 31.55236408230781819, -6.376774720514426953, 19.84760796525321780 ) ) ;
#15141 = CARTESIAN_POINT ( 'NONE',  ( -5.740839400147730309, 20.75665450205591966, -1.500000000000002220 ) ) ;
#15142 = LINE ( 'NONE', #32372, #68418 ) ;
#15143 = VERTEX_POINT ( 'NONE', #25159 ) ;
#15144 = CARTESIAN_POINT ( 'NONE',  ( -20.44436638909326120, 5.324712401148210539, 11.49999999999998934 ) ) ;
#15145 = DIRECTION ( 'NONE',  ( 0.000000000000000000, 0.000000000000000000, -1.000000000000000000 ) ) ;
#15146 = DIRECTION ( 'NONE',  ( -3.773278334453079618E-23, 0.9999999999976377785, 2.173523156925979975E-06 ) ) ;
#15147 = DIRECTION ( 'NONE',  ( -1.000000000000000000, -0.000000000000000000, 0.000000000000000000 ) ) ;
#15148 = DIRECTION ( 'NONE',  ( 0.000000000000000000, -0.3081562241202474572, -0.9513357669802769978 ) ) ;
#15149 = CARTESIAN_POINT ( 'NONE',  ( -73.62287095715005592, -29.50247984919015209, -1.443849546365055359 ) ) ;
#15150 = CARTESIAN_POINT ( 'NONE',  ( 19.88262469969689050, -9.776007750257504014, -1.500000000000002220 ) ) ;
#15151 = AXIS2_PLACEMENT_3D ( 'NONE', #47616, #15148, #68942 ) ;
#15152 = CARTESIAN_POINT ( 'NONE',  ( -71.63518065170222826, -24.15543982623907127, -0.2315651400026636497 ) ) ;
#15153 = ORIENTED_EDGE ( 'NONE', *, *, #54147, .T. ) ;
#15154 = CARTESIAN_POINT ( 'NONE',  ( -51.88058966555665563, -25.24860181553395932, 5.810524397698039856 ) ) ;
#15155 = CARTESIAN_POINT ( 'NONE',  ( 11.96746718618548577, 4.832654890647344104, -27.30666805081000348 ) ) ;
#15156 = DIRECTION ( 'NONE',  ( -0.000000000000000000, 1.000000000000000000, -0.000000000000000000 ) ) ;
#15157 = CARTESIAN_POINT ( 'NONE',  ( -100.6278572774885589, -24.63355581998384380, 0.9682620441943933232 ) ) ;
#15158 = CARTESIAN_POINT ( 'NONE',  ( 15.33136405852079243, -11.96835230219363311, 11.49999999999998934 ) ) ;
#15159 = CARTESIAN_POINT ( 'NONE',  ( 18.17913347391500523, 11.28257676469832660, -1.500000000000002220 ) ) ;
#15160 = CARTESIAN_POINT ( 'NONE',  ( -62.64210508241590958, -23.96119346886881019, -0.6495511937832098015 ) ) ;
#15161 = FACE_BOUND ( 'NONE', #27271, .T. ) ;
#15162 = CARTESIAN_POINT ( 'NONE',  ( -79.62287095715001328, -24.51283580621365843, 0.6167428607019644904 ) ) ;
#15163 = CARTESIAN_POINT ( 'NONE',  ( -101.3340698065965455, -25.27360105556784475, 3.896482660342662996 ) ) ;
#15164 = CARTESIAN_POINT ( 'NONE',  ( -18.45961786539058380, -13.25243217869837231, -1.500000000000002220 ) ) ;
#15165 = B_SPLINE_SURFACE_WITH_KNOTS ( 'NONE', 3, 3, ( 
 ( #36958, #73644, #65560, #11732 ),
 ( #19835, #57938, #88877, #57441 ),
 ( #19349, #66056, #50315, #95978 ),
 ( #81251, #67927, #83120, #50812 ),
 ( #95478, #42710, #96976, #56936 ),
 ( #27477, #25964, #72652, #13610 ),
 ( #44578, #75506, #88369, #98847 ) ),
 .UNSPECIFIED., .F., .F., .F.,
 ( 4, 3, 4 ),
 ( 4, 4 ),
 ( 0.0004766839783834271615, 0.1029713700210900945, 0.2054660560637967537 ),
 ( 0.8897203268989763991, 0.8911435667790393866 ),
 .UNSPECIFIED. ) ;
#15166 = CARTESIAN_POINT ( 'NONE',  ( -93.52287095715006160, -24.64898659630368272, 1.056161002820827921 ) ) ;
#15167 = FACE_OUTER_BOUND ( 'NONE', #46210, .T. ) ;
#15168 = CARTESIAN_POINT ( 'NONE',  ( -12.90690225449951001, 15.05119527412115055, 11.49999999999999645 ) ) ;
#15169 = EDGE_CURVE ( 'NONE', #22949, #32255, #55955, .T. ) ;
#15170 = CARTESIAN_POINT ( 'NONE',  ( 32.45853543194704116, -5.965225279485572685, 9.169203677920338080 ) ) ;
#15171 = VERTEX_POINT ( 'NONE', #42907 ) ;
#15172 = CARTESIAN_POINT ( 'NONE',  ( -60.52287095715006870, -24.63287334234176740, 0.9662140553045375224 ) ) ;
#15173 = LINE ( 'NONE', #52748, #8555 ) ;
#15174 = AXIS2_PLACEMENT_3D ( 'NONE', #99368, #29860, #7026 ) ;
#15175 = EDGE_CURVE ( 'NONE', #24103, #16838, #46235, .T. ) ;
#15176 = CARTESIAN_POINT ( 'NONE',  ( 10.24059822343757808, -5.876774720514426953, 17.17691942396160698 ) ) ;
#15177 = CARTESIAN_POINT ( 'NONE',  ( 5.966611984012316405, 20.80180421262142687, -1.500000000000002220 ) ) ;
#15178 = DIRECTION ( 'NONE',  ( -3.773278334453079618E-23, 0.9999999999976377785, 2.173523156925979975E-06 ) ) ;
#15179 = CARTESIAN_POINT ( 'NONE',  ( -10.03281922573575002, -16.61734169602722488, -1.500000000000002220 ) ) ;
#15180 = EDGE_CURVE ( 'NONE', #74207, #20296, #28412, .T. ) ;
#15181 = CARTESIAN_POINT ( 'NONE',  ( -79.62287095715005592, -29.50250243563736774, 8.947779886222141599 ) ) ;
#15182 = CARTESIAN_POINT ( 'NONE',  ( -48.52287095715006160, -29.50248528299804818, 1.056150453629033370 ) ) ;
#15183 = CARTESIAN_POINT ( 'NONE',  ( 8.478510716907816658, 17.93336729499101523, 11.49999999999998934 ) ) ;
#15184 = VERTEX_POINT ( 'NONE', #26677 ) ;
#15185 = VECTOR ( 'NONE', #30885, 999.9999999999998863 ) ;
#15186 = EDGE_CURVE ( 'NONE', #65785, #65683, #2851, .T. ) ;
#15187 = CARTESIAN_POINT ( 'NONE',  ( -0.6891947355827284794, 20.32259304938107292, 11.49999999999999645 ) ) ;
#15188 = CARTESIAN_POINT ( 'NONE',  ( -80.65304186593860436, -23.48783264082476308, -1.443836473390095687 ) ) ;
#15189 = EDGE_CURVE ( 'NONE', #71759, #4176, #33784, .T. ) ;
#15190 = CARTESIAN_POINT ( 'NONE',  ( 33.37790122608239329, -4.268345726061002487, -11.54778842029335806 ) ) ;
#15191 = ORIENTED_EDGE ( 'NONE', *, *, #9557, .F. ) ;
#15192 = CARTESIAN_POINT ( 'NONE',  ( 0.01195862986790833214, -23.20481386120385636, 3.825958421598584902 ) ) ;
#15193 = CARTESIAN_POINT ( 'NONE',  ( -62.58953762381672448, -24.64898659630528854, 1.056161002820822814 ) ) ;
#15194 = CARTESIAN_POINT ( 'NONE',  ( -48.88506298778586512, -25.25214647875201379, 5.954471609515935349 ) ) ;
#15195 = CARTESIAN_POINT ( 'NONE',  ( -40.50923893080022964, -23.85049219812685095, 10.88485053497527488 ) ) ;
#15196 = CARTESIAN_POINT ( 'NONE',  ( -0.5315124411682757843, -5.876774720514411854, 19.46509473978807847 ) ) ;
#15197 = CARTESIAN_POINT ( 'NONE',  ( -12.91570554291229023, -15.35452705144416896, 11.49999999999998934 ) ) ;
#15198 = ADVANCED_FACE ( 'NONE', ( #34292 ), #32780, .T. ) ;
#15199 = VECTOR ( 'NONE', #50550, 1000.000000000000000 ) ;
#15200 = DIRECTION ( 'NONE',  ( -0.000000000000000000, 2.173523156925979552E-06, -0.9999999999976378895 ) ) ;
#15201 = ORIENTED_EDGE ( 'NONE', *, *, #15433, .T. ) ;
#15202 = DIRECTION ( 'NONE',  ( -1.000000000000000000, -0.000000000000000000, -0.000000000000000000 ) ) ;
#15203 = ADVANCED_FACE ( 'NONE', ( #25667 ), #72856, .F. ) ;
#15204 = CARTESIAN_POINT ( 'NONE',  ( -14.01358469492184966, -18.07645309290061064, 11.49999999999999645 ) ) ;
#15205 = CARTESIAN_POINT ( 'NONE',  ( 15.30562342774392093, -16.77826389816909725, -1.500000000000002220 ) ) ;
#15206 = ORIENTED_EDGE ( 'NONE', *, *, #29838, .T. ) ;
#15207 = LINE ( 'NONE', #15708, #48638 ) ;
#15208 = DIRECTION ( 'NONE',  ( -0.000000000000000000, -0.000000000000000000, 1.000000000000000000 ) ) ;
#15209 = CARTESIAN_POINT ( 'NONE',  ( -38.57582415398436382, -24.66019654487198665, 8.947790411086121054 ) ) ;
#15210 = B_SPLINE_CURVE_WITH_KNOTS ( 'NONE', 3,
 ( #4863, #52038, #19077, #74855, #36313, #11471, #98191, #81985, #34318, #42445, #43437, #42939, #51046, #73873, #59661, #19577, #65788, #82476 ),
 .UNSPECIFIED., .F., .F.,
 ( 4, 2, 2, 2, 2, 2, 2, 2, 4 ),
 ( 1.411962612463446054E-17, 0.0004122230507468467478, 0.0006183345761202429895, 0.0008244461014936392855, 0.001030557626867035365, 0.001236669152240431552, 0.001442780677613827956, 0.001545836440300521822, 0.001648892202987215470 ),
 .UNSPECIFIED. ) ;
#15211 = PLANE ( 'NONE',  #64381 ) ;
#15212 = LINE ( 'NONE', #16712, #64083 ) ;
#15213 = AXIS2_PLACEMENT_3D ( 'NONE', #82563, #26290, #43020 ) ;
#15214 = DIRECTION ( 'NONE',  ( 0.000000000000000000, 0.000000000000000000, 1.000000000000000000 ) ) ;
#15215 = ORIENTED_EDGE ( 'NONE', *, *, #96965, .F. ) ;
#15216 = CARTESIAN_POINT ( 'NONE',  ( -0.9335293527496063559, -20.33857301660709638, 11.49999999999998934 ) ) ;
#15217 = AXIS2_PLACEMENT_3D ( 'NONE', #38509, #30895, #61862 ) ;
#15218 = VERTEX_POINT ( 'NONE', #81466 ) ;
#15219 = EDGE_CURVE ( 'NONE', #91196, #77233, #48522, .T. ) ;
#15220 = CARTESIAN_POINT ( 'NONE',  ( -21.12268324108725892, 9.058254180033936009, 11.49999999999998934 ) ) ;
#15221 = CARTESIAN_POINT ( 'NONE',  ( -88.52287095715006160, -24.64898659630367916, 1.056161002820827921 ) ) ;
#15222 = VERTEX_POINT ( 'NONE', #18055 ) ;
#15223 = CARTESIAN_POINT ( 'NONE',  ( -108.5876495711624301, -24.51419770103158768, 9.386484678747162747 ) ) ;
#15224 = CARTESIAN_POINT ( 'NONE',  ( -77.62361616268356102, -24.66019654487200441, 8.947790411086108620 ) ) ;
#15225 = CARTESIAN_POINT ( 'NONE',  ( -51.59924249663487217, -23.96169478059713143, 10.65365249895718236 ) ) ;
#15227 = ORIENTED_EDGE ( 'NONE', *, *, #22285, .T. ) ;
#15226 = CARTESIAN_POINT ( 'NONE',  ( -10.85727797829764185, 18.24708236899833835, 11.49999999999999645 ) ) ;
#15228 = EDGE_LOOP ( 'NONE', ( #31010, #3310, #93741, #66167 ) ) ;
#15229 = CARTESIAN_POINT ( 'NONE',  ( -0.9571703918902072505, -22.19477237104690914, 11.49999999999998934 ) ) ;
#15230 = CARTESIAN_POINT ( 'NONE',  ( -18.12278953325389708, -9.833843834435361586, -1.500000000000002220 ) ) ;
#15231 = ORIENTED_EDGE ( 'NONE', *, *, #70564, .T. ) ;
#15232 = EDGE_LOOP ( 'NONE', ( #35832, #16717, #8866, #44029 ) ) ;
#15233 = CARTESIAN_POINT ( 'NONE',  ( -108.9545715455115129, -25.31627118360455597, 4.170144754312187452 ) ) ;
#15234 = EDGE_CURVE ( 'NONE', #12369, #7140, #5566, .T. ) ;
#15235 = CARTESIAN_POINT ( 'NONE',  ( 2.649863049427662709, -5.876774720514419847, 20.71861240329949538 ) ) ;
#15236 = ORIENTED_EDGE ( 'NONE', *, *, #96905, .F. ) ;
#15237 = CARTESIAN_POINT ( 'NONE',  ( -91.55469558775585881, -23.96119346886880663, -0.6495511937832073590 ) ) ;
#15238 = VERTEX_POINT ( 'NONE', #63760 ) ;
#15239 = CARTESIAN_POINT ( 'NONE',  ( 30.57287095715020087, 6.475225279485571583, 25.41160796525326404 ) ) ;
#15240 = CARTESIAN_POINT ( 'NONE',  ( -44.52287095715006160, -23.47593901973090169, -1.443836447538997092 ) ) ;
#15241 = CARTESIAN_POINT ( 'NONE',  ( 3.748101851616784774, 20.49759516964078188, -1.500000000000002220 ) ) ;
#15243 = EDGE_CURVE ( 'NONE', #5514, #30477, #41889, .T. ) ;
#15242 = CARTESIAN_POINT ( 'NONE',  ( -7.892909027492730267, -20.28523913882780505, 11.49999999999999645 ) ) ;
#15244 = CARTESIAN_POINT ( 'NONE',  ( -102.6228709571500417, -23.48786465467241769, 11.44779295918253936 ) ) ;
#15245 = CARTESIAN_POINT ( 'NONE',  ( -78.60557720441329366, -23.48786465467241058, 11.44779295918254469 ) ) ;
#15246 = CARTESIAN_POINT ( 'NONE',  ( -21.66288588771858770, -5.991481186202806342, 11.49999999999998934 ) ) ;
#15247 = CARTESIAN_POINT ( 'NONE',  ( -118.6241804900995191, -24.51419770103160189, 9.386484678747168076 ) ) ;
#15248 = EDGE_LOOP ( 'NONE', ( #9964, #73663, #60686, #30349 ) ) ;
#15249 = DIRECTION ( 'NONE',  ( 0.1254312216594016538, 0.000000000000000000, 0.9921023176230513441 ) ) ;
#15250 = CARTESIAN_POINT ( 'NONE',  ( -69.52287095715006160, -23.47596703998600631, 11.44779298504228748 ) ) ;
#15251 = B_SPLINE_CURVE_WITH_KNOTS ( 'NONE', 3,
 ( #66448, #96368, #57825, #90752 ),
 .UNSPECIFIED., .F., .F.,
 ( 4, 4 ),
 ( 1.387778780781445521E-17, 9.999999999997510880E-05 ),
 .UNSPECIFIED. ) ;
#15252 = VECTOR ( 'NONE', #84355, 1000.000000000000114 ) ;
#15253 = ORIENTED_EDGE ( 'NONE', *, *, #85300, .T. ) ;
#15254 = VERTEX_POINT ( 'NONE', #65758 ) ;
#15255 = APPROVAL ( #16551, 'UNKNOWN' ) ;
#15256 = ORIENTED_EDGE ( 'NONE', *, *, #29467, .T. ) ;
#15257 = CARTESIAN_POINT ( 'NONE',  ( -13.37813101364405100, 16.61575060780308277, -1.500000000000002220 ) ) ;
#15258 = ORIENTED_EDGE ( 'NONE', *, *, #77612, .T. ) ;
#15259 = CARTESIAN_POINT ( 'NONE',  ( -20.11743356864677423, -6.099313207006018089, -1.500000000000002220 ) ) ;
#15260 = CARTESIAN_POINT ( 'NONE',  ( -30.51821544575032519, -25.31106951508110825, 3.857144010898052588 ) ) ;
#15261 = CARTESIAN_POINT ( 'NONE',  ( -110.6087918725420423, -25.19910796341628156, 3.322910391071347114 ) ) ;
#15262 = CARTESIAN_POINT ( 'NONE',  ( -79.11611000704996854, -25.13069340115296058, 2.947789388436138580 ) ) ;
#15263 = CARTESIAN_POINT ( 'NONE',  ( -18.59763704738199408, -11.70098744416181979, -1.500000000000002220 ) ) ;
#15264 = CARTESIAN_POINT ( 'NONE',  ( -36.52287095715006870, -23.47593901973090169, -1.443836447538997314 ) ) ;
#15265 = ORIENTED_EDGE ( 'NONE', *, *, #37907, .F. ) ;
#15266 = FACE_OUTER_BOUND ( 'NONE', #12621, .T. ) ;
#15267 = DIRECTION ( 'NONE',  ( -0.000000000000000000, 1.000000000000000000, -0.000000000000000000 ) ) ;
#15268 = CARTESIAN_POINT ( 'NONE',  ( 31.64388307978972747, -6.098167052574009261, 27.71102684943996053 ) ) ;
#15269 = DIRECTION ( 'NONE',  ( 0.000000000000000000, -1.000000000000000000, 0.000000000000000000 ) ) ;
#15270 = CARTESIAN_POINT ( 'NONE',  ( -20.41428188797595311, -24.04316117960158650, 8.370978854367628230 ) ) ;
#15271 = CARTESIAN_POINT ( 'NONE',  ( -15.80959461918071618, 14.24510877297761446, 11.49999999999998934 ) ) ;
#15272 = CARTESIAN_POINT ( 'NONE',  ( -31.24388727629350626, -25.30412371111346204, 3.891793866089567455 ) ) ;
#15273 = DIRECTION ( 'NONE',  ( 0.000000000000000000, 0.000000000000000000, -1.000000000000000000 ) ) ;
#15274 = FACE_OUTER_BOUND ( 'NONE', #83079, .T. ) ;
#15275 = CARTESIAN_POINT ( 'NONE',  ( -29.52287095715006870, -23.40099448348795264, -1.443836171194820883 ) ) ;
#15276 = CARTESIAN_POINT ( 'NONE',  ( 9.939345090160914609, -20.19931669485651682, -1.500000000000002220 ) ) ;
#15277 = CARTESIAN_POINT ( 'NONE',  ( -111.9718182513300775, -25.21970293610405633, 6.713732480141158199 ) ) ;
#15278 = VERTEX_POINT ( 'NONE', #40894 ) ;
#15279 = CARTESIAN_POINT ( 'NONE',  ( -51.05357089062000853, -25.31022451930674677, 5.374527235766375810 ) ) ;
#15280 = CARTESIAN_POINT ( 'NONE',  ( -3.586273028688536257, -19.27814873881845514, 11.49999999999999645 ) ) ;
#15281 = DIRECTION ( 'NONE',  ( 0.000000000000000000, -0.9999999999976377785, -2.173523156925979975E-06 ) ) ;
#15282 = CARTESIAN_POINT ( 'NONE',  ( -76.62287095715007013, -24.64965695001468404, 8.947790433994182280 ) ) ;
#15283 = B_SPLINE_CURVE_WITH_KNOTS ( 'NONE', 3,
 ( #58509, #50891, #98036, #80837 ),
 .UNSPECIFIED., .F., .F.,
 ( 4, 4 ),
 ( 0.7403145649873383860, 0.7493209962594540308 ),
 .UNSPECIFIED. ) ;
#15284 = ORIENTED_EDGE ( 'NONE', *, *, #49327, .F. ) ;
#15285 = DIRECTION ( 'NONE',  ( 0.8219392559241306406, -0.5637660281018075370, 0.08114015731558719968 ) ) ;
#15286 = LINE ( 'NONE', #70087, #93373 ) ;
#15287 = CARTESIAN_POINT ( 'NONE',  ( -91.96692758709957616, -25.12049752546737480, 2.832404795212227100 ) ) ;
#15288 = CARTESIAN_POINT ( 'NONE',  ( -0.8432318219891272726, -19.69000482574202238, -1.500000000000002220 ) ) ;
#15289 = ORIENTED_EDGE ( 'NONE', *, *, #70162, .F. ) ;
#15290 = ADVANCED_FACE ( 'NONE', ( #19549 ), #97746, .T. ) ;
#15291 = B_SPLINE_CURVE_WITH_KNOTS ( 'NONE', 3,
 ( #32826, #38932, #55180, #40939 ),
 .UNSPECIFIED., .F., .F.,
 ( 4, 4 ),
 ( 0.000000000000000000, 9.999999999998900014E-05 ),
 .UNSPECIFIED. ) ;
#15292 = CARTESIAN_POINT ( 'NONE',  ( 8.655157120174900243, 3.316774720514428232, -28.10018424651253000 ) ) ;
#15293 = CARTESIAN_POINT ( 'NONE',  ( -118.5228709571501184, -23.73907113216990794, -1.053371485793245244 ) ) ;
#15294 = EDGE_CURVE ( 'NONE', #75526, #80526, #43406, .T. ) ;
#15295 = VECTOR ( 'NONE', #55898, 1000.000000000000000 ) ;
#15296 = PERSON_AND_ORGANIZATION ( #70597, #27821 ) ;
#15297 = ORIENTED_EDGE ( 'NONE', *, *, #13569, .T. ) ;
#15298 = CARTESIAN_POINT ( 'NONE',  ( -6.660000000000001030, 8.793627758918228565, -2.994553991265763049 ) ) ;
#15299 = CARTESIAN_POINT ( 'NONE',  ( -39.52287095715006870, -24.64898659630528144, 1.056161002820819261 ) ) ;
#15300 = CARTESIAN_POINT ( 'NONE',  ( -55.52645498910460020, -25.00158670708910336, 2.256160236439221034 ) ) ;
#15301 = CARTESIAN_POINT ( 'NONE',  ( -86.62287095715004170, -29.50250243563736774, 8.947779886222139822 ) ) ;
#15302 = DIRECTION ( 'NONE',  ( 1.000000000000000000, 3.773278334444167608E-23, 8.201307833595939069E-29 ) ) ;
#15303 = CARTESIAN_POINT ( 'NONE',  ( -94.55620429048339304, -24.65952944569304961, 1.056160979905701236 ) ) ;
#15304 = DIRECTION ( 'NONE',  ( -0.000000000000000000, -1.000000000000000000, 0.000000000000000000 ) ) ;
#15305 = CARTESIAN_POINT ( 'NONE',  ( -15.89961544564849305, 12.09337254111102844, -1.500000000000002220 ) ) ;
#15306 = EDGE_CURVE ( 'NONE', #16795, #73446, #37019, .T. ) ;
#15307 = AXIS2_PLACEMENT_3D ( 'NONE', #42086, #19713, #3517 ) ;
#15308 = DIRECTION ( 'NONE',  ( -1.000000000000000000, -3.491481338843133355E-15, -2.352173255807796056E-16 ) ) ;
#15309 = DIRECTION ( 'NONE',  ( -3.773278334453079030E-23, 0.9999999999976377785, 2.173523156925979128E-06 ) ) ;
#15310 = ORIENTED_EDGE ( 'NONE', *, *, #71554, .T. ) ;
#15311 = DIRECTION ( 'NONE',  ( 0.7512896232465891000, -0.000000000000000000, 0.6599726524652352877 ) ) ;
#15312 = LINE ( 'NONE', #32049, #39379 ) ;
#15313 = CARTESIAN_POINT ( 'NONE',  ( -35.62710011636686147, -23.48783264082477729, -1.443836473390077701 ) ) ;
#15314 = CARTESIAN_POINT ( 'NONE',  ( -106.5895376238167387, -23.48786465467241769, 11.44779295918253759 ) ) ;
#15315 = CARTESIAN_POINT ( 'NONE',  ( 31.48454476783385658, -4.132774720514426292, -1.134026763942596494 ) ) ;
#15316 = CARTESIAN_POINT ( 'NONE',  ( -83.62359966500085307, -24.65952944569305316, 1.056160979905701680 ) ) ;
#15317 = CARTESIAN_POINT ( 'NONE',  ( -81.52287095715006160, -23.47596703998600631, 11.44779298504228571 ) ) ;
#15318 = CARTESIAN_POINT ( 'NONE',  ( 5.328346181807287252, -5.876774720514418071, 20.81670806933143680 ) ) ;
#15319 = ORIENTED_EDGE ( 'NONE', *, *, #79553, .T. ) ;
#15320 = CARTESIAN_POINT ( 'NONE',  ( -18.77428246231291808, -7.638711222589018135, 11.49999999999998934 ) ) ;
#15321 = FACE_BOUND ( 'NONE', #21067, .T. ) ;
#15322 = CARTESIAN_POINT ( 'NONE',  ( 27.53860345374808105, -3.356774720514427823, 1.647607965253212292 ) ) ;
#15323 = CARTESIAN_POINT ( 'NONE',  ( -90.52287095715003318, -24.91544648472626378, 1.928969306349430424 ) ) ;
#15324 = ORIENTED_EDGE ( 'NONE', *, *, #2250, .T. ) ;
#15326 = EDGE_CURVE ( 'NONE', #87201, #5271, #59849, .T. ) ;
#15325 = DIRECTION ( 'NONE',  ( 0.000000000000000000, -1.000000000000000000, 0.000000000000000000 ) ) ;
#15327 = CARTESIAN_POINT ( 'NONE',  ( 20.05498121024909253, 1.910150955369836812, -1.500000000000002220 ) ) ;
#15328 = CARTESIAN_POINT ( 'NONE',  ( 20.99878002148846790, -2.064974809011826729, 11.49999999999999645 ) ) ;
#15329 = VECTOR ( 'NONE', #43883, 1000.000000000000000 ) ;
#15330 = CARTESIAN_POINT ( 'NONE',  ( -64.55620429048339304, -24.66019654487199020, 8.947790411086133489 ) ) ;
#15331 = CARTESIAN_POINT ( 'NONE',  ( 16.06085343747454175, -15.19291221174989204, 11.49999999999998934 ) ) ;
#15332 = EDGE_CURVE ( 'NONE', #33363, #67215, #39774, .T. ) ;
#15333 = CARTESIAN_POINT ( 'NONE',  ( 18.81462172601333549, -8.267562025728075525, -1.500000000000002220 ) ) ;
#15334 = DIRECTION ( 'NONE',  ( -3.773278334453079030E-23, 0.9999999999976377785, 2.173523156925979128E-06 ) ) ;
#15335 = CARTESIAN_POINT ( 'NONE',  ( -60.59908362041784358, -24.15503026093916006, -0.2815557561904390993 ) ) ;
#15336 = ORIENTED_EDGE ( 'NONE', *, *, #73622, .T. ) ;
#15337 = DIRECTION ( 'NONE',  ( 0.000000000000000000, -0.9999999999976377785, -2.173523156925979128E-06 ) ) ;
#15338 = VERTEX_POINT ( 'NONE', #29658 ) ;
#15339 = CARTESIAN_POINT ( 'NONE',  ( 9.150000000000000355, -6.376774720514426953, -15.70000000000000284 ) ) ;
#15340 = B_SPLINE_SURFACE_WITH_KNOTS ( 'NONE', 3, 1, ( 
 ( #10638, #95869 ),
 ( #65455, #27363 ),
 ( #96372, #88772 ),
 ( #19240, #11626 ),
 ( #5573, #82197 ),
 ( #83185, #44642 ),
 ( #60385, #91800 ),
 ( #22276, #91308 ),
 ( #58874, #89814 ),
 ( #29404, #84187 ),
 ( #53259, #97910 ),
 ( #67484, #14678 ),
 ( #74583, #66998 ),
 ( #59369, #20284 ),
 ( #4591, #44144 ) ),
 .UNSPECIFIED., .F., .F., .F.,
 ( 4, 1, 1, 1, 1, 1, 1, 1, 1, 1, 1, 1, 4 ),
 ( 2, 2 ),
 ( 0.000000000000000000, 0.08940971111013579220, 0.1763057644831058923, 0.2626259021834156937, 0.3494457264756534176, 0.4354982637429541947, 0.5189281301037146354, 0.6013546565787400988, 0.6842564217184154973, 0.7658067397968338907, 0.8448768657103881141, 0.9222797948488744568, 1.000000000000000000 ),
 ( 0.000000000000000000, 1.000000000000000000 ),
 .UNSPECIFIED. ) ;
#15341 = CARTESIAN_POINT ( 'NONE',  ( 31.55236408230781819, 0.6647747205144264315, 19.84760796525321780 ) ) ;
#15342 = VERTEX_POINT ( 'NONE', #90067 ) ;
#15343 = ORIENTED_EDGE ( 'NONE', *, *, #23812, .T. ) ;
#15344 = B_SPLINE_CURVE_WITH_KNOTS ( 'NONE', 3,
 ( #57075, #64704, #49462, #73287, #88011, #43340, #18490, #11379 ),
 .UNSPECIFIED., .F., .F.,
 ( 4, 2, 2, 4 ),
 ( 1.199502015590836694E-17, 0.001846270405096679841, 0.003692540810193348840, 0.007385081620386685537 ),
 .UNSPECIFIED. ) ;
#15345 = ORIENTED_EDGE ( 'NONE', *, *, #12664, .T. ) ;
#15346 = CARTESIAN_POINT ( 'NONE',  ( -80.80810375339596874, -25.28533477229251147, 4.196857630783810578 ) ) ;
#15347 = CARTESIAN_POINT ( 'NONE',  ( -49.85452831604734314, -25.04816763092740217, 7.491332617951499628 ) ) ;
#15348 = CARTESIAN_POINT ( 'NONE',  ( -68.64586005558507509, -23.73791477778911840, 11.05961554403170943 ) ) ;
#15349 = CARTESIAN_POINT ( 'NONE',  ( -18.79711486612840332, 8.613068827758688428, -1.500000000000002220 ) ) ;
#15350 = CARTESIAN_POINT ( 'NONE',  ( -19.28869470675124731, 9.786980993800005635, 11.49999999999999645 ) ) ;
#15351 = ORIENTED_EDGE ( 'NONE', *, *, #53126, .T. ) ;
#15352 = PLANE ( 'NONE',  #75841 ) ;
#15353 = CARTESIAN_POINT ( 'NONE',  ( 3.398951772795901771, -5.876774720514403860, 18.23562605320997676 ) ) ;
#15354 = CARTESIAN_POINT ( 'NONE',  ( -7.019573500991415749, 21.25910006591672996, 11.49999999999998934 ) ) ;
#15355 = CARTESIAN_POINT ( 'NONE',  ( -80.15527233487838998, -25.12205802297570401, 7.057878230000818931 ) ) ;
#15356 = CARTESIAN_POINT ( 'NONE',  ( -88.62287095715002749, -24.66019654487199730, 8.947790411086128159 ) ) ;
#15357 = VERTEX_POINT ( 'NONE', #20540 ) ;
#15358 = CARTESIAN_POINT ( 'NONE',  ( -99.61025418334982362, -25.29543586644560094, 4.300707857027740388 ) ) ;
#15359 = DIRECTION ( 'NONE',  ( -0.000000000000000000, -0.000000000000000000, -1.000000000000000000 ) ) ;
#15360 = CARTESIAN_POINT ( 'NONE',  ( -33.52287095715005449, -23.72747288104469732, -1.053458166803227902 ) ) ;
#15361 = CARTESIAN_POINT ( 'NONE',  ( -19.40224465947428456, -7.824916089261592766, -1.500000000000002220 ) ) ;
#15362 = ORIENTED_EDGE ( 'NONE', *, *, #42796, .T. ) ;
#15363 = AXIS2_PLACEMENT_3D ( 'NONE', #56415, #17834, #50291 ) ;
#15364 = EDGE_CURVE ( 'NONE', #1762, #12512, #56267, .T. ) ;
#15365 = CARTESIAN_POINT ( 'NONE',  ( -67.49333554985891226, -24.66019654487199730, 8.947790411086115725 ) ) ;
#15366 = ORIENTED_EDGE ( 'NONE', *, *, #3849, .T. ) ;
#15367 = CARTESIAN_POINT ( 'NONE',  ( -25.92875734969026524, 5.356774720514425603, 0.7300228001186309656 ) ) ;
#15368 = CARTESIAN_POINT ( 'NONE',  ( 19.38521227897113874, -8.589346653930519437, -1.500000000000002220 ) ) ;
#15369 = VERTEX_POINT ( 'NONE', #35293 ) ;
#15370 = CARTESIAN_POINT ( 'NONE',  ( -50.65952998986089995, -23.85016227208579309, -0.8807180028928346394 ) ) ;
#15371 = CARTESIAN_POINT ( 'NONE',  ( 31.14267748017797999, -4.481735162546526041, -3.047060235321866539 ) ) ;
#15372 = CARTESIAN_POINT ( 'NONE',  ( 1.472770742059883897, 21.73951962378590963, -1.500000000000002220 ) ) ;
#15373 = CARTESIAN_POINT ( 'NONE',  ( -60.58953762381671737, -23.47596703998600276, 11.44779298504227505 ) ) ;
#15374 = CARTESIAN_POINT ( 'NONE',  ( -50.62287095715005592, -24.99156045073392463, 7.747789690856161648 ) ) ;
#15375 = CARTESIAN_POINT ( 'NONE',  ( -79.57012802947382113, -25.20210771990827325, 6.663789735179169504 ) ) ;
#15376 = CARTESIAN_POINT ( 'NONE',  ( -11.22809577558575000, 18.72649003030000259, -1.500000000000002220 ) ) ;
#15377 = CARTESIAN_POINT ( 'NONE',  ( -79.12865799501358310, -25.18586200194109281, 6.785185366648832428 ) ) ;
#15378 = ORIENTED_EDGE ( 'NONE', *, *, #95265, .F. ) ;
#15379 = CARTESIAN_POINT ( 'NONE',  ( -69.62287095715005592, -23.48786465467241058, 11.44779295918254824 ) ) ;
#15380 = FACE_OUTER_BOUND ( 'NONE', #86116, .T. ) ;
#15381 = CARTESIAN_POINT ( 'NONE',  ( 32.15269211224249091, -6.376774720514427841, 3.401810532325274750 ) ) ;
#15382 = VERTEX_POINT ( 'NONE', #82447 ) ;
#15383 = AXIS2_PLACEMENT_3D ( 'NONE', #49960, #27102, #97112 ) ;
#15384 = ADVANCED_FACE ( 'NONE', ( #21040 ), #13428, .F. ) ;
#15385 = ORIENTED_EDGE ( 'NONE', *, *, #65704, .F. ) ;
#15386 = ORIENTED_EDGE ( 'NONE', *, *, #415, .T. ) ;
#15387 = DIRECTION ( 'NONE',  ( 0.8219392559241307517, -0.5637660281018076480, -0.08114015731558694988 ) ) ;
#15388 = B_SPLINE_CURVE_WITH_KNOTS ( 'NONE', 3,
 ( #98496, #83282, #6158, #37111, #98997, #61462 ),
 .UNSPECIFIED., .F., .F.,
 ( 4, 2, 4 ),
 ( 2.780973288783981667E-17, 0.0002696131282151457303, 0.0005392262564302635966 ),
 .UNSPECIFIED. ) ;
#15389 = CARTESIAN_POINT ( 'NONE',  ( -19.34623641613454836, -8.721557147202650739, -1.500000000000002220 ) ) ;
#15390 = B_SPLINE_CURVE_WITH_KNOTS ( 'NONE', 3,
 ( #60512, #66638, #68606, #82328 ),
 .UNSPECIFIED., .F., .F.,
 ( 4, 4 ),
 ( 0.000000000000000000, 0.0008333333333333595161 ),
 .UNSPECIFIED. ) ;
#15391 = CARTESIAN_POINT ( 'NONE',  ( -94.59406255952302445, -23.96119346886881019, -0.6495511937832051386 ) ) ;
#15392 = CARTESIAN_POINT ( 'NONE',  ( -78.99318656846928377, -25.27791721166854089, 6.404754622004839248 ) ) ;
#15393 = DIRECTION ( 'NONE',  ( 0.000000000000000000, 0.000000000000000000, 1.000000000000000000 ) ) ;
#15394 = CARTESIAN_POINT ( 'NONE',  ( 32.01683625711453374, 5.152774720514459617, -11.91548796314834036 ) ) ;
#15395 = CARTESIAN_POINT ( 'NONE',  ( 3.017506814366913481, 19.14668354085002733, -1.500000000000002220 ) ) ;
#15396 = CARTESIAN_POINT ( 'NONE',  ( -69.39739843404061048, -25.28243495002747920, 5.901832878838482621 ) ) ;
#15397 = EDGE_LOOP ( 'NONE', ( #65343, #46106, #26759, #83459 ) ) ;
#15398 = CARTESIAN_POINT ( 'NONE',  ( 14.64286990871793392, 12.78475832571431070, 11.49999999999999645 ) ) ;
#15399 = CARTESIAN_POINT ( 'NONE',  ( -111.6228709571500559, -29.50248528299804818, 1.056150453629043584 ) ) ;
#15400 = EDGE_CURVE ( 'NONE', #96024, #7215, #69542, .T. ) ;
#15401 = EDGE_CURVE ( 'NONE', #65066, #99147, #44650, .T. ) ;
#15402 = FACE_OUTER_BOUND ( 'NONE', #74020, .T. ) ;
#15403 = ORIENTED_EDGE ( 'NONE', *, *, #74440, .T. ) ;
#15404 = DIRECTION ( 'NONE',  ( -0.9951627101165078093, 1.776356839400250267E-15, 0.09824042138329590335 ) ) ;
#15405 = CYLINDRICAL_SURFACE ( 'NONE', #90171, 3.570000000000003837 ) ;
#15406 = B_SPLINE_CURVE_WITH_KNOTS ( 'NONE', 3,
 ( #25455, #15960, #246, #84980, #33576, #10741, #49823, #87352, #48813, #77356, #3142, #100180, #62163, #57434, #72148, #79738, #64554, #95471, #25958, #23065, #34083, #95972, #26471, #11236, #42213, #54054 ),
 .UNSPECIFIED., .F., .F.,
 ( 4, 2, 2, 2, 2, 2, 2, 2, 2, 2, 2, 2, 4 ),
 ( 9.172631729222333727E-06, 0.001697682463320513953, 0.002541937379116161830, 0.003386192294911809925, 0.004230447210707458452, 0.005074702126503106113, 0.006763211958094405771, 0.007607466873890056901, 0.008451721789685704561, 0.01014023162127699815, 0.01098448653707264494, 0.01182874145286829173, 0.01351725128445958879 ),
 .UNSPECIFIED. ) ;
#15407 = DIRECTION ( 'NONE',  ( 1.000000000000000000, 3.773278334444166432E-23, 8.201307841325785021E-29 ) ) ;
#15408 = CARTESIAN_POINT ( 'NONE',  ( -93.58858278818280496, -24.35071581493543391, 9.817618358456016381 ) ) ;
#15409 = CARTESIAN_POINT ( 'NONE',  ( -18.74126595726828626, 5.813943427813767606, -1.500000000000002220 ) ) ;
#15410 = CARTESIAN_POINT ( 'NONE',  ( -117.6228709571500559, -23.73934037231758154, 11.05740245334328264 ) ) ;
#15411 = ORIENTED_EDGE ( 'NONE', *, *, #37567, .F. ) ;
#15412 = VECTOR ( 'NONE', #3852, 1000.000000000000114 ) ;
#15413 = CARTESIAN_POINT ( 'NONE',  ( 14.45009471711328786, 16.04676183837579373, 11.49999999999998934 ) ) ;
#15414 = DIRECTION ( 'NONE',  ( 0.000000000000000000, -1.000000000000000000, 0.000000000000000000 ) ) ;
#15415 = CARTESIAN_POINT ( 'NONE',  ( -40.53341874850772086, -24.63355581998386512, 0.9682620441943814438 ) ) ;
#15416 = CARTESIAN_POINT ( 'NONE',  ( -90.52287095715006160, -23.48786465467241769, 11.44779295918254292 ) ) ;
#15417 = CARTESIAN_POINT ( 'NONE',  ( 22.66633601775066253, -4.223608244049824378, -1.500000000000002220 ) ) ;
#15418 = EDGE_CURVE ( 'NONE', #67116, #69390, #76691, .T. ) ;
#15419 = ADVANCED_FACE ( 'NONE', ( #22524 ), #49098, .T. ) ;
#15420 = PERSON_AND_ORGANIZATION ( #70597, #27821 ) ;
#15421 = FACE_OUTER_BOUND ( 'NONE', #77772, .T. ) ;
#15422 = CARTESIAN_POINT ( 'NONE',  ( 4.453188626415028217, -6.376774720514422512, 21.07953283331298167 ) ) ;
#15423 = CARTESIAN_POINT ( 'NONE',  ( -121.6240024248556040, -24.51419770103157347, 9.386484678747175181 ) ) ;
#15424 = CARTESIAN_POINT ( 'NONE',  ( -100.8191360062217399, -25.05035194608113613, 7.529171757875409376 ) ) ;
#15425 = CARTESIAN_POINT ( 'NONE',  ( 5.641653616409716854, -5.876774720514419847, 20.81030773351227481 ) ) ;
#15426 = CARTESIAN_POINT ( 'NONE',  ( -98.52287095715001897, -23.94994826722565406, -0.6494450866342705853 ) ) ;
#15427 = CARTESIAN_POINT ( 'NONE',  ( -114.5873116467302708, -24.66019654487200441, 8.947790411086106843 ) ) ;
#15428 = CARTESIAN_POINT ( 'NONE',  ( 7.614665684681447111, -18.39110272641453037, 11.49999999999998934 ) ) ;
#15429 = EDGE_CURVE ( 'NONE', #21992, #26463, #54009, .T. ) ;
#15430 = CARTESIAN_POINT ( 'NONE',  ( -24.90875734969025501, -5.965225279485572685, 30.51402280011862089 ) ) ;
#15431 = CARTESIAN_POINT ( 'NONE',  ( 18.78741845327603599, -6.401996767227196905, -1.500000000000002220 ) ) ;
#15432 = CARTESIAN_POINT ( 'NONE',  ( -56.49721973070467129, -24.34968618360933590, 0.1864209137778786995 ) ) ;
#15433 = EDGE_CURVE ( 'NONE', #25116, #19170, #92527, .T. ) ;
#15434 = UNCERTAINTY_MEASURE_WITH_UNIT (LENGTH_MEASURE( 1.000000000000000082E-05 ), #34402, 'distance_accuracy_value', 'NONE');
#15435 = LINE ( 'NONE', #45907, #43490 ) ;
#15436 = CARTESIAN_POINT ( 'NONE',  ( -23.31187512739357715, -0.3587747205144061202, -17.31005501743528541 ) ) ;
#15437 = CARTESIAN_POINT ( 'NONE',  ( -18.06733440434376092, 10.15830956056102963, 11.49999999999999645 ) ) ;
#15438 = CARTESIAN_POINT ( 'NONE',  ( -129.6228709571500417, -29.50250243563736774, 8.947779886222132717 ) ) ;
#15439 = AXIS2_PLACEMENT_3D ( 'NONE', #95960, #81733, #19816 ) ;
#15440 = CARTESIAN_POINT ( 'NONE',  ( -49.68170153635294639, -25.25138720524621760, 5.417898236803782908 ) ) ;
#15441 = CARTESIAN_POINT ( 'NONE',  ( 21.16149768242404861, -8.233860041645145955, 11.49999999999999645 ) ) ;
#15442 = ORIENTED_EDGE ( 'NONE', *, *, #84505, .T. ) ;
#15443 = B_SPLINE_CURVE_WITH_KNOTS ( 'NONE', 3,
 ( #66284, #59157, #43439, #81987, #4375, #36813 ),
 .UNSPECIFIED., .F., .F.,
 ( 4, 2, 4 ),
 ( 1.570755371633915156E-05, 0.001396183895866085801, 0.002776660238015832543 ),
 .UNSPECIFIED. ) ;
#15444 = CARTESIAN_POINT ( 'NONE',  ( -60.62287095715002039, -24.15431212366389602, -0.2830839119429001682 ) ) ;
#15445 = CARTESIAN_POINT ( 'NONE',  ( -74.62287095715009855, -23.73934037231756733, 11.05740245334329153 ) ) ;
#15446 = CARTESIAN_POINT ( 'NONE',  ( -1.055277534996966970, 20.15608268182561247, 11.49999999999998934 ) ) ;
#15447 = DIRECTION ( 'NONE',  ( 0.8219392559241307517, -0.08114015731558921196, 0.5637660281018073150 ) ) ;
#15448 = CIRCLE ( 'NONE', #86735, 19.30000000000000071 ) ;
#15449 = CARTESIAN_POINT ( 'NONE',  ( -45.52287095715006160, -23.48786465467240347, 11.44779295918255002 ) ) ;
#15450 = ORIENTED_EDGE ( 'NONE', *, *, #38383, .F. ) ;
#15451 = AXIS2_PLACEMENT_3D ( 'NONE', #41957, #43452, #20093 ) ;
#15452 = VERTEX_POINT ( 'NONE', #69221 ) ;
#15453 = CARTESIAN_POINT ( 'NONE',  ( 0.1739078616027790736, -5.876774720514415407, 19.75705121608222115 ) ) ;
#15454 = CARTESIAN_POINT ( 'NONE',  ( 15.01570752033863165, -17.30494853738164096, 11.49999999999998934 ) ) ;
#15455 = CARTESIAN_POINT ( 'NONE',  ( -41.82691350321800172, -25.26045596155741890, 3.841969471408021253 ) ) ;
#15456 = CARTESIAN_POINT ( 'NONE',  ( 0.6597851148675514255, -21.60297929554585394, -1.500000000000002220 ) ) ;
#15457 = CARTESIAN_POINT ( 'NONE',  ( 14.76093561896379214, -3.316774720514426456, -27.37148769130089931 ) ) ;
#15458 = CARTESIAN_POINT ( 'NONE',  ( -69.62287095715005592, -29.50250243563736774, 8.947779886222143375 ) ) ;
#15459 = CARTESIAN_POINT ( 'NONE',  ( -2.496121100066326814, 20.73550571027955769, 11.49999999999999645 ) ) ;
#15460 = VERTEX_POINT ( 'NONE', #62619 ) ;
#15461 = CARTESIAN_POINT ( 'NONE',  ( -124.6246529919008594, -24.15543982623907127, -0.2315651400026562945 ) ) ;
#15462 = CARTESIAN_POINT ( 'NONE',  ( -16.14483305390557888, 14.99321182834783528, -1.500000000000002220 ) ) ;
#15463 = DIRECTION ( 'NONE',  ( 0.000000000000000000, 0.000000000000000000, -1.000000000000000000 ) ) ;
#15464 = CARTESIAN_POINT ( 'NONE',  ( -65.62287095715008434, -24.62285846362216191, 9.038163152653529764 ) ) ;
#15466 = ORIENTED_EDGE ( 'NONE', *, *, #26545, .T. ) ;
#15465 = EDGE_CURVE ( 'NONE', #47759, #5356, #93540, .T. ) ;
#15467 = DIRECTION ( 'NONE',  ( 0.8246584009594635223, 0.5656310827093757876, 0.000000000000000000 ) ) ;
#15468 = CARTESIAN_POINT ( 'NONE',  ( 6.600000000000001421, 0.000000000000000000, 0.000000000000000000 ) ) ;
#15469 = ORIENTED_EDGE ( 'NONE', *, *, #80758, .F. ) ;
#15470 = CARTESIAN_POINT ( 'NONE',  ( -65.05438548721848235, -5.356774720514425603, 0.7300228001186309656 ) ) ;
#15471 = ORIENTED_EDGE ( 'NONE', *, *, #74122, .T. ) ;
#15472 = ORIENTED_EDGE ( 'NONE', *, *, #32860, .T. ) ;
#15473 = CARTESIAN_POINT ( 'NONE',  ( -41.62287095715006302, -24.64965695001467694, 8.947790433994187609 ) ) ;
#15474 = CARTESIAN_POINT ( 'NONE',  ( -101.7453191491394477, -25.27404852088134746, 3.852396047414954339 ) ) ;
#15475 = CARTESIAN_POINT ( 'NONE',  ( -4.152941208099351300, -5.876774720514415407, 20.35309744218305639 ) ) ;
#15476 = CARTESIAN_POINT ( 'NONE',  ( -20.02755620033356010, -4.236777897013602079, -1.500000000000002220 ) ) ;
#15477 = ORIENTED_EDGE ( 'NONE', *, *, #50593, .F. ) ;
#15478 = CARTESIAN_POINT ( 'NONE',  ( -110.5228709571500616, -24.99156044556120548, 7.747789690856173195 ) ) ;
#15479 = DIRECTION ( 'NONE',  ( 0.000000000000000000, -1.000000000000000000, 0.000000000000000000 ) ) ;
#15480 = CARTESIAN_POINT ( 'NONE',  ( -19.77875734969026311, -3.316774720514426456, 29.49402280011862487 ) ) ;
#15481 = CARTESIAN_POINT ( 'NONE',  ( 18.42719714020066846, 12.55551944762973626, -1.500000000000002220 ) ) ;
#15482 = CARTESIAN_POINT ( 'NONE',  ( -4.141166922167975883, -6.376774720514420736, 20.63520656483649063 ) ) ;
#15483 = CARTESIAN_POINT ( 'NONE',  ( -91.52287095715006160, -23.47593901973090524, -1.443836447538996648 ) ) ;
#15484 = VERTEX_POINT ( 'NONE', #24035 ) ;
#15485 = CARTESIAN_POINT ( 'NONE',  ( -29.81175120719462157, -25.24633111994858581, 4.942810988825437235 ) ) ;
#15486 = CARTESIAN_POINT ( 'NONE',  ( -39.52287095715004739, -24.51387760970725438, 9.387446482453428942 ) ) ;
#15487 = CARTESIAN_POINT ( 'NONE',  ( -17.17656601037699104, 11.78060583124977256, 11.49999999999998934 ) ) ;
#15488 = EDGE_LOOP ( 'NONE', ( #67311, #29761, #60592, #62037 ) ) ;
#15490 = ORIENTED_EDGE ( 'NONE', *, *, #64608, .F. ) ;
#15489 = DIRECTION ( 'NONE',  ( 5.095998543435641288E-17, 0.6401843996644797086, -0.7682212795973759611 ) ) ;
#15491 = EDGE_CURVE ( 'NONE', #75557, #1512, #17415, .T. ) ;
#15492 = CARTESIAN_POINT ( 'NONE',  ( -51.45055690290539019, -25.12217740856155146, 6.541367195127278045 ) ) ;
#15493 = ORIENTED_EDGE ( 'NONE', *, *, #57367, .F. ) ;
#15494 = DIRECTION ( 'NONE',  ( 0.000000000000000000, -2.173523156925979552E-06, 0.9999999999976378895 ) ) ;
#15495 = CARTESIAN_POINT ( 'NONE',  ( -121.5228709571500616, -23.48786465467241769, 11.44779295918253759 ) ) ;
#15496 = CARTESIAN_POINT ( 'NONE',  ( 8.720390671778812219, -3.316774720514306996, -27.07197491306147086 ) ) ;
#15497 = DIRECTION ( 'NONE',  ( -3.773278334453079618E-23, 0.9999999999976377785, 2.173523156925979975E-06 ) ) ;
#15498 = CARTESIAN_POINT ( 'NONE',  ( 29.73860345376319003, -4.772774720514425972, -8.849814207987163783 ) ) ;
#15499 = DIRECTION ( 'NONE',  ( -3.773278334453079618E-23, 0.9999999999976377785, 2.173523156925979975E-06 ) ) ;
#15501 = ORIENTED_EDGE ( 'NONE', *, *, #33860, .F. ) ;
#15500 = CARTESIAN_POINT ( 'NONE',  ( -5.994446910899359438, -21.39327697068355505, 11.49999999999999645 ) ) ;
#15502 = CARTESIAN_POINT ( 'NONE',  ( -38.62287095715005592, -24.34917612406837506, 0.1852690917426539075 ) ) ;
#15503 = ORIENTED_EDGE ( 'NONE', *, *, #52988, .T. ) ;
#15504 = CARTESIAN_POINT ( 'NONE',  ( 14.74224262856723833, 17.19160420931263999, 11.49999999999998934 ) ) ;
#15505 = ADVANCED_FACE ( 'NONE', ( #78317 ), #8823, .F. ) ;
#15506 = ADVANCED_FACE ( 'NONE', ( #94051 ), #70720, .T. ) ;
#15507 = B_SPLINE_CURVE_WITH_KNOTS ( 'NONE', 3,
 ( #8826, #32153, #1220, #16931 ),
 .UNSPECIFIED., .F., .F.,
 ( 4, 4 ),
 ( 0.000000000000000000, 9.999999999996123101E-05 ),
 .UNSPECIFIED. ) ;
#15509 = ORIENTED_EDGE ( 'NONE', *, *, #43023, .T. ) ;
#15508 = DIRECTION ( 'NONE',  ( -0.000000000000000000, 0.000000000000000000, 1.000000000000000000 ) ) ;
#15510 = ORIENTED_EDGE ( 'NONE', *, *, #95148, .F. ) ;
#15511 = EDGE_CURVE ( 'NONE', #45688, #54341, #68280, .T. ) ;
#15512 = CYLINDRICAL_SURFACE ( 'NONE', #62888, 1.836000000000000743 ) ;
#15513 = VECTOR ( 'NONE', #60789, 1000.000000000000114 ) ;
#15514 = CARTESIAN_POINT ( 'NONE',  ( -19.48533387766964964, -5.011242947278518045, -1.500000000000002220 ) ) ;
#15515 = CARTESIAN_POINT ( 'NONE',  ( 22.81105451610979173, -6.475225279485573360, -16.21691820600746681 ) ) ;
#15516 = EDGE_LOOP ( 'NONE', ( #66128, #10753, #95256, #28647, #57943, #83759, #23966, #81877, #84498, #18633, #17921, #98855 ) ) ;
#15517 = AXIS2_PLACEMENT_3D ( 'NONE', #23231, #16629, #54217 ) ;
#15518 = LINE ( 'NONE', #39865, #43906 ) ;
#15519 = CARTESIAN_POINT ( 'NONE',  ( 0.3464652362752086434, -22.36268665536068667, -1.500000000000002220 ) ) ;
#15520 = EDGE_CURVE ( 'NONE', #85004, #54879, #33152, .T. ) ;
#15521 = CIRCLE ( 'NONE', #46313, 18.50000000000000000 ) ;
#15522 = VERTEX_POINT ( 'NONE', #58016 ) ;
#15523 = ORIENTED_EDGE ( 'NONE', *, *, #17717, .F. ) ;
#15524 = CARTESIAN_POINT ( 'NONE',  ( 26.73860345374794178, -1.477225279485574028, 19.84760796525321780 ) ) ;
#15525 = PLANE ( 'NONE',  #58900 ) ;
#15526 = CARTESIAN_POINT ( 'NONE',  ( -80.44898789460346222, -25.29552500624826195, 4.507972869655594295 ) ) ;
#15527 = CARTESIAN_POINT ( 'NONE',  ( 32.19706240494739546, 5.152774720514445406, -11.87117847608345933 ) ) ;
#15528 = AXIS2_PLACEMENT_3D ( 'NONE', #2645, #80763, #56938 ) ;
#15529 = FACE_BOUND ( 'NONE', #89365, .T. ) ;
#15530 = CARTESIAN_POINT ( 'NONE',  ( 18.72186718581493636, -5.619560887262019300, -1.500000000000002220 ) ) ;
#15531 = DIRECTION ( 'NONE',  ( -0.9978940991575085961, 0.000000000000000000, -0.06486421869277853025 ) ) ;
#15532 = CARTESIAN_POINT ( 'NONE',  ( 13.13055478438326773, -17.03443908202477886, 11.49999999999998934 ) ) ;
#15533 = CARTESIAN_POINT ( 'NONE',  ( -128.6241754002568882, -23.73766607897672287, -1.055555164236423149 ) ) ;
#15534 = LINE ( 'NONE', #32267, #90193 ) ;
#15535 = DIRECTION ( 'NONE',  ( -1.000000000000000000, 0.000000000000000000, -0.000000000000000000 ) ) ;
#15536 = CARTESIAN_POINT ( 'NONE',  ( 32.54628039735602130, -5.044004387208919304, -11.78547710168594165 ) ) ;
#15537 = CARTESIAN_POINT ( 'NONE',  ( 20.53691900564983186, 10.01969956684014207, -1.500000000000002220 ) ) ;
#15538 = EDGE_CURVE ( 'NONE', #63330, #81513, #34666, .T. ) ;
#15539 = ADVANCED_FACE ( 'NONE', ( #79823 ), #24730, .T. ) ;
#15540 = B_SPLINE_CURVE_WITH_KNOTS ( 'NONE', 3,
 ( #14923, #68731, #85948, #61631, #46386, #62123, #93045, #24037, #69731, #55010, #62623, #93542, #209, #99650 ),
 .UNSPECIFIED., .F., .F.,
 ( 4, 2, 2, 2, 2, 2, 4 ),
 ( 1.734723475976807094E-18, 0.0001855958525969266134, 0.0003711917051938514920, 0.0007423834103877197891, 0.001113575115581588032, 0.001299170968178541994, 0.001484766820775495957 ),
 .UNSPECIFIED. ) ;
#15541 = APPROVAL_STATUS ( 'not_yet_approved' ) ;
#15542 = CARTESIAN_POINT ( 'NONE',  ( -96.60008899554439665, -23.48786465467241058, 11.44779295918254469 ) ) ;
#15543 = CARTESIAN_POINT ( 'NONE',  ( -70.93828905505007754, -25.30664601920957324, 5.476242254610935944 ) ) ;
#15544 = CARTESIAN_POINT ( 'NONE',  ( 5.980626343040887249, -19.09133569553460319, 11.49999999999999645 ) ) ;
#15545 = CARTESIAN_POINT ( 'NONE',  ( -78.99596516450635875, -25.31594537816884127, 5.526333899285822859 ) ) ;
#15546 = LINE ( 'NONE', #23654, #40395 ) ;
#15547 = CARTESIAN_POINT ( 'NONE',  ( 27.86270917940689174, 0.3587747205144265483, 29.49402280011862487 ) ) ;
#15548 = FACE_OUTER_BOUND ( 'NONE', #99857, .T. ) ;
#15549 = EDGE_LOOP ( 'NONE', ( #33760, #5404, #46240, #1520 ) ) ;
#15550 = CARTESIAN_POINT ( 'NONE',  ( 27.53860345374771867, 500000.0000000000582, -9.482392034746240483 ) ) ;
#15551 = CARTESIAN_POINT ( 'NONE',  ( -92.62287095715005592, -23.48783264082479150, -1.443836473390063713 ) ) ;
#15552 = EDGE_CURVE ( 'NONE', #97111, #1645, #27129, .T. ) ;
#15553 = CARTESIAN_POINT ( 'NONE',  ( -18.42844947050907578, 11.51566461966115540, 11.49999999999998934 ) ) ;
#15554 = CARTESIAN_POINT ( 'NONE',  ( -56.62287095715005592, -23.48786465467241413, 11.44779295918254824 ) ) ;
#15555 = CARTESIAN_POINT ( 'NONE',  ( -13.18904525526904692, 14.46673508071025971, -1.500000000000002220 ) ) ;
#15556 = CARTESIAN_POINT ( 'NONE',  ( -85.52287095715006160, -24.92604778743017491, 8.074972756849357225 ) ) ;
#15557 = EDGE_CURVE ( 'NONE', #72155, #65722, #88955, .T. ) ;
#15558 = EDGE_CURVE ( 'NONE', #56230, #82393, #25037, .T. ) ;
#15559 = CARTESIAN_POINT ( 'NONE',  ( -41.46611000704998418, -25.27828342519987359, 4.188173683033348915 ) ) ;
#15560 = CONTEXT_DEPENDENT_SHAPE_REPRESENTATION ( #51150, #25498 ) ;
#15561 = CARTESIAN_POINT ( 'NONE',  ( -38.58953762381672448, -23.47596703998600276, 11.44779298504227505 ) ) ;
#15562 = LINE ( 'NONE', #91190, #8606 ) ;
#15563 = CARTESIAN_POINT ( 'NONE',  ( -1.452656003914881477, -20.50939586048694352, 11.49999999999999645 ) ) ;
#15564 = CARTESIAN_POINT ( 'NONE',  ( 22.81105451610979173, -2.682774720540237468, -16.21691820600746681 ) ) ;
#15565 = CARTESIAN_POINT ( 'NONE',  ( -6.660000000000001030, 2.939152317953647106E-16, -2.399999999999999911 ) ) ;
#15566 = ADVANCED_FACE ( 'NONE', ( #80331 ), #72732, .F. ) ;
#15567 = ORIENTED_EDGE ( 'NONE', *, *, #11464, .T. ) ;
#15568 = CARTESIAN_POINT ( 'NONE',  ( -100.5167721066480908, -25.31296450146793120, 4.733455254540654522 ) ) ;
#15569 = FACE_OUTER_BOUND ( 'NONE', #84748, .T. ) ;
#15570 = CARTESIAN_POINT ( 'NONE',  ( -125.5200004750861638, -24.63419186844610920, 9.035850630976920428 ) ) ;
#15571 = CARTESIAN_POINT ( 'NONE',  ( -85.62287095715004170, -24.52232992886362695, 0.6492154411906178035 ) ) ;
#15572 = CARTESIAN_POINT ( 'NONE',  ( -25.53215482860445107, -24.93062936653361206, 5.039154709304365376 ) ) ;
#15573 = CARTESIAN_POINT ( 'NONE',  ( -68.62287095715005592, -23.48783264082478439, -1.443836473390067265 ) ) ;
#15574 = VECTOR ( 'NONE', #43530, 1000.000000000000114 ) ;
#15575 = CARTESIAN_POINT ( 'NONE',  ( 11.75533340255842596, 19.88161105567325038, 11.49999999999999645 ) ) ;
#15576 = CARTESIAN_POINT ( 'NONE',  ( -12.44792101662413408, -19.12764231104124946, 11.49999999999998934 ) ) ;
#15577 = CARTESIAN_POINT ( 'NONE',  ( -74.55900427510123052, -23.73766607897670511, -1.055555164236458898 ) ) ;
#15578 = CARTESIAN_POINT ( 'NONE',  ( -88.52287095715001897, -23.73907113216989373, -1.053371485793251017 ) ) ;
#15579 = CARTESIAN_POINT ( 'NONE',  ( -59.27315846036497504, -25.26302882147717099, 3.719515914026431336 ) ) ;
#15580 = CARTESIAN_POINT ( 'NONE',  ( 14.18375884139645215, 17.39688726336347102, 11.49999999999999645 ) ) ;
#15581 = VERTEX_POINT ( 'NONE', #11816 ) ;
#15582 = DIRECTION ( 'NONE',  ( 0.7512896232465892110, 0.000000000000000000, 0.6599726524652350657 ) ) ;
#15583 = CARTESIAN_POINT ( 'NONE',  ( -43.52287095715007581, -23.95044443724991723, 10.65354141964649415 ) ) ;
#15584 = CARTESIAN_POINT ( 'NONE',  ( 18.54397492014093984, 11.73900455106235086, 11.49999999999998934 ) ) ;
#15585 = FACE_OUTER_BOUND ( 'NONE', #10654, .T. ) ;
#15586 = CIRCLE ( 'NONE', #26904, 253.2618649670780826 ) ;
#15587 = CARTESIAN_POINT ( 'NONE',  ( -87.58839707165199684, -24.35071581493543391, 9.817618358456025263 ) ) ;
#15588 = PLANE ( 'NONE',  #1699 ) ;
#15589 = CARTESIAN_POINT ( 'NONE',  ( -78.51706572721168698, -23.73766607897670511, -1.055555164236459342 ) ) ;
#15590 = CARTESIAN_POINT ( 'NONE',  ( -97.22287095715006444, -23.47593901973090169, -1.443836447538996870 ) ) ;
#15591 = ORIENTED_EDGE ( 'NONE', *, *, #91115, .F. ) ;
#15592 = AXIS2_PLACEMENT_3D ( 'NONE', #78377, #8379, #39826 ) ;
#15593 = CARTESIAN_POINT ( 'NONE',  ( 8.813945691637787405, 18.49579627399651471, 11.49999999999998934 ) ) ;
#15594 = ORIENTED_EDGE ( 'NONE', *, *, #87958, .T. ) ;
#15595 = VECTOR ( 'NONE', #35490, 1000.000000000000000 ) ;
#15596 = ORIENTED_EDGE ( 'NONE', *, *, #77312, .F. ) ;
#15597 = ORIENTED_EDGE ( 'NONE', *, *, #21732, .F. ) ;
#15598 = EDGE_LOOP ( 'NONE', ( #28215, #97985, #581, #4779 ) ) ;
#15599 = CARTESIAN_POINT ( 'NONE',  ( 18.43541038833219758, -13.85303862407246811, 11.49999999999998934 ) ) ;
#15600 = CARTESIAN_POINT ( 'NONE',  ( -72.62287095715005592, -29.50248528299804818, 1.056150453629036701 ) ) ;
#15601 = CARTESIAN_POINT ( 'NONE',  ( 9.670762957215185196, 17.83519281925787325, -1.500000000000002220 ) ) ;
#15602 = AXIS2_PLACEMENT_3D ( 'NONE', #3212, #88433, #34153 ) ;
#15603 = VERTEX_POINT ( 'NONE', #20914 ) ;
#15604 = CARTESIAN_POINT ( 'NONE',  ( -48.52287095715006160, -24.50321055353804667, 9.387540953477520489 ) ) ;
#15605 = CARTESIAN_POINT ( 'NONE',  ( -72.52287095715007581, -24.64898659630367916, 1.056161002820824368 ) ) ;
#15606 = VECTOR ( 'NONE', #38289, 1000.000000000000114 ) ;
#15607 = FACE_OUTER_BOUND ( 'NONE', #91420, .T. ) ;
#15608 = CARTESIAN_POINT ( 'NONE',  ( -70.53858138727555627, -24.73486907724917572, 1.287355809206963908 ) ) ;
#15610 = EDGE_LOOP ( 'NONE', ( #79215, #80322, #81101, #85485 ) ) ;
#15609 = CARTESIAN_POINT ( 'NONE',  ( 19.19993882694861753, 9.668096177433461946, 11.49999999999999645 ) ) ;
#15611 = CARTESIAN_POINT ( 'NONE',  ( -75.62528691939071734, -24.92564183028979130, 1.928384488918256645 ) ) ;
#15612 = CARTESIAN_POINT ( 'NONE',  ( -61.63716569185557148, -24.15620529776628089, 10.23563542870660825 ) ) ;
#15613 = ORIENTED_EDGE ( 'NONE', *, *, #64449, .F. ) ;
#15614 = CARTESIAN_POINT ( 'NONE',  ( 19.40724743217988291, -7.346346906864608783, 11.49999999999998934 ) ) ;
#15615 = VERTEX_POINT ( 'NONE', #60510 ) ;
#15617 = VERTEX_POINT ( 'NONE', #66137 ) ;
#15616 = CARTESIAN_POINT ( 'NONE',  ( -32.62287095715004881, -29.50248528299804818, 1.056150453629029817 ) ) ;
#15618 = EDGE_CURVE ( 'NONE', #91541, #96024, #36834, .T. ) ;
#15619 = CARTESIAN_POINT ( 'NONE',  ( -53.01255352321339842, -4.772774720514425972, 35.59556822165056644 ) ) ;
#15620 = CARTESIAN_POINT ( 'NONE',  ( -48.52287095715004739, -23.96127896942158486, -0.6493128930934110032 ) ) ;
#15621 = ORIENTED_EDGE ( 'NONE', *, *, #99072, .F. ) ;
#15622 = ORIENTED_EDGE ( 'NONE', *, *, #44619, .T. ) ;
#15623 = ADVANCED_FACE ( 'NONE', ( #35665 ), #37149, .F. ) ;
#15624 = CARTESIAN_POINT ( 'NONE',  ( 3.825381322105384285, -5.876774720514399419, 18.16071977647550995 ) ) ;
#15625 = CARTESIAN_POINT ( 'NONE',  ( 33.00535138976610483, -5.965225279485572685, -12.97242311383961422 ) ) ;
#15626 = CARTESIAN_POINT ( 'NONE',  ( -65.64505387063937292, -24.15503026093916006, -0.2815557561904380446 ) ) ;
#15627 = CARTESIAN_POINT ( 'NONE',  ( 14.26656746985186608, 16.74056184347216458, 11.49999999999999645 ) ) ;
#15628 = EDGE_CURVE ( 'NONE', #64178, #33243, #82820, .T. ) ;
#15629 = CARTESIAN_POINT ( 'NONE',  ( -89.55151923034836159, -24.15620529776628445, 10.23563542870660115 ) ) ;
#15630 = CARTESIAN_POINT ( 'NONE',  ( 15.50834587592193259, -16.38432980155966590, -1.500000000000002220 ) ) ;
#15631 = B_SPLINE_CURVE_WITH_KNOTS ( 'NONE', 3,
 ( #79346, #86463, #47912, #9839 ),
 .UNSPECIFIED., .F., .F.,
 ( 4, 4 ),
 ( 2.775557561562891351E-17, 9.999999999994735322E-05 ),
 .UNSPECIFIED. ) ;
#15632 = VECTOR ( 'NONE', #27423, 1000.000000000000000 ) ;
#15633 = EDGE_CURVE ( 'NONE', #58927, #25949, #59075, .T. ) ;
#15634 = CARTESIAN_POINT ( 'NONE',  ( 11.23609023086081038, -17.74952302366565604, -1.500000000000002220 ) ) ;
#15635 = ADVANCED_FACE ( 'NONE', ( #75207 ), #44774, .F. ) ;
#15636 = DIRECTION ( 'NONE',  ( -3.773278334453079030E-23, 0.9999999999976377785, 2.173523156925979128E-06 ) ) ;
#15637 = ORIENTED_EDGE ( 'NONE', *, *, #72612, .F. ) ;
#15638 = ORIENTED_EDGE ( 'NONE', *, *, #73953, .T. ) ;
#15639 = EDGE_CURVE ( 'NONE', #95598, #43602, #5699, .T. ) ;
#15640 = CARTESIAN_POINT ( 'NONE',  ( -66.49289369796184701, -24.65952944569304250, 1.056160979905692798 ) ) ;
#15641 = CARTESIAN_POINT ( 'NONE',  ( -21.28347836979250118, 3.227085873532868021, -1.500000000000002220 ) ) ;
#15642 = CARTESIAN_POINT ( 'NONE',  ( -100.5228709571500616, -23.47596703998600631, 11.44779298504228215 ) ) ;
#15643 = ORIENTED_EDGE ( 'NONE', *, *, #83583, .T. ) ;
#15644 = CARTESIAN_POINT ( 'NONE',  ( -0.2625952501129409367, 21.13516572482953748, 11.49999999999998934 ) ) ;
#15645 = DIRECTION ( 'NONE',  ( -0.000000000000000000, 1.000000000000000000, -0.000000000000000000 ) ) ;
#15646 = CARTESIAN_POINT ( 'NONE',  ( -51.44452858623887437, -25.26041045480337388, 7.233629632149025213 ) ) ;
#15647 = CARTESIAN_POINT ( 'NONE',  ( -121.6240037161720409, -24.51314013834316441, 0.6176544820404217262 ) ) ;
#15648 = CARTESIAN_POINT ( 'NONE',  ( -79.62287095715005592, -24.64898659630528854, 1.056161002820826145 ) ) ;
#15649 = CARTESIAN_POINT ( 'NONE',  ( -80.92287095715010992, -23.47593901973090524, -1.443836447538997536 ) ) ;
#15650 = CARTESIAN_POINT ( 'NONE',  ( -21.91774099701738621, 3.392077650570975766, -1.500000000000002220 ) ) ;
#15651 = DIRECTION ( 'NONE',  ( -1.000000000000000000, 0.000000000000000000, 2.501730345825856573E-15 ) ) ;
#15652 = EDGE_CURVE ( 'NONE', #79759, #25743, #519, .T. ) ;
#15653 = ORIENTED_EDGE ( 'NONE', *, *, #53162, .F. ) ;
#15654 = CARTESIAN_POINT ( 'NONE',  ( -20.27875734969026311, 7.743225279485574042, 24.00402280011862288 ) ) ;
#15655 = CARTESIAN_POINT ( 'NONE',  ( -37.57003923573987691, -23.48783264082477729, -1.443836473390075703 ) ) ;
#15656 = CARTESIAN_POINT ( 'NONE',  ( -126.5562100404590211, -23.73766607897670511, -1.055555164236450238 ) ) ;
#15657 = VECTOR ( 'NONE', #59372, 1000.000000000000000 ) ;
#15658 = DIRECTION ( 'NONE',  ( 0.000000000000000000, 0.000000000000000000, -1.000000000000000000 ) ) ;
#15659 = DIRECTION ( 'NONE',  ( 0.000000000000000000, 0.000000000000000000, 1.000000000000000000 ) ) ;
#15660 = ADVANCED_FACE ( 'NONE', ( #82817 ), #64502, .T. ) ;
#15661 = CARTESIAN_POINT ( 'NONE',  ( 18.36381783059253081, 6.383776564742674964, -1.500000000000002220 ) ) ;
#15662 = CARTESIAN_POINT ( 'NONE',  ( -6.079122355442096115, 20.50309271558274915, 11.49999999999998934 ) ) ;
#15663 = CARTESIAN_POINT ( 'NONE',  ( -64.52287095715006160, -24.65952944569304606, 1.056160979905695463 ) ) ;
#15664 = CARTESIAN_POINT ( 'NONE',  ( 8.160000000000000142, -7.443174476472325551, 8.148664233019720982 ) ) ;
#15665 = CARTESIAN_POINT ( 'NONE',  ( -123.5228709571500616, -24.64898659630368627, 1.056161002820833028 ) ) ;
#15666 = CARTESIAN_POINT ( 'NONE',  ( -101.1965263674405691, -25.27360055340518841, 3.665446404013341208 ) ) ;
#15667 = CARTESIAN_POINT ( 'NONE',  ( 12.08046422559826816, 19.21373320108137861, -1.500000000000002220 ) ) ;
#15668 = EDGE_CURVE ( 'NONE', #99093, #83403, #46536, .T. ) ;
#15669 = VECTOR ( 'NONE', #81231, 1000.000000000000114 ) ;
#15670 = AXIS2_PLACEMENT_3D ( 'NONE', #51448, #38198, #53448 ) ;
#15671 = CARTESIAN_POINT ( 'NONE',  ( 17.51792015816173986, 0.3587747205144265483, 29.01255224319336889 ) ) ;
#15672 = CARTESIAN_POINT ( 'NONE',  ( -127.6228709571500559, -23.96127896941633750, -0.6493128931037727147 ) ) ;
#15673 = CARTESIAN_POINT ( 'NONE',  ( 4.300141163375406528, 19.41444791797076874, 11.49999999999999645 ) ) ;
#15674 = CARTESIAN_POINT ( 'NONE',  ( -123.5905687669561530, -23.96169478059714919, 10.65365249895717348 ) ) ;
#15675 = AXIS2_PLACEMENT_3D ( 'NONE', #5406, #99236, #99724 ) ;
#15676 = CARTESIAN_POINT ( 'NONE',  ( -60.25625423781919920, -25.20074414427590170, 3.409327697718777195 ) ) ;
#15677 = EDGE_LOOP ( 'NONE', ( #45867, #2898, #2902, #72185 ) ) ;
#15678 = CARTESIAN_POINT ( 'NONE',  ( -40.62287095715005592, -23.84081130438200091, 10.88220057463248658 ) ) ;
#15679 = CARTESIAN_POINT ( 'NONE',  ( -24.90875734969025501, 5.965225279485572685, 30.51402280011862089 ) ) ;
#15680 = CARTESIAN_POINT ( 'NONE',  ( 14.02745725694894574, 2.682774720514426559, -27.25215004931931517 ) ) ;
#15681 = CARTESIAN_POINT ( 'NONE',  ( 20.17453868081960167, 7.849935799312063089, -1.500000000000002220 ) ) ;
#15682 = LINE ( 'NONE', #92799, #18840 ) ;
#15683 = CARTESIAN_POINT ( 'NONE',  ( -8.724563080612403709, -17.33930400145671413, -1.500000000000002220 ) ) ;
#15684 = FACE_OUTER_BOUND ( 'NONE', #44579, .T. ) ;
#15685 = CARTESIAN_POINT ( 'NONE',  ( -55.54036855594094391, -24.52399227489126687, 9.353111116836526406 ) ) ;
#15686 = EDGE_CURVE ( 'NONE', #52813, #6577, #69607, .T. ) ;
#15687 = CARTESIAN_POINT ( 'NONE',  ( 16.46483878678964174, 11.07114234313464252, 11.49999999999998934 ) ) ;
#15688 = ORIENTED_EDGE ( 'NONE', *, *, #62159, .F. ) ;
#15689 = CARTESIAN_POINT ( 'NONE',  ( -6.898722100468609675, -19.10483383855023476, 11.49999999999999645 ) ) ;
#15690 = CARTESIAN_POINT ( 'NONE',  ( -80.51503367831445246, -23.85016227208580730, -0.8807180028928341953 ) ) ;
#15691 = EDGE_CURVE ( 'NONE', #92378, #47484, #91424, .T. ) ;
#15692 = DIRECTION ( 'NONE',  ( -3.773278334444167608E-23, 1.000000000000000000, 0.000000000000000000 ) ) ;
#15693 = ORIENTED_EDGE ( 'NONE', *, *, #62794, .T. ) ;
#15694 = LINE ( 'NONE', #8085, #81568 ) ;
#15695 = FACE_OUTER_BOUND ( 'NONE', #92354, .T. ) ;
#15696 = CARTESIAN_POINT ( 'NONE',  ( -49.08163135806235289, -25.31601931085639023, 5.465038190089022585 ) ) ;
#15697 = CARTESIAN_POINT ( 'NONE',  ( -40.57354567782093824, -23.48786465467240347, 11.44779295918255180 ) ) ;
#15698 = CARTESIAN_POINT ( 'NONE',  ( -0.9540731552372990754, -5.876774720514411854, 19.74568812963596542 ) ) ;
#15699 = CARTESIAN_POINT ( 'NONE',  ( 18.81927703376926786, -7.057843677351100631, -1.500000000000002220 ) ) ;
#15700 = EDGE_CURVE ( 'NONE', #89719, #67804, #38643, .T. ) ;
#15701 = FACE_OUTER_BOUND ( 'NONE', #37836, .T. ) ;
#15702 = EDGE_LOOP ( 'NONE', ( #18519, #39014, #47204, #35876 ) ) ;
#15703 = CARTESIAN_POINT ( 'NONE',  ( -91.62287095715007013, -24.35013146730204525, 9.818937971375104823 ) ) ;
#15704 = VECTOR ( 'NONE', #39825, 1000.000000000000000 ) ;
#15705 = CARTESIAN_POINT ( 'NONE',  ( -16.32851894532483783, 16.03542138455653898, 11.49999999999999645 ) ) ;
#15706 = CARTESIAN_POINT ( 'NONE',  ( 1.118074629359579797, -22.68859683979520980, 11.49999999999998934 ) ) ;
#15707 = ORIENTED_EDGE ( 'NONE', *, *, #31783, .F. ) ;
#15708 = CARTESIAN_POINT ( 'NONE',  ( 31.31283134548411340, -1.477225279485574028, -10.20862453625735711 ) ) ;
#15709 = CARTESIAN_POINT ( 'NONE',  ( -126.5228709571500616, -24.66019654487200441, 8.947790411086108620 ) ) ;
#15710 = CARTESIAN_POINT ( 'NONE',  ( -0.02075734969026423599, 5.965225279485572685, -28.54397719988136828 ) ) ;
#15711 = FACE_OUTER_BOUND ( 'NONE', #3535, .T. ) ;
#15712 = FACE_OUTER_BOUND ( 'NONE', #90195, .T. ) ;
#15713 = CARTESIAN_POINT ( 'NONE',  ( -111.5228709571500616, -23.47596703998600631, 11.44779298504228038 ) ) ;
#15714 = ORIENTED_EDGE ( 'NONE', *, *, #33430, .T. ) ;
#15715 = CARTESIAN_POINT ( 'NONE',  ( 17.64890103348723116, 10.21726211432410203, -1.500000000000002220 ) ) ;
#15716 = ORIENTED_EDGE ( 'NONE', *, *, #100039, .T. ) ;
#15717 = CARTESIAN_POINT ( 'NONE',  ( -22.04953120734539240, -6.464106996104416858, -1.500000000000002220 ) ) ;
#15718 = CARTESIAN_POINT ( 'NONE',  ( -54.61289481623843756, -23.48786465467240347, 11.44779295918255357 ) ) ;
#15719 = ORIENTED_EDGE ( 'NONE', *, *, #61370, .T. ) ;
#15720 = CARTESIAN_POINT ( 'NONE',  ( -101.4686356869278967, -25.21739261586568048, 6.465307737249717412 ) ) ;
#15721 = VECTOR ( 'NONE', #80677, 1000.000000000000114 ) ;
#15722 = CARTESIAN_POINT ( 'NONE',  ( -81.48149462243461016, -25.24685308744633261, 6.293942982122115559 ) ) ;
#15723 = B_SPLINE_CURVE_WITH_KNOTS ( 'NONE', 3,
 ( #50011, #3343, #72343, #79435 ),
 .UNSPECIFIED., .F., .F.,
 ( 4, 4 ),
 ( 0.000000000000000000, 9.999999999998206125E-05 ),
 .UNSPECIFIED. ) ;
#15724 = CARTESIAN_POINT ( 'NONE',  ( 22.81105451610979173, 1.682774720514426114, -18.46691820600746681 ) ) ;
#15726 = ORIENTED_EDGE ( 'NONE', *, *, #93007, .F. ) ;
#15725 = CARTESIAN_POINT ( 'NONE',  ( 9.714863677370791706, 19.00186346016302608, 11.49999999999999645 ) ) ;
#15727 = ORIENTED_EDGE ( 'NONE', *, *, #15745, .T. ) ;
#15728 = CARTESIAN_POINT ( 'NONE',  ( 7.537409830304743430, 20.87355781386819942, -1.500000000000002220 ) ) ;
#15729 = CARTESIAN_POINT ( 'NONE',  ( 13.18972694569024640, 15.87703813876158598, 11.49999999999998934 ) ) ;
#15730 = AXIS2_PLACEMENT_3D ( 'NONE', #49301, #80230, #10726 ) ;
#15731 = ORIENTED_EDGE ( 'NONE', *, *, #12205, .F. ) ;
#15732 = ORIENTED_EDGE ( 'NONE', *, *, #88594, .F. ) ;
#15733 = CARTESIAN_POINT ( 'NONE',  ( -4.977357939505175466, -6.376774720514410077, 19.14913681718893557 ) ) ;
#15734 = CARTESIAN_POINT ( 'NONE',  ( -71.72373620137601336, -25.31392322340849432, 5.203679841770401104 ) ) ;
#15735 = ORIENTED_EDGE ( 'NONE', *, *, #96169, .F. ) ;
#15736 = AXIS2_PLACEMENT_3D ( 'NONE', #48976, #79908, #10398 ) ;
#15737 = ADVANCED_FACE ( 'NONE', ( #8710 ), #68604, .F. ) ;
#15738 = CARTESIAN_POINT ( 'NONE',  ( -91.50906031749687486, -24.34968618360934300, 0.1864209137778843617 ) ) ;
#15739 = AXIS2_PLACEMENT_3D ( 'NONE', #31880, #27647, #79547 ) ;
#15740 = ORIENTED_EDGE ( 'NONE', *, *, #8761, .F. ) ;
#15741 = CARTESIAN_POINT ( 'NONE',  ( -58.55359039973971846, -23.96169478059713143, 10.65365249895718058 ) ) ;
#15742 = DIRECTION ( 'NONE',  ( -3.773278334444166432E-23, 1.000000000000000000, 0.000000000000000000 ) ) ;
#15743 = CARTESIAN_POINT ( 'NONE',  ( 19.93353245626563819, -6.116835970281883306, -1.500000000000002220 ) ) ;
#15744 = CARTESIAN_POINT ( 'NONE',  ( -21.05831370385527990, 5.553659732266172711, 11.49999999999999645 ) ) ;
#15745 = EDGE_CURVE ( 'NONE', #79100, #19988, #85314, .T. ) ;
#15746 = CARTESIAN_POINT ( 'NONE',  ( -98.52287095715006160, -29.50248528299804818, 1.056150453629042030 ) ) ;
#15747 = LINE ( 'NONE', #99472, #80719 ) ;
#15748 = CARTESIAN_POINT ( 'NONE',  ( -6.716530693746936898, -21.44081863256500142, 11.49999999999998934 ) ) ;
#15749 = EDGE_CURVE ( 'NONE', #60562, #10305, #49375, .T. ) ;
#15750 = CARTESIAN_POINT ( 'NONE',  ( -118.5167408753442260, -24.66019654487199730, 8.947790411086115725 ) ) ;
#15751 = PLANE ( 'NONE',  #25867 ) ;
#15752 = CARTESIAN_POINT ( 'NONE',  ( 4.959846025536391423, -5.876774720514417183, 20.32314756232572250 ) ) ;
#15753 = EDGE_LOOP ( 'NONE', ( #73047, #7359, #74876, #7755 ) ) ;
#15754 = EDGE_CURVE ( 'NONE', #47315, #48546, #39647, .T. ) ;
#15755 = ORIENTED_EDGE ( 'NONE', *, *, #26300, .T. ) ;
#15756 = ORIENTED_EDGE ( 'NONE', *, *, #47622, .T. ) ;
#15757 = CARTESIAN_POINT ( 'NONE',  ( 20.50650179695670872, -5.950058665555418180, -1.500000000000002220 ) ) ;
#15758 = ORIENTED_EDGE ( 'NONE', *, *, #74789, .F. ) ;
#15759 = CARTESIAN_POINT ( 'NONE',  ( -4.359323203648655998, -20.60729432550360585, 11.49999999999998934 ) ) ;
#15760 = CARTESIAN_POINT ( 'NONE',  ( -30.49166226875084718, -24.48011564457811673, 0.5642940035406436294 ) ) ;
#15761 = CARTESIAN_POINT ( 'NONE',  ( 15.29947331669757737, -3.406413700670902323, -27.16854001216721670 ) ) ;
#15762 = B_SPLINE_CURVE_WITH_KNOTS ( 'NONE', 3,
 ( #100295, #77471, #93202, #60284, #85093, #84596 ),
 .UNSPECIFIED., .F., .F.,
 ( 4, 2, 4 ),
 ( 6.384118678612693437E-06, 0.001386860460828375202, 0.002767336802978137989 ),
 .UNSPECIFIED. ) ;
#15763 = CARTESIAN_POINT ( 'NONE',  ( 3.036358173076929123, -5.876774720514419847, 20.87990785256409865 ) ) ;
#15764 = CARTESIAN_POINT ( 'NONE',  ( -9.458160343781703006, 19.84743614482962926, -1.500000000000002220 ) ) ;
#15765 = CARTESIAN_POINT ( 'NONE',  ( -87.52287095715006160, -23.47593901973090524, -1.443836447538996648 ) ) ;
#15766 = EDGE_LOOP ( 'NONE', ( #35964, #47017, #92619, #48338 ) ) ;
#15767 = DIRECTION ( 'NONE',  ( 3.773278334444167608E-23, -1.000000000000000000, 0.000000000000000000 ) ) ;
#15768 = LINE ( 'NONE', #39105, #12465 ) ;
#15769 = CARTESIAN_POINT ( 'NONE',  ( -18.00717387566553995, 10.56535500573724740, 11.49999999999999645 ) ) ;
#15770 = VECTOR ( 'NONE', #28975, 1000.000000000000000 ) ;
#15771 = CARTESIAN_POINT ( 'NONE',  ( 31.65781406150966149, -5.771867554241929987, 28.25297929084395321 ) ) ;
#15772 = CARTESIAN_POINT ( 'NONE',  ( -128.9228709571500531, -23.47596703998600631, 11.44779298504227860 ) ) ;
#15773 = CIRCLE ( 'NONE', #80608, 91.74549126261076992 ) ;
#15774 = CARTESIAN_POINT ( 'NONE',  ( -20.38992447862095148, -24.51869592734078651, 6.147794833475635379 ) ) ;
#15775 = CARTESIAN_POINT ( 'NONE',  ( 0.1273799443098547757, 21.28700333820561497, 11.49999999999998934 ) ) ;
#15776 = CARTESIAN_POINT ( 'NONE',  ( -19.77875734969026311, 6.143225279485574397, 27.31649921512899937 ) ) ;
#15777 = CARTESIAN_POINT ( 'NONE',  ( -107.5552259268662993, -23.96169478059713853, 10.65365249895717348 ) ) ;
#15778 = CARTESIAN_POINT ( 'NONE',  ( -35.52287095715006870, -29.50247984919015209, -1.443849546365060466 ) ) ;
#15779 = CARTESIAN_POINT ( 'NONE',  ( -4.968349358974361252, -5.876774720514412742, 19.46153846153847056 ) ) ;
#15780 = CARTESIAN_POINT ( 'NONE',  ( 12.95044643391442030, 18.39415735498938176, -1.500000000000002220 ) ) ;
#15781 = B_SPLINE_SURFACE_WITH_KNOTS ( 'NONE', 3, 3, ( 
 ( #35108, #27495, #58452, #72670 ),
 ( #34108, #89384, #12743, #84639 ),
 ( #15626, #5145, #67066, #76513 ),
 ( #30857, #45593, #30352, #46593 ),
 ( #407, #69921, #77518, #43714 ),
 ( #66580, #89883, #74649, #38471 ),
 ( #20352, #23738, #100341, #35608 ),
 ( #7516, #97492, #20857, #68918 ),
 ( #85139, #37968, #92250, #8018 ),
 ( #61326, #77015, #99844, #69423 ) ),
 .UNSPECIFIED., .F., .F., .F.,
 ( 4, 3, 3, 4 ),
 ( 4, 4 ),
 ( 0.0004766839783815427639, 0.1491231665100170578, 0.2234464077758348266, 0.2977696490416525954 ),
 ( 0.6495724517647905039, 0.6509722533490930330 ),
 .UNSPECIFIED. ) ;
#15782 = DIRECTION ( 'NONE',  ( -0.5656310827093757876, 2.995395837334947896E-15, -0.8246584009594636333 ) ) ;
#15783 = ORIENTED_EDGE ( 'NONE', *, *, #15797, .F. ) ;
#15784 = DIRECTION ( 'NONE',  ( 0.000000000000000000, 0.000000000000000000, 1.000000000000000000 ) ) ;
#15785 = CARTESIAN_POINT ( 'NONE',  ( -18.24527198174902765, 7.358211898524878336, 11.49999999999999645 ) ) ;
#15786 = CARTESIAN_POINT ( 'NONE',  ( -28.62287095715004526, -24.19530606561500008, 0.1850819291420055523 ) ) ;
#15787 = CARTESIAN_POINT ( 'NONE',  ( -20.27875734969026311, -6.143225279485574397, 21.75402280011862644 ) ) ;
#15788 = ORIENTED_EDGE ( 'NONE', *, *, #20794, .T. ) ;
#15789 = CARTESIAN_POINT ( 'NONE',  ( -99.63195852548790299, -23.96119346886881374, -0.6495511937831867089 ) ) ;
#15790 = CARTESIAN_POINT ( 'NONE',  ( -36.52287095715007581, -23.95044443724991723, 10.65354141964649415 ) ) ;
#15791 = CARTESIAN_POINT ( 'NONE',  ( -100.1102081092206930, -25.31439547524505684, 5.264240186624079776 ) ) ;
#15792 = VECTOR ( 'NONE', #29897, 1000.000000000000114 ) ;
#15793 = CARTESIAN_POINT ( 'NONE',  ( -24.90875734969025501, -3.316774720514426456, 26.43402280011862615 ) ) ;
#15794 = CARTESIAN_POINT ( 'NONE',  ( 5.037983044326730386, -19.10262670698400100, 11.49999999999998934 ) ) ;
#15795 = VERTEX_POINT ( 'NONE', #92428 ) ;
#15796 = CARTESIAN_POINT ( 'NONE',  ( 9.313311959394031447, 3.316774720514592545, -28.06297399525112013 ) ) ;
#15797 = EDGE_CURVE ( 'NONE', #16286, #85354, #31974, .T. ) ;
#15798 = AXIS2_PLACEMENT_3D ( 'NONE', #66811, #90125, #14485 ) ;
#15799 = APPROVAL_STATUS ( 'not_yet_approved' ) ;
#15800 = ADVANCED_FACE ( 'NONE', ( #1095 ), #81537, .T. ) ;
#15801 = VERTEX_POINT ( 'NONE', #9706 ) ;
#15802 = PLANE ( 'NONE',  #15930 ) ;
#15803 = CARTESIAN_POINT ( 'NONE',  ( -53.62287095715003460, -24.33832256526968507, 0.1851278514119814866 ) ) ;
#15804 = CARTESIAN_POINT ( 'NONE',  ( -81.48149462243459595, -25.23679622552714363, 6.293943003980942308 ) ) ;
#15805 = CARTESIAN_POINT ( 'NONE',  ( -98.89994392110364174, -25.26638266936259214, 6.299691109395265443 ) ) ;
#15806 = CARTESIAN_POINT ( 'NONE',  ( -2.104002878010082789, -5.876774720514410077, 19.15289935703627222 ) ) ;
#15807 = VECTOR ( 'NONE', #98506, 1000.000000000000114 ) ;
#15808 = CARTESIAN_POINT ( 'NONE',  ( -67.52287095715006160, -24.64965694238407323, 8.947790433994200043 ) ) ;
#15809 = PLANE ( 'NONE',  #51079 ) ;
#15810 = CARTESIAN_POINT ( 'NONE',  ( -13.93161493328335432, -14.37010051631055418, 11.49999999999998934 ) ) ;
#15811 = CARTESIAN_POINT ( 'NONE',  ( -8.160000000000000142, -9.636585826567531043, 1.623587105904843231 ) ) ;
#15812 = CARTESIAN_POINT ( 'NONE',  ( -45.49172329232699497, -24.40133493613049964, 9.663955038902802386 ) ) ;
#15813 = ORIENTED_EDGE ( 'NONE', *, *, #78206, .T. ) ;
#15814 = B_SPLINE_CURVE_WITH_KNOTS ( 'NONE', 3,
 ( #16951, #42320, #80351, #78832, #9333, #40296 ),
 .UNSPECIFIED., .F., .F.,
 ( 4, 2, 4 ),
 ( 6.384118696476699610E-06, 0.001386860460837304257, 0.002767336802978131918 ),
 .UNSPECIFIED. ) ;
#15815 = CARTESIAN_POINT ( 'NONE',  ( 10.50543233995236037, -4.482436650883735219, -26.67361961461832109 ) ) ;
#15816 = CARTESIAN_POINT ( 'NONE',  ( -109.4273347235498193, -25.18430276407331903, 3.857971852524231249 ) ) ;
#15817 = LINE ( 'NONE', #53402, #26692 ) ;
#15818 = CARTESIAN_POINT ( 'NONE',  ( -100.5228709571500616, -23.48786465467242479, 11.44779295918254114 ) ) ;
#15819 = DIRECTION ( 'NONE',  ( 0.000000000000000000, -0.3081562241202474572, -0.9513357669802769978 ) ) ;
#15820 = CARTESIAN_POINT ( 'NONE',  ( -10.16634758543296613, -5.965225279485572685, 30.00402280011862288 ) ) ;
#15821 = DIRECTION ( 'NONE',  ( -0.9921023176230513441, 0.000000000000000000, 0.1254312216594016538 ) ) ;
#15822 = CARTESIAN_POINT ( 'NONE',  ( 0.3910256410256394144, -5.876774720514412742, 19.63681891025641235 ) ) ;
#15823 = ORIENTED_EDGE ( 'NONE', *, *, #15652, .T. ) ;
#15824 = CARTESIAN_POINT ( 'NONE',  ( 17.44645523915803764, -10.38078700900905993, 11.49999999999998934 ) ) ;
#15825 = FACE_OUTER_BOUND ( 'NONE', #80273, .T. ) ;
#15826 = AXIS2_PLACEMENT_3D ( 'NONE', #47109, #1432, #55230 ) ;
#15827 = CARTESIAN_POINT ( 'NONE',  ( -76.62287095715007013, -23.48783264082478084, -1.443836473390065489 ) ) ;
#15828 = ORIENTED_EDGE ( 'NONE', *, *, #27558, .T. ) ;
#15829 = EDGE_CURVE ( 'NONE', #25204, #89557, #55388, .T. ) ;
#15830 = FACE_OUTER_BOUND ( 'NONE', #60017, .T. ) ;
#15831 = CARTESIAN_POINT ( 'NONE',  ( 18.81927703376926786, -7.057843677351100631, -1.500000000000002220 ) ) ;
#15832 = CARTESIAN_POINT ( 'NONE',  ( -6.733481718715807141, 19.98004043397084928, 11.49999999999999645 ) ) ;
#15833 = CARTESIAN_POINT ( 'NONE',  ( -4.051365815588555463, -21.74199345402511696, -1.500000000000002220 ) ) ;
#15834 = CARTESIAN_POINT ( 'NONE',  ( 4.502618398017903090, 20.03723546437915104, -1.500000000000002220 ) ) ;
#15835 = CARTESIAN_POINT ( 'NONE',  ( -60.49079332354545357, -24.63355581998385446, 0.9682620441943891043 ) ) ;
#15836 = ORIENTED_EDGE ( 'NONE', *, *, #4774, .T. ) ;
#15837 = DIRECTION ( 'NONE',  ( 8.334928612639484546E-17, 1.000000000000000000, 7.321843366904296032E-17 ) ) ;
#15838 = ORIENTED_EDGE ( 'NONE', *, *, #71117, .T. ) ;
#15839 = CARTESIAN_POINT ( 'NONE',  ( -6.072964844751159497, -6.376774720514410077, 19.44316438561912008 ) ) ;
#15840 = CARTESIAN_POINT ( 'NONE',  ( -70.52287095715007581, -24.99156044556120548, 7.747789690856173195 ) ) ;
#15841 = ORIENTED_EDGE ( 'NONE', *, *, #83710, .T. ) ;
#15842 = B_SPLINE_CURVE_WITH_KNOTS ( 'NONE', 3,
 ( #81478, #18563, #41414, #18068, #49538, #3370 ),
 .UNSPECIFIED., .F., .F.,
 ( 4, 2, 4 ),
 ( 0.000000000000000000, 0.001380901958385387894, 0.002761803916770775788 ),
 .UNSPECIFIED. ) ;
#15844 = ORIENTED_EDGE ( 'NONE', *, *, #38567, .F. ) ;
#15843 = EDGE_CURVE ( 'NONE', #20587, #49615, #73119, .T. ) ;
#15845 = ORIENTED_EDGE ( 'NONE', *, *, #987, .F. ) ;
#15846 = DIRECTION ( 'NONE',  ( 1.000000000000000000, 3.773278334444167608E-23, 8.201307833595939069E-29 ) ) ;
#15847 = DIRECTION ( 'NONE',  ( -3.773278334453079618E-23, 0.9999999999976377785, 2.173523156925979975E-06 ) ) ;
#15848 = FACE_OUTER_BOUND ( 'NONE', #38576, .T. ) ;
#15849 = CARTESIAN_POINT ( 'NONE',  ( -18.12278953325389708, -9.833843834435361586, -1.500000000000002220 ) ) ;
#15850 = CARTESIAN_POINT ( 'NONE',  ( 11.83326311654409935, 18.06170320929925310, 11.49999999999999645 ) ) ;
#15851 = ORIENTED_EDGE ( 'NONE', *, *, #17001, .T. ) ;
#15852 = ADVANCED_FACE ( 'NONE', ( #57407, #65028 ), #78690, .F. ) ;
#15853 = CARTESIAN_POINT ( 'NONE',  ( -42.22287095715005734, -23.47596703998600276, 11.44779298504227860 ) ) ;
#15854 = CARTESIAN_POINT ( 'NONE',  ( 3.325015365150250535, -5.876774720514402972, 18.26971317031913955 ) ) ;
#15855 = CARTESIAN_POINT ( 'NONE',  ( 3.152853332073482839, 22.16862046936333286, -1.500000000000002220 ) ) ;
#15856 = AXIS2_PLACEMENT_3D ( 'NONE', #37892, #84059, #77432 ) ;
#15857 = EDGE_CURVE ( 'NONE', #5378, #20580, #10208, .T. ) ;
#15858 = CARTESIAN_POINT ( 'NONE',  ( -103.6228709571500559, -29.50248528299804818, 1.056150453629042030 ) ) ;
#15859 = CARTESIAN_POINT ( 'NONE',  ( -53.01255352321339842, -4.772774720514425972, 35.59556822165056644 ) ) ;
#15860 = ORIENTED_EDGE ( 'NONE', *, *, #18647, .F. ) ;
#15861 = CARTESIAN_POINT ( 'NONE',  ( -100.4293229868110160, -25.31235227439576363, 4.721894440410697058 ) ) ;
#15862 = CARTESIAN_POINT ( 'NONE',  ( -35.52193564919225111, -23.48786465467240347, 11.44779295918255180 ) ) ;
#15863 = EDGE_CURVE ( 'NONE', #11023, #29369, #50138, .T. ) ;
#15864 = CARTESIAN_POINT ( 'NONE',  ( -13.90609606471210391, -15.62508359690603221, -1.500000000000002220 ) ) ;
#15865 = EDGE_CURVE ( 'NONE', #59928, #18750, #8966, .T. ) ;
#15866 = EDGE_LOOP ( 'NONE', ( #9512, #80742, #76305, #90470 ) ) ;
#15867 = B_SPLINE_CURVE_WITH_KNOTS ( 'NONE', 3,
 ( #78627, #69546, #30969, #85253, #55832, #7640, #9640, #63451, #22837, #38586, #86262, #47209, #77132, #26, #61936, #16742, #86758, #71047, #1536, #92866, #92366, #23343 ),
 .UNSPECIFIED., .F., .F.,
 ( 4, 2, 2, 2, 2, 2, 2, 2, 2, 2, 4 ),
 ( 0.0003089662623631434001, 0.001025905326923032615, 0.001742844391482921938, 0.002459783456042811262, 0.002818252988322752887, 0.003176722520602694947, 0.003535192052882637007, 0.003893661585162578632, 0.004610600649722459282, 0.005327539714282339932, 0.006044478778842219714 ),
 .UNSPECIFIED. ) ;
#15868 = CARTESIAN_POINT ( 'NONE',  ( 29.73860345376319358, 1.682774720514426114, -1.352392034746782823 ) ) ;
#15869 = VECTOR ( 'NONE', #56572, 1000.000000000000000 ) ;
#15870 = ORIENTED_EDGE ( 'NONE', *, *, #94562, .F. ) ;
#15871 = CARTESIAN_POINT ( 'NONE',  ( -101.9507253916653440, -29.50249654204571215, 6.236241424690079249 ) ) ;
#15872 = CARTESIAN_POINT ( 'NONE',  ( -20.37118330240554087, -5.769015352940915164, -1.500000000000002220 ) ) ;
#15873 = EDGE_LOOP ( 'NONE', ( #35647, #32233, #16205, #64146 ) ) ;
#15874 = CARTESIAN_POINT ( 'NONE',  ( 29.73860345376319003, -1.682774720514426114, -8.849814207987163783 ) ) ;
#15875 = CARTESIAN_POINT ( 'NONE',  ( 10.97640485992876691, 18.82695874702771377, 11.49999999999998934 ) ) ;
#15876 = CARTESIAN_POINT ( 'NONE',  ( -60.55620429048339304, -23.47596703998600276, 11.44779298504227505 ) ) ;
#15877 = AXIS2_PLACEMENT_3D ( 'NONE', #52889, #7704, #83828 ) ;
#15878 = LINE ( 'NONE', #29607, #82590 ) ;
#15879 = DIRECTION ( 'NONE',  ( -3.773278334453080206E-23, 0.9999999999976377785, 2.173523156925979975E-06 ) ) ;
#15880 = CARTESIAN_POINT ( 'NONE',  ( 4.919149715316761373, 21.27959583485438344, -1.500000000000002220 ) ) ;
#15881 = CARTESIAN_POINT ( 'NONE',  ( 6.429811694900724461, -6.376774720514426065, 21.48000018967326596 ) ) ;
#15882 = ORIENTED_EDGE ( 'NONE', *, *, #22851, .T. ) ;
#15883 = EDGE_CURVE ( 'NONE', #91742, #89308, #42180, .T. ) ;
#15884 = CARTESIAN_POINT ( 'NONE',  ( 7.141559373243376641, -5.876774720514415407, 19.83742167145384983 ) ) ;
#15885 = CARTESIAN_POINT ( 'NONE',  ( 30.93860345374796594, 6.475225279485573360, 19.84760796525321780 ) ) ;
#15886 = ORIENTED_EDGE ( 'NONE', *, *, #65178, .T. ) ;
#15887 = ORIENTED_EDGE ( 'NONE', *, *, #926, .F. ) ;
#15888 = B_SPLINE_CURVE_WITH_KNOTS ( 'NONE', 3,
 ( #13160, #45135, #74570, #97895 ),
 .UNSPECIFIED., .F., .F.,
 ( 4, 4 ),
 ( 3.422183298990500128E-11, 0.002177849098239042699 ),
 .UNSPECIFIED. ) ;
#15889 = ORIENTED_EDGE ( 'NONE', *, *, #30809, .T. ) ;
#15890 = DIRECTION ( 'NONE',  ( -1.000000000000000000, -3.773278334444167608E-23, -8.201307833595939069E-29 ) ) ;
#15891 = DIRECTION ( 'NONE',  ( -0.000000000000000000, 1.000000000000000000, -0.000000000000000000 ) ) ;
#15892 = CARTESIAN_POINT ( 'NONE',  ( 0.06830352742921809439, -21.21198074455918814, 11.49999999999998934 ) ) ;
#15893 = CARTESIAN_POINT ( 'NONE',  ( -125.5228709571500616, -23.47593901973090524, -1.443836447538996204 ) ) ;
#15894 = CARTESIAN_POINT ( 'NONE',  ( -80.40044610398997804, -25.03138299335276429, 7.562159499395756157 ) ) ;
#15895 = DIRECTION ( 'NONE',  ( -3.773278334453079618E-23, 0.9999999999976377785, 2.173523156925979975E-06 ) ) ;
#15896 = CARTESIAN_POINT ( 'NONE',  ( 30.09341516180546350, 1.477225279485574028, -11.39311774897855933 ) ) ;
#15897 = CARTESIAN_POINT ( 'NONE',  ( 18.67713048845720181, -5.233370074711279685, -1.500000000000002220 ) ) ;
#15898 = CARTESIAN_POINT ( 'NONE',  ( -69.56540253034138743, -25.29932401351703675, 5.636500610589230575 ) ) ;
#15899 = VERTEX_POINT ( 'NONE', #86823 ) ;
#15900 = CARTESIAN_POINT ( 'NONE',  ( -0.2416374764669896869, -19.45557994585427508, 11.49999999999999645 ) ) ;
#15901 = CARTESIAN_POINT ( 'NONE',  ( 9.299999999999993605, 12.00000000000002309, 2.100000000000000089 ) ) ;
#15902 = CARTESIAN_POINT ( 'NONE',  ( -80.11904448212310115, -25.13254330329641917, 7.046576512759410882 ) ) ;
#15903 = ORIENTED_EDGE ( 'NONE', *, *, #21288, .F. ) ;
#15904 = CARTESIAN_POINT ( 'NONE',  ( 2.993128331772667572, -5.876774720514403860, 18.53171057923899312 ) ) ;
#15905 = CARTESIAN_POINT ( 'NONE',  ( -54.52287095715006870, -29.50250786944525672, 11.44777988621624054 ) ) ;
#15906 = CARTESIAN_POINT ( 'NONE',  ( -64.62287095715005592, -24.50216790748205398, 0.6166512839542535040 ) ) ;
#15907 = EDGE_CURVE ( 'NONE', #3681, #53534, #17312, .T. ) ;
#15908 = CARTESIAN_POINT ( 'NONE',  ( -93.54470257384001286, -24.66019654487200441, 8.947790411086105067 ) ) ;
#15909 = CARTESIAN_POINT ( 'NONE',  ( -15.16444148636751521, -12.51942901160708921, -1.500000000000002220 ) ) ;
#15910 = B_SPLINE_SURFACE_WITH_KNOTS ( 'NONE', 3, 1, ( 
 ( #71713, #71210 ),
 ( #33649, #33140 ),
 ( #39745, #1201 ),
 ( #63108, #64628 ),
 ( #47876, #25532 ),
 ( #94035, #87934 ),
 ( #24520, #1705 ),
 ( #77792, #78795 ),
 ( #9294, #32638 ),
 ( #63614, #64122 ),
 ( #688, #48377 ),
 ( #55999, #95040 ),
 ( #86924, #26027 ),
 ( #56502, #95542 ),
 ( #16402, #78301 ),
 ( #87425, #17922 ),
 ( #48881, #79808 ),
 ( #10306, #36142 ),
 ( #42772, #51369 ),
 ( #58495, #66620 ),
 ( #43265, #3215 ),
 ( #97534, #89431 ),
 ( #88436, #19903 ),
 ( #49388, #50877 ),
 ( #28032, #82310 ),
 ( #81816, #27032 ),
 ( #58991, #20394 ) ),
 .UNSPECIFIED., .F., .F., .F.,
 ( 4, 1, 1, 1, 1, 1, 1, 1, 1, 1, 1, 1, 1, 1, 1, 1, 1, 1, 1, 1, 1, 1, 1, 1, 4 ),
 ( 2, 2 ),
 ( 0.000000000000000000, 0.06811324674912544452, 0.1325644684346005686, 0.1934266930244679106, 0.2502184821984413388, 0.3035685554824333332, 0.3535758444159123881, 0.4002351701272690576, 0.4435864585068350907, 0.4846193083749509301, 0.5242924705629079529, 0.5623796179232622983, 0.5990492626598917791, 0.6349401741080455963, 0.6697821542752002699, 0.7040087777416839110, 0.7378419440949924857, 0.7710977456761829441, 0.8038960730129318666, 0.8364148124046564270, 0.8686388349573493928, 0.9007151219040273604, 0.9333783422757061521, 0.9662128536530091294, 1.000000000000000000 ),
 ( 0.000000000000000000, 1.000000000000000000 ),
 .UNSPECIFIED. ) ;
#15911 = PLANE ( 'NONE',  #57462 ) ;
#15912 = ORIENTED_EDGE ( 'NONE', *, *, #8562, .T. ) ;
#15913 = CARTESIAN_POINT ( 'NONE',  ( 7.401388779597747103, 20.28278527911644247, -1.500000000000002220 ) ) ;
#15914 = CARTESIAN_POINT ( 'NONE',  ( -40.52633905974123962, -24.83618233451449342, 1.606449574219539711 ) ) ;
#15915 = LINE ( 'NONE', #70714, #13178 ) ;
#15916 = CARTESIAN_POINT ( 'NONE',  ( -3.733506833432379768, 22.73668382284982314, -1.500000000000002220 ) ) ;
#15917 = EDGE_CURVE ( 'NONE', #17108, #49884, #5528, .T. ) ;
#15918 = PERSON_AND_ORGANIZATION ( #70597, #27821 ) ;
#15919 = DIRECTION ( 'NONE',  ( 3.773278334444167608E-23, -1.000000000000000000, 0.000000000000000000 ) ) ;
#15920 = CARTESIAN_POINT ( 'NONE',  ( 4.653494883475234545, -6.376774720514415407, 20.13747874360300116 ) ) ;
#15921 = CARTESIAN_POINT ( 'NONE',  ( -121.5924664832264881, -23.48786465467241413, 11.44779295918253581 ) ) ;
#15922 = FACE_OUTER_BOUND ( 'NONE', #77731, .T. ) ;
#15923 = CARTESIAN_POINT ( 'NONE',  ( -111.0058427071010527, -25.10921409436117813, 2.995661355163232731 ) ) ;
#15924 = CARTESIAN_POINT ( 'NONE',  ( -129.5899315059631647, -23.73766607897671577, -1.055555164236443577 ) ) ;
#15925 = B_SPLINE_CURVE_WITH_KNOTS ( 'NONE', 3,
 ( #124, #8744, #54921, #62533, #23954, #54418 ),
 .UNSPECIFIED., .F., .F.,
 ( 4, 2, 4 ),
 ( 0.000000000000000000, 0.001380764517854760412, 0.002761529035709520824 ),
 .UNSPECIFIED. ) ;
#15926 = CARTESIAN_POINT ( 'NONE',  ( -99.19491584893809488, -25.31565985344014180, 4.406300475431831565 ) ) ;
#15927 = CARTESIAN_POINT ( 'NONE',  ( 19.23997954701083657, -5.074110557352235595, -1.500000000000002220 ) ) ;
#15928 = CARTESIAN_POINT ( 'NONE',  ( -101.3316698755723451, -25.26509388656816668, 3.891060496532311230 ) ) ;
#15929 = CARTESIAN_POINT ( 'NONE',  ( -4.880483578727112359, 19.22116399702514045, -1.500000000000002220 ) ) ;
#15930 = AXIS2_PLACEMENT_3D ( 'NONE', #8203, #88214, #26807 ) ;
#15931 = FACE_BOUND ( 'NONE', #9524, .T. ) ;
#15932 = CARTESIAN_POINT ( 'NONE',  ( -39.08546997848264226, -25.29116740964227361, 3.855771218128337896 ) ) ;
#15933 = PLANE ( 'NONE',  #60476 ) ;
#15934 = CARTESIAN_POINT ( 'NONE',  ( -5.109682455881146446, -20.12422286529520932, 11.49999999999999645 ) ) ;
#15935 = CARTESIAN_POINT ( 'NONE',  ( -7.640838998533831194, -5.876774720514417183, 20.32624910079993086 ) ) ;
#15936 = CC_DESIGN_PERSON_AND_ORGANIZATION_ASSIGNMENT ( #4830, #89069, ( #68385 ) ) ;
#15937 = FACE_OUTER_BOUND ( 'NONE', #32222, .T. ) ;
#15938 = CARTESIAN_POINT ( 'NONE',  ( 9.298244000614250382, 20.81247324795305431, 11.49999999999999645 ) ) ;
#15939 = EDGE_LOOP ( 'NONE', ( #35072, #7029, #37447, #10122 ) ) ;
#15940 = CARTESIAN_POINT ( 'NONE',  ( -69.62709768445154168, -24.51314013834315375, 0.6176544820404143987 ) ) ;
#15941 = CARTESIAN_POINT ( 'NONE',  ( -69.34467329208345632, -25.23938715212924322, 6.270976422656406868 ) ) ;
#15942 = ORIENTED_EDGE ( 'NONE', *, *, #40295, .F. ) ;
#15943 = AXIS2_PLACEMENT_3D ( 'NONE', #1101, #40670, #48284 ) ;
#15944 = CARTESIAN_POINT ( 'NONE',  ( -18.21026628907936029, 8.684577975296603469, 11.49999999999998934 ) ) ;
#15945 = DIRECTION ( 'NONE',  ( 0.000000000000000000, 0.9999999999976377785, 2.173523156925979128E-06 ) ) ;
#15946 = CARTESIAN_POINT ( 'NONE',  ( -40.91555040693666712, -25.30563909050597360, 4.985614010301523180 ) ) ;
#15947 = ORIENTED_EDGE ( 'NONE', *, *, #28566, .T. ) ;
#15948 = ORIENTED_EDGE ( 'NONE', *, *, #36144, .F. ) ;
#15949 = FACE_OUTER_BOUND ( 'NONE', #85870, .T. ) ;
#15950 = CARTESIAN_POINT ( 'NONE',  ( 16.68310095749102118, 15.68496000196893370, -1.500000000000002220 ) ) ;
#15951 = CARTESIAN_POINT ( 'NONE',  ( -51.29535283968221648, -25.18439786647864409, 3.923498624102081056 ) ) ;
#15952 = CARTESIAN_POINT ( 'NONE',  ( 19.28387207504633949, -9.851753786812027514, -1.500000000000002220 ) ) ;
#15953 = AXIS2_PLACEMENT_3D ( 'NONE', #14187, #96943, #13688 ) ;
#15954 = CARTESIAN_POINT ( 'NONE',  ( -40.94688081444584782, -25.03284417894045788, 7.563176522466704910 ) ) ;
#15955 = CARTESIAN_POINT ( 'NONE',  ( 18.69404101259207707, 9.334567778723176446, 11.49999999999999645 ) ) ;
#15956 = VERTEX_POINT ( 'NONE', #33545 ) ;
#15957 = CARTESIAN_POINT ( 'NONE',  ( -124.5216661205150928, -23.73766607897670866, -1.055555164236449350 ) ) ;
#15958 = CARTESIAN_POINT ( 'NONE',  ( -7.807709442696729063, 20.60712426125841645, -1.500000000000002220 ) ) ;
#15959 = CARTESIAN_POINT ( 'NONE',  ( -8.349999999999971223, 27.69999999999999574, 2.100000000000000089 ) ) ;
#15960 = CARTESIAN_POINT ( 'NONE',  ( -30.47287095715008576, -23.78634900524765072, 10.96467695203478065 ) ) ;
#15961 = VERTEX_POINT ( 'NONE', #64529 ) ;
#15962 = DIRECTION ( 'NONE',  ( 0.000000000000000000, 0.000000000000000000, 1.000000000000000000 ) ) ;
#15963 = DIRECTION ( 'NONE',  ( 0.000000000000000000, 0.9999999999976377785, 2.173523156925979128E-06 ) ) ;
#15964 = ORIENTED_EDGE ( 'NONE', *, *, #37313, .F. ) ;
#15965 = CARTESIAN_POINT ( 'NONE',  ( -72.60740660736958318, -23.48786465467241058, 11.44779295918254824 ) ) ;
#15966 = ORIENTED_EDGE ( 'NONE', *, *, #93289, .T. ) ;
#15967 = ORIENTED_EDGE ( 'NONE', *, *, #18486, .T. ) ;
#15968 = ADVANCED_FACE ( 'NONE', ( #10711 ), #95442, .F. ) ;
#15969 = DIRECTION ( 'NONE',  ( 1.000000000000000000, 0.000000000000000000, 0.000000000000000000 ) ) ;
#15970 = CARTESIAN_POINT ( 'NONE',  ( -95.62287095715007013, -24.92604778743017491, 8.074972756849353672 ) ) ;
#15971 = CARTESIAN_POINT ( 'NONE',  ( -36.54575551158481517, -24.15543982623906771, -0.2315651400026672579 ) ) ;
#15972 = CARTESIAN_POINT ( 'NONE',  ( 19.37909195245082472, -6.530858791768283211, -1.500000000000002220 ) ) ;
#15973 = ORIENTED_EDGE ( 'NONE', *, *, #5208, .T. ) ;
#15974 = CARTESIAN_POINT ( 'NONE',  ( -79.52287095715011844, -23.94994826722565406, -0.6494450866342715845 ) ) ;
#15975 = CARTESIAN_POINT ( 'NONE',  ( -0.02075734969026423599, -5.965225279485572685, -0.08597719988137648983 ) ) ;
#15976 = CARTESIAN_POINT ( 'NONE',  ( -77.62287095715005592, -24.64898659630367916, 1.056161002820826145 ) ) ;
#15977 = CARTESIAN_POINT ( 'NONE',  ( 9.404896790668452411, 20.21284700076377305, -1.500000000000002220 ) ) ;
#15978 = CARTESIAN_POINT ( 'NONE',  ( -55.52287095715005449, -24.15516710230293285, 10.28746687063726384 ) ) ;
#15979 = DIRECTION ( 'NONE',  ( 0.000000000000000000, 0.000000000000000000, 1.000000000000000000 ) ) ;
#15980 = ORIENTED_EDGE ( 'NONE', *, *, #17363, .T. ) ;
#15981 = CARTESIAN_POINT ( 'NONE',  ( -89.40841769935767047, -25.11033443737731474, 2.832404817301930056 ) ) ;
#15982 = FACE_OUTER_BOUND ( 'NONE', #62919, .T. ) ;
#15983 = EDGE_CURVE ( 'NONE', #60838, #75484, #53733, .T. ) ;
#15984 = CARTESIAN_POINT ( 'NONE',  ( -20.33245250387252767, 4.503473919074798104, 11.49999999999998934 ) ) ;
#15985 = ADVANCED_FACE ( 'NONE', ( #80218 ), #95941, .T. ) ;
#15986 = ORIENTED_EDGE ( 'NONE', *, *, #79267, .T. ) ;
#15988 = VERTEX_POINT ( 'NONE', #4606 ) ;
#15987 = CARTESIAN_POINT ( 'NONE',  ( -85.52287095715003318, -25.00182538069145011, 7.747789668545101094 ) ) ;
#15989 = VERTEX_POINT ( 'NONE', #43169 ) ;
#15990 = B_SPLINE_SURFACE_WITH_KNOTS ( 'NONE', 3, 3, ( 
 ( #91992, #60570, #53451, #14361 ),
 ( #29593, #44341, #91488, #31088 ),
 ( #83377, #84878, #77252, #21967 ),
 ( #84380, #144, #76747, #7757 ),
 ( #44837, #5763, #100078, #92487 ),
 ( #22463, #14861, #75269, #45827 ),
 ( #62058, #76260, #22957, #60070 ) ),
 .UNSPECIFIED., .F., .F., .F.,
 ( 4, 3, 4 ),
 ( 4, 4 ),
 ( 0.7945040050992251413, 0.8970133687736507877, 0.9995227324480764342 ),
 ( 0.8096997531712926133, 0.8110862888633306733 ),
 .UNSPECIFIED. ) ;
#15991 = CARTESIAN_POINT ( 'NONE',  ( -111.6228709571500559, -29.50248528299804818, 1.056150453629043584 ) ) ;
#15992 = CARTESIAN_POINT ( 'NONE',  ( 8.398332666215036824, -19.25654272332048578, -1.500000000000002220 ) ) ;
#15993 = ORIENTED_EDGE ( 'NONE', *, *, #47111, .F. ) ;
#15994 = CARTESIAN_POINT ( 'NONE',  ( -86.62287095715005592, -24.66019654487199375, 8.947790411086124607 ) ) ;
#15995 = VECTOR ( 'NONE', #50789, 1000.000000000000000 ) ;
#15996 = CARTESIAN_POINT ( 'NONE',  ( -55.62287095715004170, -24.51254535404256174, 9.355368623467651190 ) ) ;
#15997 = CARTESIAN_POINT ( 'NONE',  ( 7.732492003039795669, -3.316774720515257791, -27.16032169665734486 ) ) ;
#15998 = AXIS2_PLACEMENT_3D ( 'NONE', #89790, #20758, #13145 ) ;
#15999 = DIRECTION ( 'NONE',  ( 0.000000000000000000, 0.000000000000000000, -1.000000000000000000 ) ) ;
#16000 = CARTESIAN_POINT ( 'NONE',  ( -91.55620429048339304, -23.47593901973091235, -1.443836447539002865 ) ) ;
#16001 = DIRECTION ( 'NONE',  ( -1.000000000000000000, 0.000000000000000000, 0.000000000000000000 ) ) ;
#16003 = ORIENTED_EDGE ( 'NONE', *, *, #59308, .F. ) ;
#16002 = CARTESIAN_POINT ( 'NONE',  ( 9.120982285578694615, 20.23247719416018242, 11.49999999999999645 ) ) ;
#16004 = EDGE_CURVE ( 'NONE', #43186, #20125, #81220, .T. ) ;
#16005 = DIRECTION ( 'NONE',  ( 0.000000000000000000, 0.000000000000000000, -1.000000000000000000 ) ) ;
#16006 = FACE_OUTER_BOUND ( 'NONE', #72944, .T. ) ;
#16007 = ORIENTED_EDGE ( 'NONE', *, *, #73379, .T. ) ;
#16008 = CARTESIAN_POINT ( 'NONE',  ( 8.023449251107201974, -21.19570997880782670, -1.500000000000002220 ) ) ;
#16009 = VECTOR ( 'NONE', #84507, 1000.000000000000114 ) ;
#16011 = ORIENTED_EDGE ( 'NONE', *, *, #76010, .F. ) ;
#16010 = CARTESIAN_POINT ( 'NONE',  ( -29.05879606100779355, -25.09401859864639661, 6.517353683613309023 ) ) ;
#16012 = ORIENTED_EDGE ( 'NONE', *, *, #98497, .F. ) ;
#16013 = VECTOR ( 'NONE', #46405, 1000.000000000000114 ) ;
#16014 = FACE_OUTER_BOUND ( 'NONE', #10405, .T. ) ;
#16015 = CARTESIAN_POINT ( 'NONE',  ( 19.84801528777503776, 3.447069022702595742, 11.49999999999998934 ) ) ;
#16016 = DIRECTION ( 'NONE',  ( -1.000000000000000000, -3.504491870660219321E-16, 0.000000000000000000 ) ) ;
#16017 = EDGE_LOOP ( 'NONE', ( #70684, #93445, #1803, #85453 ) ) ;
#16018 = CARTESIAN_POINT ( 'NONE',  ( -3.826923076923078426, -5.876774720514409189, 19.19230769230769695 ) ) ;
#16019 = CARTESIAN_POINT ( 'NONE',  ( -15.79502933763849271, 15.79022959414610661, -1.500000000000002220 ) ) ;
#16020 = EDGE_CURVE ( 'NONE', #91432, #57584, #19803, .T. ) ;
#16021 = ORIENTED_EDGE ( 'NONE', *, *, #96724, .F. ) ;
#16022 = ORIENTED_EDGE ( 'NONE', *, *, #72561, .T. ) ;
#16023 = DIRECTION ( 'NONE',  ( -1.000000000000000000, -0.000000000000000000, -0.000000000000000000 ) ) ;
#16024 = CARTESIAN_POINT ( 'NONE',  ( -94.63333269353616117, -23.96169478059713143, 10.65365249895717881 ) ) ;
#16025 = CARTESIAN_POINT ( 'NONE',  ( -80.80255094563601403, -25.29787882119566333, 4.568986449336699174 ) ) ;
#16026 = CARTESIAN_POINT ( 'NONE',  ( -68.52287095715006160, -23.96177878511308990, 10.65340807706330573 ) ) ;
#16027 = DIRECTION ( 'NONE',  ( -0.000000000000000000, 1.000000000000000000, -0.000000000000000000 ) ) ;
#16028 = EDGE_CURVE ( 'NONE', #84261, #60824, #51774, .T. ) ;
#16029 = CARTESIAN_POINT ( 'NONE',  ( 3.395600993332231532, 19.23619202488179525, -1.500000000000002220 ) ) ;
#16030 = CARTESIAN_POINT ( 'NONE',  ( -78.52287095715006160, -29.50250786944525672, 11.44777988621623521 ) ) ;
#16031 = CARTESIAN_POINT ( 'NONE',  ( 0.6623178260406717976, 21.47796536025111536, -1.500000000000002220 ) ) ;
#16032 = CARTESIAN_POINT ( 'NONE',  ( -128.5556220342893141, -24.34968618360935011, 0.1864209137779018477 ) ) ;
#16033 = CARTESIAN_POINT ( 'NONE',  ( -54.62287095715005592, -24.64965695001467694, 8.947790433994185832 ) ) ;
#16034 = CARTESIAN_POINT ( 'NONE',  ( -117.6228709571500559, -23.47593901973091235, -1.443836447538997536 ) ) ;
#16035 = CARTESIAN_POINT ( 'NONE',  ( -111.6228709571500985, -23.73907113216991860, -1.053371485793221929 ) ) ;
#16036 = CARTESIAN_POINT ( 'NONE',  ( 13.94817355369617751, 18.09530419158152625, -1.500000000000002220 ) ) ;
#16037 = CIRCLE ( 'NONE', #93839, 251.4258649670780699 ) ;
#16038 = EDGE_CURVE ( 'NONE', #53278, #66705, #65984, .T. ) ;
#16039 = CALENDAR_DATE ( 2026, 9, 10 ) ;
#16040 = CARTESIAN_POINT ( 'NONE',  ( -101.6228709571500559, -23.47593901973091235, -1.443836447539001089 ) ) ;
#16041 = CARTESIAN_POINT ( 'NONE',  ( -2.762050907158362989, -5.876774720514416295, 19.89644244529369033 ) ) ;
#16042 = CARTESIAN_POINT ( 'NONE',  ( -13.81204400269958654, 14.50282280199826701, 11.49999999999999645 ) ) ;
#16043 = CARTESIAN_POINT ( 'NONE',  ( -78.94416233434603214, -25.31594624443190611, 5.924886392682762626 ) ) ;
#16044 = DIRECTION ( 'NONE',  ( 0.000000000000000000, 0.000000000000000000, -1.000000000000000000 ) ) ;
#16045 = CARTESIAN_POINT ( 'NONE',  ( 4.856316114246853388, -5.876774720514408301, 19.03119074624055074 ) ) ;
#16046 = DIRECTION ( 'NONE',  ( -3.773278334453079030E-23, 0.9999999999976377785, 2.173523156925979128E-06 ) ) ;
#16047 = ORIENTED_EDGE ( 'NONE', *, *, #39135, .T. ) ;
#16048 = CARTESIAN_POINT ( 'NONE',  ( -50.62287095715006302, -24.63345952396258198, 9.038047939301517175 ) ) ;
#16049 = B_SPLINE_CURVE_WITH_KNOTS ( 'NONE', 3,
 ( #50386, #33656, #72223, #49897, #64636, #11316 ),
 .UNSPECIFIED., .F., .F.,
 ( 4, 2, 4 ),
 ( 6.384118678609748304E-06, 0.001386860460828374334, 0.002767336802978138856 ),
 .UNSPECIFIED. ) ;
#16050 = CARTESIAN_POINT ( 'NONE',  ( -17.16505717403991227, -13.39166244882208012, -1.500000000000002220 ) ) ;
#16051 = CARTESIAN_POINT ( 'NONE',  ( -56.62287095715004881, -24.51387760970724372, 9.387446482453427166 ) ) ;
#16052 = CARTESIAN_POINT ( 'NONE',  ( -17.62174901100306101, -8.731699659924187173, -1.500000000000002220 ) ) ;
#16053 = DIRECTION ( 'NONE',  ( 1.000000000000000000, 0.000000000000000000, 0.000000000000000000 ) ) ;
#16054 = CARTESIAN_POINT ( 'NONE',  ( -41.05392197949270638, -25.20725972110717095, 3.457283663102085125 ) ) ;
#16055 = ITEM_DEFINED_TRANSFORMATION ( 'NONE', 'NONE', #50425,  #37391 ) ;
#16056 = CARTESIAN_POINT ( 'NONE',  ( -56.62287095715009144, -23.95044443724992433, 10.65354141964650125 ) ) ;
#16057 = CARTESIAN_POINT ( 'NONE',  ( -44.52287095715006160, -24.64898659630367916, 1.056161002820819261 ) ) ;
#16058 = CARTESIAN_POINT ( 'NONE',  ( -17.20787902393383462, -11.26661214947554157, 11.49999999999999645 ) ) ;
#16059 = CARTESIAN_POINT ( 'NONE',  ( -39.04303308397305727, -25.29008967749855685, 4.215216926603018166 ) ) ;
#16060 = CARTESIAN_POINT ( 'NONE',  ( -120.5901076504048177, -24.40034930558991633, 0.3402023900116107336 ) ) ;
#16061 = EDGE_CURVE ( 'NONE', #70795, #73934, #84087, .T. ) ;
#16062 = CARTESIAN_POINT ( 'NONE',  ( -22.20892344277460850, -4.061126821146308963, 11.49999999999999645 ) ) ;
#16063 = VERTEX_POINT ( 'NONE', #5087 ) ;
#16064 = CARTESIAN_POINT ( 'NONE',  ( -100.2051565992114632, -25.26387441634614817, 4.680112826087972522 ) ) ;
#16065 = DIRECTION ( 'NONE',  ( -3.773278334453079030E-23, 0.9999999999976377785, 2.173523156925979128E-06 ) ) ;
#16066 = VECTOR ( 'NONE', #14458, 1000.000000000000000 ) ;
#16067 = CARTESIAN_POINT ( 'NONE',  ( -125.5556643051668715, -24.15602025860897584, 10.28564288303534013 ) ) ;
#16068 = PLANE ( 'NONE',  #96939 ) ;
#16069 = ADVANCED_FACE ( 'NONE', ( #81720 ), #30987, .T. ) ;
#16070 = VECTOR ( 'NONE', #40510, 1000.000000000000000 ) ;
#16071 = DIRECTION ( 'NONE',  ( -0.000000000000000000, -1.000000000000000000, -0.000000000000000000 ) ) ;
#16072 = DIRECTION ( 'NONE',  ( 1.000000000000000000, 1.413818403454611288E-16, 0.000000000000000000 ) ) ;
#16073 = EDGE_CURVE ( 'NONE', #37981, #44655, #1794, .T. ) ;
#16074 = ADVANCED_FACE ( 'NONE', ( #98421 ), #42676, .T. ) ;
#16075 = ORIENTED_EDGE ( 'NONE', *, *, #54619, .F. ) ;
#16076 = CARTESIAN_POINT ( 'NONE',  ( 11.92049557817732364, -19.74369927386287671, 11.49999999999999645 ) ) ;
#16077 = CARTESIAN_POINT ( 'NONE',  ( 16.42120958226126604, -15.83219868413775622, -1.500000000000002220 ) ) ;
#16078 = CARTESIAN_POINT ( 'NONE',  ( 4.017909867803298063, -5.876774720514403860, 18.55402206357357286 ) ) ;
#16079 = VECTOR ( 'NONE', #75603, 1000.000000000000000 ) ;
#16080 = CARTESIAN_POINT ( 'NONE',  ( -96.59677831669986858, -23.73766607897670511, -1.055555164236452681 ) ) ;
#16081 = CARTESIAN_POINT ( 'NONE',  ( -63.62287095715004881, -23.47593901973091235, -1.443836447539007972 ) ) ;
#16082 = CARTESIAN_POINT ( 'NONE',  ( 18.78116726530667080, 12.29669497462397842, 11.49999999999999645 ) ) ;
#16083 = EDGE_LOOP ( 'NONE', ( #81095, #45697, #89704, #5491 ) ) ;
#16084 = VECTOR ( 'NONE', #40064, 1000.000000000000000 ) ;
#16085 = B_SPLINE_CURVE_WITH_KNOTS ( 'NONE', 3,
 ( #97482, #11741, #27974, #35096, #96984, #27484 ),
 .UNSPECIFIED., .F., .F.,
 ( 4, 2, 4 ),
 ( 6.391158118963033063E-06, 0.001387004593080786580, 0.002767618028042609802 ),
 .UNSPECIFIED. ) ;
#16086 = DIRECTION ( 'NONE',  ( -3.773278334453080206E-23, 0.9999999999976377785, 2.173523156925979975E-06 ) ) ;
#16087 = CARTESIAN_POINT ( 'NONE',  ( -43.52287095715006870, -24.50321055353803601, 9.387540953477522265 ) ) ;
#16088 = CARTESIAN_POINT ( 'NONE',  ( 6.821863743248424150, 20.85434273413645911, -1.500000000000002220 ) ) ;
#16089 = CARTESIAN_POINT ( 'NONE',  ( -28.62287095715004881, -29.50248298729119867, -6.412432996800796609E-05 ) ) ;
#16090 = CARTESIAN_POINT ( 'NONE',  ( -34.61899282609274309, -23.48786465467240347, 11.44779295918255535 ) ) ;
#16091 = CARTESIAN_POINT ( 'NONE',  ( -121.5228709571500616, -24.64965694238408034, 8.947790433994191162 ) ) ;
#16092 = ORIENTED_EDGE ( 'NONE', *, *, #91341, .F. ) ;
#16093 = CARTESIAN_POINT ( 'NONE',  ( 29.57907552799942508, 3.316774720514426456, 29.21818156447043791 ) ) ;
#16094 = DIRECTION ( 'NONE',  ( -1.000000000000000000, 0.000000000000000000, 5.238131417152343399E-15 ) ) ;
#16095 = ORIENTED_EDGE ( 'NONE', *, *, #79229, .F. ) ;
#16096 = CARTESIAN_POINT ( 'NONE',  ( 13.99439195134931069, 14.96789054323355828, -1.500000000000002220 ) ) ;
#16097 = ORIENTED_EDGE ( 'NONE', *, *, #75313, .F. ) ;
#16098 = ORIENTED_EDGE ( 'NONE', *, *, #46286, .T. ) ;
#16099 = ORIENTED_EDGE ( 'NONE', *, *, #47546, .F. ) ;
#16100 = ORIENTED_EDGE ( 'NONE', *, *, #4320, .F. ) ;
#16101 = EDGE_CURVE ( 'NONE', #34861, #42876, #24582, .T. ) ;
#16102 = CARTESIAN_POINT ( 'NONE',  ( 14.79121776280621425, -17.69394282334246427, -1.500000000000002220 ) ) ;
#16103 = CARTESIAN_POINT ( 'NONE',  ( -49.75863811138101056, -25.14487534265549229, 2.970700725601126635 ) ) ;
#16104 = CARTESIAN_POINT ( 'NONE',  ( -17.48930418531667996, -10.34094407820366612, -1.500000000000002220 ) ) ;
#16105 = VERTEX_POINT ( 'NONE', #75090 ) ;
#16106 = LINE ( 'NONE', #56197, #72056 ) ;
#16107 = CARTESIAN_POINT ( 'NONE',  ( -92.55472887090941470, -23.96119346886881374, -0.6495511937831873750 ) ) ;
#16108 = CARTESIAN_POINT ( 'NONE',  ( -47.58953762381671737, -23.48783264082478084, -1.443836473390070596 ) ) ;
#16109 = CARTESIAN_POINT ( 'NONE',  ( 4.451706829556401956, -5.876774720514407413, 18.91922570401084513 ) ) ;
#16111 = ORIENTED_EDGE ( 'NONE', *, *, #27341, .F. ) ;
#16110 = CARTESIAN_POINT ( 'NONE',  ( -20.49900048275977227, -6.559984590058941301, 11.49999999999999645 ) ) ;
#16112 = CARTESIAN_POINT ( 'NONE',  ( -75.49128703381974503, -24.92564183028979130, 1.928384488918256645 ) ) ;
#16113 = CARTESIAN_POINT ( 'NONE',  ( -61.49058198215474391, -24.66019654487199375, 8.947790411086119278 ) ) ;
#16114 = EDGE_LOOP ( 'NONE', ( #20571, #84913, #5885, #86273 ) ) ;
#16115 = CARTESIAN_POINT ( 'NONE',  ( -14.15296684469643118, 15.14645709676483420, 11.49999999999998934 ) ) ;
#16116 = EDGE_CURVE ( 'NONE', #52940, #58462, #89335, .T. ) ;
#16117 = EDGE_LOOP ( 'NONE', ( #40731, #96901, #45217, #41573 ) ) ;
#16119 = ORIENTED_EDGE ( 'NONE', *, *, #54590, .T. ) ;
#16118 = CARTESIAN_POINT ( 'NONE',  ( 0.000000000000000000, 1.530000000000000027, -0.3849999999999998979 ) ) ;
#16120 = EDGE_CURVE ( 'NONE', #65549, #68269, #31786, .T. ) ;
#16121 = CARTESIAN_POINT ( 'NONE',  ( -41.62875083135785559, -24.51419770103157347, 9.386484678747180510 ) ) ;
#16122 = CARTESIAN_POINT ( 'NONE',  ( -20.77875734969026311, 5.356774720514425603, 27.31649921512899937 ) ) ;
#16123 = ORIENTED_EDGE ( 'NONE', *, *, #22085, .T. ) ;
#16124 = EDGE_LOOP ( 'NONE', ( #93883, #67280, #80043, #25372 ) ) ;
#16125 = CARTESIAN_POINT ( 'NONE',  ( -53.52287095715006870, -23.47596703998600631, 11.44779298504229104 ) ) ;
#16126 = FACE_OUTER_BOUND ( 'NONE', #259, .T. ) ;
#16127 = CARTESIAN_POINT ( 'NONE',  ( -35.22287095715007155, -23.47596703998600276, 11.44779298504227683 ) ) ;
#16128 = CARTESIAN_POINT ( 'NONE',  ( -10.85839155550747392, 19.17434714687634667, 11.49999999999999645 ) ) ;
#16129 = EDGE_CURVE ( 'NONE', #16459, #16877, #36532, .T. ) ;
#16130 = CYLINDRICAL_SURFACE ( 'NONE', #57710, 10.20000000000000107 ) ;
#16131 = CARTESIAN_POINT ( 'NONE',  ( 22.10748686624256720, -4.471405416651531795, -1.500000000000002220 ) ) ;
#16132 = CARTESIAN_POINT ( 'NONE',  ( 18.73254098450790295, -9.497730595714260815, -1.500000000000002220 ) ) ;
#16133 = EDGE_CURVE ( 'NONE', #75014, #25230, #83898, .T. ) ;
#16134 = PLANE ( 'NONE',  #89718 ) ;
#16135 = ORIENTED_EDGE ( 'NONE', *, *, #49541, .T. ) ;
#16136 = EDGE_CURVE ( 'NONE', #47065, #94497, #7183, .T. ) ;
#16137 = EDGE_LOOP ( 'NONE', ( #36057, #70047, #32419, #71492 ) ) ;
#16138 = CARTESIAN_POINT ( 'NONE',  ( -80.62287095715005592, -24.99132157543084531, 2.256160258750667502 ) ) ;
#16139 = AXIS2_PLACEMENT_3D ( 'NONE', #81567, #35401, #96786 ) ;
#16140 = CARTESIAN_POINT ( 'NONE',  ( 22.02124265030973760, 7.743225279485574042, 16.20402280011862217 ) ) ;
#16141 = ORIENTED_EDGE ( 'NONE', *, *, #6099, .T. ) ;
#16142 = CARTESIAN_POINT ( 'NONE',  ( 20.45381123341165619, -5.387677532796200097, 11.49999999999998934 ) ) ;
#16143 = DIRECTION ( 'NONE',  ( 0.000000000000000000, 0.000000000000000000, -1.000000000000000000 ) ) ;
#16144 = CARTESIAN_POINT ( 'NONE',  ( -51.87944994387085274, -25.26040897669429697, 6.553577496112825251 ) ) ;
#16146 = CARTESIAN_POINT ( 'NONE',  ( -121.6259254375848400, -23.96119346886880663, -0.6495511937832033622 ) ) ;
#16145 = VECTOR ( 'NONE', #64053, 1000.000000000000114 ) ;
#16147 = CARTESIAN_POINT ( 'NONE',  ( -109.5228709571500474, -24.66019654487200086, 8.947790411086119278 ) ) ;
#16148 = CARTESIAN_POINT ( 'NONE',  ( 31.59111626279633711, -5.965225279485572685, 16.27760796525321751 ) ) ;
#16149 = CARTESIAN_POINT ( 'NONE',  ( -18.12599551585701008, -12.76988789260850332, -1.500000000000002220 ) ) ;
#16150 = CARTESIAN_POINT ( 'NONE',  ( 30.93860345374796594, 5.965225279485573573, 28.83647319851474933 ) ) ;
#16151 = ORIENTED_EDGE ( 'NONE', *, *, #73822, .T. ) ;
#16152 = CARTESIAN_POINT ( 'NONE',  ( 8.462785143989153269, 3.316774720514427344, -28.02084008811334215 ) ) ;
#16153 = CARTESIAN_POINT ( 'NONE',  ( -37.65704668824173496, -23.73766607897671221, -1.055555164236442023 ) ) ;
#16154 = CARTESIAN_POINT ( 'NONE',  ( -126.5555567441935523, -24.15543982623907482, -0.2315651400026573492 ) ) ;
#16155 = VECTOR ( 'NONE', #20011, 1000.000000000000114 ) ;
#16156 = CARTESIAN_POINT ( 'NONE',  ( 24.71017632900190719, -3.356774720514427379, 1.647607965253211848 ) ) ;
#16157 = DIRECTION ( 'NONE',  ( 0.000000000000000000, 0.000000000000000000, -1.000000000000000000 ) ) ;
#16158 = VECTOR ( 'NONE', #21225, 1000.000000000000114 ) ;
#16159 = CARTESIAN_POINT ( 'NONE',  ( 13.32768686175602646, -14.16729652289716057, 11.49999999999998934 ) ) ;
#16160 = AXIS2_PLACEMENT_3D ( 'NONE', #594, #1105, #62006 ) ;
#16161 = CARTESIAN_POINT ( 'NONE',  ( -19.04320821261859464, -9.809917703373946196, 11.49999999999998934 ) ) ;
#16162 = CARTESIAN_POINT ( 'NONE',  ( -62.50439628441560558, -24.15543982623907482, -0.2315651400026649265 ) ) ;
#16163 = DIRECTION ( 'NONE',  ( -0.000000000000000000, 1.000000000000000000, -0.000000000000000000 ) ) ;
#16164 = DIRECTION ( 'NONE',  ( 0.000000000000000000, 0.000000000000000000, -1.000000000000000000 ) ) ;
#16165 = CARTESIAN_POINT ( 'NONE',  ( -101.3603016561062589, -25.18440155020230975, 3.955748670072496864 ) ) ;
#16166 = CARTESIAN_POINT ( 'NONE',  ( -10.49914784070103124, -20.09245350529190688, -1.500000000000002220 ) ) ;
#16167 = B_SPLINE_CURVE_WITH_KNOTS ( 'NONE', 3,
 ( #43588, #43094, #11134, #35968, #97372, #65948 ),
 .UNSPECIFIED., .F., .F.,
 ( 4, 2, 4 ),
 ( 0.000000000000000000, 0.001380764517854769086, 0.002761529035709538171 ),
 .UNSPECIFIED. ) ;
#16168 = CIRCLE ( 'NONE', #29131, 2.399999999999999911 ) ;
#16169 = LINE ( 'NONE', #8061, #17457 ) ;
#16170 = CARTESIAN_POINT ( 'NONE',  ( -72.92287095715006728, -23.47593901973090169, -1.443836447538997536 ) ) ;
#16171 = CARTESIAN_POINT ( 'NONE',  ( 19.67252036444665109, 2.607452956813616218, 11.49999999999999645 ) ) ;
#16172 = CARTESIAN_POINT ( 'NONE',  ( -123.5198832471558319, -24.35071581493544457, 9.817618358456016381 ) ) ;
#16173 =( REPRESENTATION_RELATIONSHIP ('NONE','NONE', #96270, #44034 ) REPRESENTATION_RELATIONSHIP_WITH_TRANSFORMATION ( #47267 )SHAPE_REPRESENTATION_RELATIONSHIP( ) );
#16174 = CARTESIAN_POINT ( 'NONE',  ( -112.5895376238167245, -23.47596703998600631, 11.44779298504227683 ) ) ;
#16175 = FACE_OUTER_BOUND ( 'NONE', #67552, .T. ) ;
#16176 = ORIENTED_EDGE ( 'NONE', *, *, #89971, .T. ) ;
#16177 = CARTESIAN_POINT ( 'NONE',  ( -49.44452229720325676, -25.19195431728568124, 6.661645827231685857 ) ) ;
#16178 = CARTESIAN_POINT ( 'NONE',  ( -111.6228709571500559, -29.50247984919015209, -1.443849546365048253 ) ) ;
#16179 = CARTESIAN_POINT ( 'NONE',  ( -71.52287095715004739, -24.33927499327855415, 9.819080762295804732 ) ) ;
#16180 = CARTESIAN_POINT ( 'NONE',  ( -19.97641003480726241, 8.421946895145676848, -1.500000000000002220 ) ) ;
#16181 = CARTESIAN_POINT ( 'NONE',  ( -56.62367364272508752, -24.66019654487199375, 8.947790411086122830 ) ) ;
#16182 = CARTESIAN_POINT ( 'NONE',  ( 6.171429453590791425, 18.48145409631445446, -1.500000000000002220 ) ) ;
#16183 = DIRECTION ( 'NONE',  ( 0.000000000000000000, 0.000000000000000000, -1.000000000000000000 ) ) ;
#16184 = EDGE_LOOP ( 'NONE', ( #9634, #90032, #65325 ) ) ;
#16185 = CARTESIAN_POINT ( 'NONE',  ( -20.10423522397153562, 3.301153050299447056, 11.49999999999999645 ) ) ;
#16186 = CARTESIAN_POINT ( 'NONE',  ( -80.54559260964333589, -24.52300882791530157, 0.6510814631126378149 ) ) ;
#16187 = CARTESIAN_POINT ( 'NONE',  ( -31.52287095715004739, -23.48783264083373723, -1.443836473376154617 ) ) ;
#16188 = ADVANCED_FACE ( 'NONE', ( #15695 ), #84702, .T. ) ;
#16189 = ORIENTED_EDGE ( 'NONE', *, *, #3654, .T. ) ;
#16190 = CARTESIAN_POINT ( 'NONE',  ( -40.52088419996039903, -25.19528773117446363, 3.295766490768270884 ) ) ;
#16191 = DIRECTION ( 'NONE',  ( 0.000000000000000000, -2.173523156925980399E-06, 0.9999999999976378895 ) ) ;
#16192 = CARTESIAN_POINT ( 'NONE',  ( -49.03252113942349411, -25.25214557872430277, 5.540384592041287526 ) ) ;
#16193 = CARTESIAN_POINT ( 'NONE',  ( -40.57482057333878345, -24.92592662359561118, 8.075495903017996469 ) ) ;
#16194 = CARTESIAN_POINT ( 'NONE',  ( -127.6228709571500559, -23.47596703998600631, 11.44779298504227860 ) ) ;
#16195 = CARTESIAN_POINT ( 'NONE',  ( -0.3114230556345199963, -20.10660241673355486, 11.49999999999998934 ) ) ;
#16196 = CARTESIAN_POINT ( 'NONE',  ( 2.230654205607476293, 0.1647943925233646134, -7.514475724998474108E-17 ) ) ;
#16197 = ORIENTED_EDGE ( 'NONE', *, *, #47477, .T. ) ;
#16198 = EDGE_CURVE ( 'NONE', #41593, #46359, #3957, .T. ) ;
#16199 = DIRECTION ( 'NONE',  ( 0.000000000000000000, -1.000000000000000000, 0.000000000000000000 ) ) ;
#16200 = EDGE_CURVE ( 'NONE', #29911, #81363, #47620, .T. ) ;
#16201 = B_SPLINE_CURVE_WITH_KNOTS ( 'NONE', 3,
 ( #20616, #83009, #4414, #68300 ),
 .UNSPECIFIED., .F., .F.,
 ( 4, 4 ),
 ( 0.000000000000000000, 0.002134615384615373701 ),
 .UNSPECIFIED. ) ;
#16202 = ADVANCED_FACE ( 'NONE', ( #30919 ), #97078, .T. ) ;
#16203 = CARTESIAN_POINT ( 'NONE',  ( 19.82229641098322404, 11.46754112681587046, 11.49999999999999645 ) ) ;
#16204 = CARTESIAN_POINT ( 'NONE',  ( -21.73129956901698989, 6.668506094012985663, 11.49999999999998934 ) ) ;
#16205 = ORIENTED_EDGE ( 'NONE', *, *, #87644, .T. ) ;
#16206 = CARTESIAN_POINT ( 'NONE',  ( -81.26889778654310703, -25.32614216758069503, 4.442629388656409439 ) ) ;
#16207 = CARTESIAN_POINT ( 'NONE',  ( -97.52287095715007581, -23.47593901973090524, -1.443836447538996648 ) ) ;
#16208 = DIRECTION ( 'NONE',  ( 0.000000000000000000, 0.000000000000000000, -1.000000000000000000 ) ) ;
#16209 = ADVANCED_FACE ( 'NONE', ( #68984 ), #99908, .T. ) ;
#16210 = CARTESIAN_POINT ( 'NONE',  ( -49.52287095715006870, -24.51283580621365132, 0.6167428607019690423 ) ) ;
#16211 = VECTOR ( 'NONE', #43330, 1000.000000000000000 ) ;
#16212 = DIRECTION ( 'NONE',  ( 0.000000000000000000, -1.478457507934778393E-16, -1.000000000000000000 ) ) ;
#16213 = DIRECTION ( 'NONE',  ( 0.000000000000000000, 0.000000000000000000, 1.000000000000000000 ) ) ;
#16214 = ORIENTED_EDGE ( 'NONE', *, *, #63541, .F. ) ;
#16215 = AXIS2_PLACEMENT_3D ( 'NONE', #93468, #33588, #8249 ) ;
#16216 = CARTESIAN_POINT ( 'NONE',  ( 11.27307661227339430, 16.98952936956587934, -1.500000000000002220 ) ) ;
#16217 = ORIENTED_EDGE ( 'NONE', *, *, #24621, .F. ) ;
#16218 = ADVANCED_FACE ( 'NONE', ( #37037 ), #61390, .F. ) ;
#16219 = CARTESIAN_POINT ( 'NONE',  ( -10.52143791818333085, 20.43947972196396989, 11.49999999999998934 ) ) ;
#16220 = CARTESIAN_POINT ( 'NONE',  ( -7.324001883147635894, -5.876774720514414518, 20.17732409774492197 ) ) ;
#16221 = CARTESIAN_POINT ( 'NONE',  ( 31.04236049493789906, 5.965225279485572685, 19.84760796525321780 ) ) ;
#16222 = ORIENTED_EDGE ( 'NONE', *, *, #8875, .T. ) ;
#16223 = AXIS2_PLACEMENT_3D ( 'NONE', #28580, #66679, #67660 ) ;
#16224 = CARTESIAN_POINT ( 'NONE',  ( -108.5942905997697636, -23.73791477778912196, 11.05961554403169878 ) ) ;
#16225 = EDGE_CURVE ( 'NONE', #60171, #99147, #77580, .T. ) ;
#16226 = VECTOR ( 'NONE', #54733, 1000.000000000000114 ) ;
#16227 = CARTESIAN_POINT ( 'NONE',  ( -53.53686286912871140, -24.51419770103157347, 9.386484678747180510 ) ) ;
#16229 = ORIENTED_EDGE ( 'NONE', *, *, #65147, .T. ) ;
#16228 = CARTESIAN_POINT ( 'NONE',  ( 0.2649960030224881025, 21.33594185153759426, 11.49999999999999645 ) ) ;
#16230 = AXIS2_PLACEMENT_3D ( 'NONE', #68636, #93846, #99554 ) ;
#16231 = ORIENTED_EDGE ( 'NONE', *, *, #14652, .T. ) ;
#16232 = CARTESIAN_POINT ( 'NONE',  ( 21.93305185196877360, -3.456643806985262302, -1.500000000000002220 ) ) ;
#16233 = CARTESIAN_POINT ( 'NONE',  ( 15.34805171112899203, -13.82090413600154299, -1.500000000000002220 ) ) ;
#16234 = ADVANCED_FACE ( 'NONE', ( #22787 ), #54279, .F. ) ;
#16235 = VECTOR ( 'NONE', #50369, 1000.000000000000114 ) ;
#16236 = ORIENTED_EDGE ( 'NONE', *, *, #8741, .F. ) ;
#16237 = CARTESIAN_POINT ( 'NONE',  ( -4.752075056065355518, -6.376774720514406525, 19.17724329193115551 ) ) ;
#16238 = B_SPLINE_CURVE_WITH_KNOTS ( 'NONE', 3,
 ( #51210, #57838, #12636, #5029 ),
 .UNSPECIFIED., .F., .F.,
 ( 4, 4 ),
 ( 0.7593203366958898304, 0.7603210837366550789 ),
 .UNSPECIFIED. ) ;
#16239 = CARTESIAN_POINT ( 'NONE',  ( -68.92091305805531931, -25.32724624944561853, 4.398071659717722959 ) ) ;
#16240 = CIRCLE ( 'NONE', #19499, 28.45799999999999486 ) ;
#16241 = EDGE_LOOP ( 'NONE', ( #13707, #76487, #88945, #43071 ) ) ;
#16242 = CARTESIAN_POINT ( 'NONE',  ( -51.62287095715007723, -24.35013146730202394, 9.818937971375115481 ) ) ;
#16243 = ORIENTED_EDGE ( 'NONE', *, *, #28753, .T. ) ;
#16244 = DIRECTION ( 'NONE',  ( -1.000000000000000000, 0.000000000000000000, -0.000000000000000000 ) ) ;
#16245 = CARTESIAN_POINT ( 'NONE',  ( -48.52287095715009002, -24.33832256527049154, 0.1851278514138615938 ) ) ;
#16246 = CARTESIAN_POINT ( 'NONE',  ( 8.468106961216914641, 19.09613275528424836, -1.500000000000002220 ) ) ;
#16247 = CARTESIAN_POINT ( 'NONE',  ( -13.95179422449595208, 16.79422078803934326, 11.49999999999999645 ) ) ;
#16248 = EDGE_CURVE ( 'NONE', #75416, #67086, #68490, .T. ) ;
#16249 = B_SPLINE_CURVE_WITH_KNOTS ( 'NONE', 3,
 ( #92146, #16516, #84537, #63222 ),
 .UNSPECIFIED., .F., .F.,
 ( 4, 4 ),
 ( 0.000000000000000000, 9.999999999998897304E-05 ),
 .UNSPECIFIED. ) ;
#16250 = CARTESIAN_POINT ( 'NONE',  ( -27.61674701359889639, -24.89280003310657108, 7.602796328702011941 ) ) ;
#16251 = CARTESIAN_POINT ( 'NONE',  ( -98.90291818520829281, -25.23555723607559997, 6.309050697855190570 ) ) ;
#16252 = CARTESIAN_POINT ( 'NONE',  ( 22.44084908143146251, -0.7541981612834567361, 11.49999999999998934 ) ) ;
#16253 = EDGE_CURVE ( 'NONE', #57780, #84750, #39034, .T. ) ;
#16254 = CARTESIAN_POINT ( 'NONE',  ( -118.5879162516116168, -24.66019654487199730, 8.947790411086115725 ) ) ;
#16255 = CARTESIAN_POINT ( 'NONE',  ( -87.52287095715006160, -23.48783264083352762, -1.443836473376473695 ) ) ;
#16256 = CARTESIAN_POINT ( 'NONE',  ( 31.88667425545054002, 1.682774720514426114, -9.651215965565025812 ) ) ;
#16257 = ORIENTED_EDGE ( 'NONE', *, *, #88724, .F. ) ;
#16258 = ORIENTED_EDGE ( 'NONE', *, *, #33885, .F. ) ;
#16259 = EDGE_CURVE ( 'NONE', #48203, #32532, #49953, .T. ) ;
#16260 = EDGE_LOOP ( 'NONE', ( #57470, #89751, #67072, #55580 ) ) ;
#16261 = CARTESIAN_POINT ( 'NONE',  ( -18.60337119584764665, 10.53494341765418874, -1.500000000000002220 ) ) ;
#16262 = CARTESIAN_POINT ( 'NONE',  ( 20.54922051473491607, -8.805037660420627077, 11.49999999999999645 ) ) ;
#16263 = EDGE_LOOP ( 'NONE', ( #57348, #78136, #58324, #60204 ) ) ;
#16264 = CARTESIAN_POINT ( 'NONE',  ( 21.00884048613226440, 1.293913838035418040, 11.49999999999998934 ) ) ;
#16265 = CARTESIAN_POINT ( 'NONE',  ( -30.42620999589370356, -24.66174847805420001, 1.095666116063856776 ) ) ;
#16266 = CARTESIAN_POINT ( 'NONE',  ( 18.23660095519748481, -8.086948576924280374, -1.500000000000002220 ) ) ;
#16267 = CARTESIAN_POINT ( 'NONE',  ( -50.63516635189558457, -24.63419186844610564, 9.035850630976916875 ) ) ;
#16268 = CARTESIAN_POINT ( 'NONE',  ( -43.52287095715008292, -24.35013146730203815, 9.818937971375106599 ) ) ;
#16269 = CARTESIAN_POINT ( 'NONE',  ( -19.92591009635028243, 9.278653061003369729, -1.500000000000002220 ) ) ;
#16270 = CARTESIAN_POINT ( 'NONE',  ( -87.52287095715007581, -24.50216790748205398, 0.6166512839542537261 ) ) ;
#16271 = ORIENTED_EDGE ( 'NONE', *, *, #87761, .T. ) ;
#16272 = LINE ( 'NONE', #85276, #14402 ) ;
#16273 = DIRECTION ( 'NONE',  ( 0.000000000000000000, 0.000000000000000000, 1.000000000000000000 ) ) ;
#16274 = CARTESIAN_POINT ( 'NONE',  ( 3.748101851616784774, 20.49759516964078188, 11.49999999999999645 ) ) ;
#16275 = CARTESIAN_POINT ( 'NONE',  ( 31.61913385939691423, -4.417689821282788643, 26.66246549260776177 ) ) ;
#16276 = CARTESIAN_POINT ( 'NONE',  ( -8.349999999999971223, 27.69999999999999574, 2.100000000000000089 ) ) ;
#16277 = CARTESIAN_POINT ( 'NONE',  ( -56.52287095715009002, -23.48783264082476308, -1.443836473390091690 ) ) ;
#16278 = CARTESIAN_POINT ( 'NONE',  ( -21.31669061289120037, -0.5855882196083471714, 11.49999999999998934 ) ) ;
#16279 = CARTESIAN_POINT ( 'NONE',  ( -98.51906314342498661, -23.73791477778912196, 11.05961554403170588 ) ) ;
#16280 = CARTESIAN_POINT ( 'NONE',  ( -66.58953762381673869, -23.47596703998600276, 11.44779298504227505 ) ) ;
#16281 = AXIS2_PLACEMENT_3D ( 'NONE', #96619, #17504, #78886 ) ;
#16282 = CARTESIAN_POINT ( 'NONE',  ( -31.92287095715005307, -23.47596703998600276, 11.44779298504227683 ) ) ;
#16283 = CARTESIAN_POINT ( 'NONE',  ( -70.65368560070751869, -25.28687673834294003, 5.910757521653128066 ) ) ;
#16284 = CARTESIAN_POINT ( 'NONE',  ( 17.90692129536829924, 13.62026984716248101, -1.500000000000002220 ) ) ;
#16285 = LINE ( 'NONE', #60485, #99255 ) ;
#16286 = VERTEX_POINT ( 'NONE', #57289 ) ;
#16287 = CARTESIAN_POINT ( 'NONE',  ( -78.97939175184666283, -25.29137798281832872, 5.597646679547159110 ) ) ;
#16288 = CARTESIAN_POINT ( 'NONE',  ( -31.54519140916136521, -24.15620529776627379, 10.23563542870661536 ) ) ;
#16289 = CARTESIAN_POINT ( 'NONE',  ( -9.502044936771568473, -17.27029980899984452, 11.49999999999999645 ) ) ;
#16290 = CARTESIAN_POINT ( 'NONE',  ( -125.6228709571500559, -24.15431212366393154, -0.2830839119429250372 ) ) ;
#16291 = CARTESIAN_POINT ( 'NONE',  ( 14.53567905697413565, -3.934666312338137129, -28.27917189340610804 ) ) ;
#16292 = ORIENTED_EDGE ( 'NONE', *, *, #90031, .T. ) ;
#16293 = CARTESIAN_POINT ( 'NONE',  ( -99.54829949207251616, -24.51314013834316796, 0.6176544820404243907 ) ) ;
#16294 = DIRECTION ( 'NONE',  ( -0.000000000000000000, 1.000000000000000000, -0.000000000000000000 ) ) ;
#16295 = CARTESIAN_POINT ( 'NONE',  ( -99.94284412489217573, -25.31439557162453369, 5.308582698213717421 ) ) ;
#16296 = CARTESIAN_POINT ( 'NONE',  ( -123.5228709571500616, -23.48786465467242479, 11.44779295918253759 ) ) ;
#16297 = CARTESIAN_POINT ( 'NONE',  ( 8.221391366598689743, 17.94232518691122635, 11.49999999999998934 ) ) ;
#16298 = AXIS2_PLACEMENT_3D ( 'NONE', #15399, #38240, #53988 ) ;
#16299 = ORIENTED_EDGE ( 'NONE', *, *, #54274, .F. ) ;
#16300 = AXIS2_PLACEMENT_3D ( 'NONE', #46820, #85875, #16352 ) ;
#16301 = CARTESIAN_POINT ( 'NONE',  ( 9.313311959400177642, 6.376774720514760020, -28.06297399545715976 ) ) ;
#16302 = AXIS2_PLACEMENT_3D ( 'NONE', #20155, #88688, #73461 ) ;
#16303 = APPROVAL_DATE_TIME ( #96812, #22686 ) ;
#16304 = ORIENTED_EDGE ( 'NONE', *, *, #77577, .F. ) ;
#16305 = DIRECTION ( 'NONE',  ( -0.000000000000000000, 2.173523156925979552E-06, -0.9999999999976378895 ) ) ;
#16306 = CARTESIAN_POINT ( 'NONE',  ( -53.62287095715004170, -23.94994826722514958, -0.6494450866351740848 ) ) ;
#16307 = LINE ( 'NONE', #24919, #29619 ) ;
#16308 = CARTESIAN_POINT ( 'NONE',  ( -66.52287095715007581, -23.72747288104470087, -1.053458166803226792 ) ) ;
#16309 = CARTESIAN_POINT ( 'NONE',  ( -1.304987980769231948, -6.376774720514413630, 19.76512419871795245 ) ) ;
#16310 = ADVANCED_FACE ( 'NONE', ( #2484 ), #70997, .T. ) ;
#16311 = CARTESIAN_POINT ( 'NONE',  ( -94.62287095715005592, -24.65952944569304606, 1.056160979905700348 ) ) ;
#16312 = EDGE_CURVE ( 'NONE', #5889, #97460, #78577, .T. ) ;
#16313 = CARTESIAN_POINT ( 'NONE',  ( -43.52287095715006160, -23.48786465467240347, 11.44779295918255180 ) ) ;
#16314 = CARTESIAN_POINT ( 'NONE',  ( -11.57650325489309395, -16.32560983125179277, 11.49999999999998934 ) ) ;
#16315 = EDGE_CURVE ( 'NONE', #75250, #50604, #64407, .T. ) ;
#16316 = CARTESIAN_POINT ( 'NONE',  ( -99.38436720317001516, -25.27532962555875784, 3.296897355697630871 ) ) ;
#16317 = CARTESIAN_POINT ( 'NONE',  ( 31.27206728860909024, -4.132774720514318822, -3.930752063305056332 ) ) ;
#16318 = ORIENTED_EDGE ( 'NONE', *, *, #48812, .T. ) ;
#16319 = EDGE_CURVE ( 'NONE', #60391, #57062, #64533, .T. ) ;
#16320 = LINE ( 'NONE', #39656, #98799 ) ;
#16321 = CARTESIAN_POINT ( 'NONE',  ( -109.3965479632025080, -25.18430294384156554, 3.940680077104115941 ) ) ;
#16322 = CARTESIAN_POINT ( 'NONE',  ( -120.6228709571500843, -24.52232992886364471, 0.6492154411906172484 ) ) ;
#16323 = CARTESIAN_POINT ( 'NONE',  ( -101.8161100070499714, -25.25287247409161040, 6.236250661346399049 ) ) ;
#16324 = CARTESIAN_POINT ( 'NONE',  ( -27.68651082257923335, -24.77145582263907286, 2.274903367125437281 ) ) ;
#16325 = CARTESIAN_POINT ( 'NONE',  ( -51.70072539166533687, -25.26279899730468159, 3.987152082073251780 ) ) ;
#16326 = DIRECTION ( 'NONE',  ( -0.000000000000000000, -0.000000000000000000, -1.000000000000000000 ) ) ;
#16327 = EDGE_CURVE ( 'NONE', #64237, #97633, #89841, .T. ) ;
#16328 = CARTESIAN_POINT ( 'NONE',  ( 5.635247460261607166, -5.876774720514423400, 21.53093896358932469 ) ) ;
#16329 = EDGE_LOOP ( 'NONE', ( #63622, #25951, #46193, #96869 ) ) ;
#16330 = CARTESIAN_POINT ( 'NONE',  ( -11.07518157712430096, -17.02944518001645946, -1.500000000000002220 ) ) ;
#16331 = DIRECTION ( 'NONE',  ( 0.000000000000000000, 0.000000000000000000, 1.000000000000000000 ) ) ;
#16332 = CARTESIAN_POINT ( 'NONE',  ( -129.6228709571500417, -29.50250786944525672, 11.44777988621622633 ) ) ;
#16333 = ORIENTED_EDGE ( 'NONE', *, *, #1623, .T. ) ;
#16334 = PLANE ( 'NONE',  #3211 ) ;
#16335 = CARTESIAN_POINT ( 'NONE',  ( 3.569899647507075890, 19.86734082857295647, -1.500000000000002220 ) ) ;
#16336 = CARTESIAN_POINT ( 'NONE',  ( 20.98173926746349238, 2.650078317256617577, 11.49999999999999645 ) ) ;
#16337 = CARTESIAN_POINT ( 'NONE',  ( 1.014068502963303864, -22.09113584270698993, -1.500000000000002220 ) ) ;
#16338 = VECTOR ( 'NONE', #17034, 1000.000000000000114 ) ;
#16339 = CARTESIAN_POINT ( 'NONE',  ( -12.99546161633903552, -15.93940442571882876, -1.500000000000002220 ) ) ;
#16340 = B_SPLINE_CURVE_WITH_KNOTS ( 'NONE', 3,
 ( #18720, #51185, #27347, #20715, #5004, #4014 ),
 .UNSPECIFIED., .F., .F.,
 ( 4, 2, 4 ),
 ( 1.570755371634190273E-05, 0.001396183895866088404, 0.002776660238015835145 ),
 .UNSPECIFIED. ) ;
#16341 = CARTESIAN_POINT ( 'NONE',  ( -60.48803809078037119, -24.73486907724917572, 1.287355809206962576 ) ) ;
#16342 = ORIENTED_EDGE ( 'NONE', *, *, #50857, .F. ) ;
#16343 = DIRECTION ( 'NONE',  ( -0.8264557562326033668, -0.000000000000000000, -0.5630016722799281448 ) ) ;
#16344 = ORIENTED_EDGE ( 'NONE', *, *, #54722, .T. ) ;
#16345 = CARTESIAN_POINT ( 'NONE',  ( -99.52287095715006160, -24.64965694238407323, 8.947790433994194714 ) ) ;
#16346 = CARTESIAN_POINT ( 'NONE',  ( -61.62287095715005592, -23.96177878511308634, 10.65340807706330573 ) ) ;
#16347 = ORIENTED_EDGE ( 'NONE', *, *, #14594, .F. ) ;
#16348 = EDGE_LOOP ( 'NONE', ( #72393, #89634, #26191, #56058 ) ) ;
#16349 = VERTEX_POINT ( 'NONE', #2992 ) ;
#16350 = CARTESIAN_POINT ( 'NONE',  ( -28.47875734969025885, 6.475225279485573360, -0.08597719988137300651 ) ) ;
#16351 = CARTESIAN_POINT ( 'NONE',  ( 7.164391295225654765, -5.876774720514419847, 20.71606273170883838 ) ) ;
#16352 = DIRECTION ( 'NONE',  ( 0.000000000000000000, 0.000000000000000000, 1.000000000000000000 ) ) ;
#16353 = CARTESIAN_POINT ( 'NONE',  ( 14.37238272058661259, 14.81585024043302035, -1.500000000000002220 ) ) ;
#16354 = CARTESIAN_POINT ( 'NONE',  ( 15.89274262425319861, 14.76810421718133171, 11.49999999999999645 ) ) ;
#16355 = EDGE_LOOP ( 'NONE', ( #65830, #31142, #63404, #48036 ) ) ;
#16356 = CARTESIAN_POINT ( 'NONE',  ( -100.5562042904833930, -23.47596703998600631, 11.44779298504227683 ) ) ;
#16357 = CARTESIAN_POINT ( 'NONE',  ( -60.62287095715004881, -24.14321612903115977, -0.2833117244521707323 ) ) ;
#16358 = CARTESIAN_POINT ( 'NONE',  ( -7.019573500991415749, 21.25910006591672996, -1.500000000000002220 ) ) ;
#16359 = EDGE_CURVE ( 'NONE', #92914, #31760, #55277, .T. ) ;
#16360 = CARTESIAN_POINT ( 'NONE',  ( -79.34687923781920915, -25.27874842775003117, 5.960409258949917799 ) ) ;
#16361 = FACE_OUTER_BOUND ( 'NONE', #79524, .T. ) ;
#16362 = VERTEX_POINT ( 'NONE', #25813 ) ;
#16363 = DIRECTION ( 'NONE',  ( 0.000000000000000000, 2.173523156925980399E-06, -0.9999999999976378895 ) ) ;
#16364 = AXIS2_PLACEMENT_3D ( 'NONE', #33267, #64255, #34781 ) ;
#16365 = CARTESIAN_POINT ( 'NONE',  ( -35.53620344211212512, -24.52399227489126687, 9.353111116836519301 ) ) ;
#16366 =( GEOMETRIC_REPRESENTATION_CONTEXT ( 3 ) GLOBAL_UNCERTAINTY_ASSIGNED_CONTEXT ( ( #34800 ) ) GLOBAL_UNIT_ASSIGNED_CONTEXT ( ( #79474, #81347, #89461 ) ) REPRESENTATION_CONTEXT ( 'NONE', 'WORKASPACE' ) );
#16367 = VERTEX_POINT ( 'NONE', #33929 ) ;
#16368 = ADVANCED_FACE ( 'NONE', ( #16692 ), #56783, .T. ) ;
#16369 = CARTESIAN_POINT ( 'NONE',  ( -6.660000000000001030, -10.77121780415746599, 1.154761385154455366 ) ) ;
#16370 = ORIENTED_EDGE ( 'NONE', *, *, #85679, .T. ) ;
#16371 = CARTESIAN_POINT ( 'NONE',  ( -50.62287095715010565, -24.82576562982392687, 8.398263435472973271 ) ) ;
#16372 = CARTESIAN_POINT ( 'NONE',  ( -3.044128750896296420, -20.94304649679510888, -1.500000000000002220 ) ) ;
#16373 = EDGE_LOOP ( 'NONE', ( #73419, #69812, #28239, #99376 ) ) ;
#16374 = CARTESIAN_POINT ( 'NONE',  ( -50.53592633393567013, -24.63355581998386867, 0.9682620441943859957 ) ) ;
#16375 = CARTESIAN_POINT ( 'NONE',  ( -21.01659442711627790, -5.882202039844940167, -1.500000000000002220 ) ) ;
#16376 = DIRECTION ( 'NONE',  ( -3.773278334453079030E-23, 0.9999999999976377785, 2.173523156925979128E-06 ) ) ;
#16377 = CARTESIAN_POINT ( 'NONE',  ( 8.349999999999972999, 27.69999999999999574, 2.100000000000000089 ) ) ;
#16378 = DIRECTION ( 'NONE',  ( 0.000000000000000000, -0.9999999999976377785, -2.173523156925979975E-06 ) ) ;
#16379 = CARTESIAN_POINT ( 'NONE',  ( 11.26692973276593968, -18.67385317477220497, -1.500000000000002220 ) ) ;
#16380 = CARTESIAN_POINT ( 'NONE',  ( -1.267404104715736279, -6.376774720514411854, 19.66076420632889921 ) ) ;
#16381 = ORIENTED_EDGE ( 'NONE', *, *, #32898, .F. ) ;
#16382 = CARTESIAN_POINT ( 'NONE',  ( 1.949999999999999956, 0.1925000000000007538, -0.1924999999999994493 ) ) ;
#16383 = CARTESIAN_POINT ( 'NONE',  ( -85.59143639821803617, -24.40133493613049964, 9.663955038902802386 ) ) ;
#16384 = B_SPLINE_CURVE_WITH_KNOTS ( 'NONE', 3,
 ( #374, #92709, #15590, #9488 ),
 .UNSPECIFIED., .F., .F.,
 ( 4, 4 ),
 ( 0.6602573981240899004, 0.6692638293962055451 ),
 .UNSPECIFIED. ) ;
#16385 = EDGE_LOOP ( 'NONE', ( #9498, #42490, #49873, #73061 ) ) ;
#16386 = ORIENTED_EDGE ( 'NONE', *, *, #68246, .T. ) ;
#16387 = ORIENTED_EDGE ( 'NONE', *, *, #77382, .T. ) ;
#16388 = DIRECTION ( 'NONE',  ( 0.000000000000000000, 0.000000000000000000, -1.000000000000000000 ) ) ;
#16389 = CARTESIAN_POINT ( 'NONE',  ( -86.62287095715004170, -23.47593901973091235, -1.443836447539002865 ) ) ;
#16390 = CARTESIAN_POINT ( 'NONE',  ( 20.41123533131232648, 5.719371238976541427, -1.500000000000002220 ) ) ;
#16391 = CARTESIAN_POINT ( 'NONE',  ( -94.63332968182956506, -23.96119346886881019, -0.6495511937832051386 ) ) ;
#16392 = CARTESIAN_POINT ( 'NONE',  ( -79.10019335338344604, -25.27791785562742533, 6.701028845095781783 ) ) ;
#16393 = CARTESIAN_POINT ( 'NONE',  ( 22.11522345091601949, -4.214729766064097660, -16.31575456565007443 ) ) ;
#16394 = LINE ( 'NONE', #10295, #50798 ) ;
#16395 = CARTESIAN_POINT ( 'NONE',  ( 18.72033823704212097, 5.060218808788302880, -1.500000000000002220 ) ) ;
#16396 = CARTESIAN_POINT ( 'NONE',  ( -69.34303308397305443, -25.25559839591755207, 6.209207386190695566 ) ) ;
#16397 = ORIENTED_EDGE ( 'NONE', *, *, #78411, .T. ) ;
#16398 = CARTESIAN_POINT ( 'NONE',  ( -14.81708852449743929, -12.69844354874750181, 11.49999999999999645 ) ) ;
#16399 = CARTESIAN_POINT ( 'NONE',  ( -45.62287095715004881, -25.00182538069145011, 7.747789668545099317 ) ) ;
#16400 = CARTESIAN_POINT ( 'NONE',  ( -79.78457243948635380, -25.16093448558851620, 6.875308263077232418 ) ) ;
#16401 = VERTEX_POINT ( 'NONE', #64909 ) ;
#16402 = CARTESIAN_POINT ( 'NONE',  ( 4.585161930874343206, -6.376774720514427841, 21.47592444013076118 ) ) ;
#16403 = CARTESIAN_POINT ( 'NONE',  ( 0.2746452767749879009, 3.927610442141378666, -2.677392948487098267E-15 ) ) ;
#16404 = PLANE ( 'NONE',  #82833 ) ;
#16405 = CARTESIAN_POINT ( 'NONE',  ( -93.55475863340156195, -23.96169478059713853, 10.65365249895717348 ) ) ;
#16406 = CARTESIAN_POINT ( 'NONE',  ( -11.90832679833862073, -15.64659449181510986, 11.49999999999998934 ) ) ;
#16407 = CARTESIAN_POINT ( 'NONE',  ( -117.6228709571501270, -24.35013146730205236, 9.818937971375103047 ) ) ;
#16408 = ORIENTED_EDGE ( 'NONE', *, *, #75076, .F. ) ;
#16409 = CARTESIAN_POINT ( 'NONE',  ( 20.07693369621832602, 7.961103810760662647, 11.49999999999998934 ) ) ;
#16410 = CARTESIAN_POINT ( 'NONE',  ( -40.55015522979748255, -24.15503026093912453, -0.2815557561904605821 ) ) ;
#16411 = CARTESIAN_POINT ( 'NONE',  ( -23.29179552176162105, -0.3587747205144061202, -17.29637630388739211 ) ) ;
#16412 = CARTESIAN_POINT ( 'NONE',  ( -43.62287095715004881, -24.64898659630367206, 1.056161002820819261 ) ) ;
#16413 = B_SPLINE_CURVE_WITH_KNOTS ( 'NONE', 3,
 ( #42296, #35658, #12297, #51883, #13294, #88446, #43768, #44269, #65629, #28042 ),
 .UNSPECIFIED., .F., .F.,
 ( 4, 2, 2, 2, 4 ),
 ( 0.000000000000000000, 0.0004833345490728424001, 0.0009666690981456848002, 0.001450003647218527092, 0.001933338196291368299 ),
 .UNSPECIFIED. ) ;
#16414 = CALENDAR_DATE ( 2026, 9, 10 ) ;
#16415 = CARTESIAN_POINT ( 'NONE',  ( -56.52287095715006870, -23.47596703998600631, 11.44779298504228926 ) ) ;
#16416 = CARTESIAN_POINT ( 'NONE',  ( -20.27875734969026311, -4.543225279485573864, 26.25402280011862288 ) ) ;
#16417 = CARTESIAN_POINT ( 'NONE',  ( 6.666194146093591399, -6.376774720514413630, 19.75460921626947908 ) ) ;
#16418 = CYLINDRICAL_SURFACE ( 'NONE', #82315, 12.23252173913042995 ) ;
#16419 = ADVANCED_FACE ( 'NONE', ( #95818 ), #86114, .T. ) ;
#16420 = FACE_OUTER_BOUND ( 'NONE', #80895, .T. ) ;
#16421 = DIRECTION ( 'NONE',  ( 0.000000000000000000, -1.000000000000000000, 0.000000000000000000 ) ) ;
#16422 = CARTESIAN_POINT ( 'NONE',  ( -68.52287095715006160, -23.47596703998600631, 11.44779298504228748 ) ) ;
#16423 = CARTESIAN_POINT ( 'NONE',  ( 1.402406813841059030, 19.88454085074057076, 11.49999999999998934 ) ) ;
#16424 = EDGE_CURVE ( 'NONE', #95862, #3328, #57775, .T. ) ;
#16425 = LINE ( 'NONE', #61635, #43626 ) ;
#16426 = CARTESIAN_POINT ( 'NONE',  ( -0.3680779360730609406, 19.82951397037014729, -1.500000000000002220 ) ) ;
#16427 = DIRECTION ( 'NONE',  ( -0.000000000000000000, 0.000000000000000000, 1.000000000000000000 ) ) ;
#16428 = EDGE_CURVE ( 'NONE', #46879, #52307, #66889, .T. ) ;
#16429 = AXIS2_PLACEMENT_3D ( 'NONE', #94813, #3483, #24305 ) ;
#16430 = EDGE_CURVE ( 'NONE', #6678, #54547, #58275, .T. ) ;
#16431 = CC_DESIGN_SECURITY_CLASSIFICATION ( #40782, ( #87801 ) ) ;
#16432 = CARTESIAN_POINT ( 'NONE',  ( -40.25203966287474344, -25.10925593919035492, 2.839407324615607298 ) ) ;
#16433 = CARTESIAN_POINT ( 'NONE',  ( -35.62287095715008434, -24.82576562982393398, 8.398263435472959060 ) ) ;
#16434 = CARTESIAN_POINT ( 'NONE',  ( -0.3852054317258338245, -20.75737367715079174, 11.49999999999999645 ) ) ;
#16435 = DIRECTION ( 'NONE',  ( -0.000000000000000000, 1.000000000000000000, -0.000000000000000000 ) ) ;
#16436 = EDGE_CURVE ( 'NONE', #23706, #91326, #80595, .T. ) ;
#16437 = CARTESIAN_POINT ( 'NONE',  ( -106.6282284235315245, -24.15543982623907127, -0.2315651400026576268 ) ) ;
#16438 = CARTESIAN_POINT ( 'NONE',  ( -7.601706241105644857, -21.46296766604531570, 11.49999999999999645 ) ) ;
#16439 = ORIENTED_EDGE ( 'NONE', *, *, #85079, .F. ) ;
#16440 = CARTESIAN_POINT ( 'NONE',  ( -57.62287095715007723, -24.34917612406837861, 0.1852690917426648154 ) ) ;
#16441 = DIRECTION ( 'NONE',  ( -0.1489078231574191280, 0.000000000000000000, 0.9888510809027406534 ) ) ;
#16442 = ORIENTED_EDGE ( 'NONE', *, *, #66654, .F. ) ;
#16443 = CARTESIAN_POINT ( 'NONE',  ( 12.43249465596513126, -15.92577207200969092, 11.49999999999998934 ) ) ;
#16444 = EDGE_CURVE ( 'NONE', #17917, #52403, #42556, .T. ) ;
#16445 = DIRECTION ( 'NONE',  ( -3.773278334453079618E-23, 0.9999999999976377785, 2.173523156925979975E-06 ) ) ;
#16446 = CARTESIAN_POINT ( 'NONE',  ( -7.160000000000000142, 1.990213166801898970, 6.144159427248533589 ) ) ;
#16447 = ORIENTED_EDGE ( 'NONE', *, *, #98152, .F. ) ;
#16448 = DIRECTION ( 'NONE',  ( 0.000000000000000000, -2.173523156925979552E-06, 0.9999999999976378895 ) ) ;
#16449 = CARTESIAN_POINT ( 'NONE',  ( -18.54830753475928518, 13.48922247889305837, 11.49999999999998934 ) ) ;
#16450 = PLANE ( 'NONE',  #69762 ) ;
#16451 = CARTESIAN_POINT ( 'NONE',  ( 13.31326451270642330, 17.06472021985377552, -1.500000000000002220 ) ) ;
#16452 = DIRECTION ( 'NONE',  ( 0.000000000000000000, -1.000000000000000000, 0.000000000000000000 ) ) ;
#16453 = CARTESIAN_POINT ( 'NONE',  ( 2.313481123293766206, -20.83243486019555135, 11.49999999999999645 ) ) ;
#16454 = ORIENTED_EDGE ( 'NONE', *, *, #55526, .T. ) ;
#16455 = CARTESIAN_POINT ( 'NONE',  ( -107.6228709571500843, -23.72773821059536559, 11.05748984161097503 ) ) ;
#16456 = CARTESIAN_POINT ( 'NONE',  ( -115.2228709571500787, -23.47596703998600631, 11.44779298504227860 ) ) ;
#16457 = CARTESIAN_POINT ( 'NONE',  ( -10.85839155550747392, 19.17434714687634667, -1.500000000000002220 ) ) ;
#16458 = CARTESIAN_POINT ( 'NONE',  ( -124.4728709571500360, -25.21113200442380275, 5.000950865234349507 ) ) ;
#16459 = VERTEX_POINT ( 'NONE', #49664 ) ;
#16460 = AXIS2_PLACEMENT_3D ( 'NONE', #61216, #15011, #86026 ) ;
#16461 = DIRECTION ( 'NONE',  ( -0.7071067811865513475, -0.7071067811865435759, 0.000000000000000000 ) ) ;
#16462 = LINE ( 'NONE', #85988, #64101 ) ;
#16463 = VERTEX_POINT ( 'NONE', #27312 ) ;
#16464 = CARTESIAN_POINT ( 'NONE',  ( -123.6228709571500559, -24.64965695001469115, 8.947790433994175174 ) ) ;
#16465 = ORIENTED_EDGE ( 'NONE', *, *, #13837, .T. ) ;
#16466 = EDGE_LOOP ( 'NONE', ( #2551, #29329, #49200, #54175 ) ) ;
#16467 = CARTESIAN_POINT ( 'NONE',  ( 13.99288689683290166, 5.965225279485572685, -28.28242551218217926 ) ) ;
#16468 = CARTESIAN_POINT ( 'NONE',  ( -83.52287095715013265, -24.33927499327856125, 9.819080762295813614 ) ) ;
#16469 = CARTESIAN_POINT ( 'NONE',  ( -36.57553010991347264, -24.65952944569304606, 1.056160979905696129 ) ) ;
#16470 = CARTESIAN_POINT ( 'NONE',  ( 18.57849760351508195, 8.651319581928444080, -1.500000000000002220 ) ) ;
#16471 = EDGE_CURVE ( 'NONE', #23306, #45965, #50653, .T. ) ;
#16472 = ORIENTED_EDGE ( 'NONE', *, *, #15418, .F. ) ;
#16473 = CARTESIAN_POINT ( 'NONE',  ( -116.5895376238167103, -24.66019654487199375, 8.947790411086122830 ) ) ;
#16474 = CARTESIAN_POINT ( 'NONE',  ( -44.62370635163588872, -24.65952944569304606, 1.056160979905693909 ) ) ;
#16475 = CARTESIAN_POINT ( 'NONE',  ( 13.59451591917074431, 3.316774720514426456, -28.23515841827053308 ) ) ;
#16476 = CARTESIAN_POINT ( 'NONE',  ( 22.08996893241407378, 3.065900275835479860, 11.49999999999998934 ) ) ;
#16477 = ADVANCED_FACE ( 'NONE', ( #65407 ), #3984, .T. ) ;
#16478 = CARTESIAN_POINT ( 'NONE',  ( -55.52287095715006870, -25.00182538069145011, 7.747789668545106423 ) ) ;
#16479 = CARTESIAN_POINT ( 'NONE',  ( -2.188401442307694289, -5.876774720514411854, 19.46153846153846700 ) ) ;
#16480 = ORIENTED_EDGE ( 'NONE', *, *, #29880, .F. ) ;
#16481 = CARTESIAN_POINT ( 'NONE',  ( -29.03649758528140623, -24.85412015691543530, 2.179221534033828345 ) ) ;
#16482 = CARTESIAN_POINT ( 'NONE',  ( -3.749999999999999556, 26.59999999999999432, 0.000000000000000000 ) ) ;
#16483 = CARTESIAN_POINT ( 'NONE',  ( -17.75621389795859884, -10.86975384844714831, -1.500000000000002220 ) ) ;
#16484 = AXIS2_PLACEMENT_3D ( 'NONE', #38037, #76582, #31426 ) ;
#16485 = ORIENTED_EDGE ( 'NONE', *, *, #20226, .T. ) ;
#16487 = VERTEX_POINT ( 'NONE', #20185 ) ;
#16486 = DIRECTION ( 'NONE',  ( -0.7512896232465892110, -0.000000000000000000, -0.6599726524652350657 ) ) ;
#16488 = VERTEX_POINT ( 'NONE', #34926 ) ;
#16489 = CARTESIAN_POINT ( 'NONE',  ( -51.21833214457227257, -25.12217806580932944, 6.843755411117837362 ) ) ;
#16490 = CARTESIAN_POINT ( 'NONE',  ( 4.154569570224219355, 20.57273982587956240, -1.500000000000002220 ) ) ;
#16491 = ADVANCED_FACE ( 'NONE', ( #11578 ), #89714, .F. ) ;
#16492 = ORIENTED_EDGE ( 'NONE', *, *, #22301, .F. ) ;
#16493 = DIRECTION ( 'NONE',  ( 0.000000000000000000, 1.000000000000000000, 0.000000000000000000 ) ) ;
#16494 = CARTESIAN_POINT ( 'NONE',  ( -37.52287095715009713, -24.33927499327855770, 9.819080762295813614 ) ) ;
#16495 = DIRECTION ( 'NONE',  ( -1.000000000000000000, -0.000000000000000000, 0.000000000000000000 ) ) ;
#16496 = DIRECTION ( 'NONE',  ( 0.000000000000000000, 0.000000000000000000, -1.000000000000000000 ) ) ;
#16497 = CARTESIAN_POINT ( 'NONE',  ( 9.315600972258334167, -0.3587747205144265483, 28.35070303307545458 ) ) ;
#16498 = CARTESIAN_POINT ( 'NONE',  ( -65.62287095715001328, -24.83620972994592080, 8.398175272781363887 ) ) ;
#16500 = VERTEX_POINT ( 'NONE', #90205 ) ;
#16499 = CARTESIAN_POINT ( 'NONE',  ( -22.11188964843745453, -1.696007508606716341, 11.49999999999999645 ) ) ;
#16501 = CARTESIAN_POINT ( 'NONE',  ( -98.89303308397306580, -25.26498937201382233, 6.110950154240443410 ) ) ;
#16502 = EDGE_CURVE ( 'NONE', #66705, #94640, #69345, .T. ) ;
#16503 = CARTESIAN_POINT ( 'NONE',  ( -44.62287095715007013, -24.35013146730203104, 9.818937971375117257 ) ) ;
#16504 = EDGE_LOOP ( 'NONE', ( #48354, #76157, #73645, #2294 ) ) ;
#16505 = CARTESIAN_POINT ( 'NONE',  ( -19.66899025692886838, 11.29834648773183581, -1.500000000000002220 ) ) ;
#16507 = ORIENTED_EDGE ( 'NONE', *, *, #9563, .T. ) ;
#16506 = LINE ( 'NONE', #33753, #62019 ) ;
#16508 = AXIS2_PLACEMENT_3D ( 'NONE', #24671, #2359, #87081 ) ;
#16509 = EDGE_LOOP ( 'NONE', ( #48101, #55495, #7399, #3906, #32467, #15191, #79872, #97834, #53198, #57957, #57351, #37604, #68034, #82986, #56677, #86503, #40613, #55430, #92483, #55242, #18206, #12870, #43580, #25197, #8842 ) ) ;
#16510 = PRODUCT_DEFINITION_FORMATION_WITH_SPECIFIED_SOURCE ( 'ANY', '', #63584, .NOT_KNOWN. ) ;
#16511 = CARTESIAN_POINT ( 'NONE',  ( 30.64697572893789967, 5.232796261063635157, 0.6042509527386027424 ) ) ;
#16512 = CC_DESIGN_DATE_AND_TIME_ASSIGNMENT ( #70717, #8316, ( #29472 ) ) ;
#16513 = CARTESIAN_POINT ( 'NONE',  ( -11.96439459519798554, -16.23097265130270728, -1.500000000000002220 ) ) ;
#16514 = DIRECTION ( 'NONE',  ( -3.773278334453079030E-23, 0.9999999999976377785, 2.173523156925979128E-06 ) ) ;
#16515 = ORIENTED_EDGE ( 'NONE', *, *, #94557, .F. ) ;
#16516 = CARTESIAN_POINT ( 'NONE',  ( -39.58953762381673158, -23.48786465467240347, 11.44779295918255180 ) ) ;
#16517 = CARTESIAN_POINT ( 'NONE',  ( -15.72835732567950195, 15.92727474065614501, -1.500000000000002220 ) ) ;
#16518 = ORIENTED_EDGE ( 'NONE', *, *, #91847, .T. ) ;
#16519 = VERTEX_POINT ( 'NONE', #12579 ) ;
#16520 = PLANE ( 'NONE',  #43339 ) ;
#16521 = DIRECTION ( 'NONE',  ( 0.000000000000000000, -1.000000000000000000, 0.000000000000000000 ) ) ;
#16522 = CARTESIAN_POINT ( 'NONE',  ( -40.11011405477550795, -25.31552197567200224, 5.046770785554223870 ) ) ;
#16523 = LINE ( 'NONE', #7418, #87054 ) ;
#16524 = CARTESIAN_POINT ( 'NONE',  ( 14.23870388848190771, 5.152774720514427642, -26.44223458220801248 ) ) ;
#16525 = CARTESIAN_POINT ( 'NONE',  ( 2.036066721924049805, 19.47704226162102614, 11.49999999999998934 ) ) ;
#16526 = DIRECTION ( 'NONE',  ( 0.000000000000000000, -1.000000000000000000, 0.000000000000000000 ) ) ;
#16527 = ORIENTED_EDGE ( 'NONE', *, *, #79840, .T. ) ;
#16528 = CARTESIAN_POINT ( 'NONE',  ( 13.13055478438326773, -17.03443908202477886, -1.500000000000002220 ) ) ;
#16529 = DIRECTION ( 'NONE',  ( -0.9685340172660600322, 0.000000000000000000, 0.2488812114211667315 ) ) ;
#16530 = CARTESIAN_POINT ( 'NONE',  ( -121.5228709571501042, -23.48783264082477018, -1.443836473390083253 ) ) ;
#16531 = CARTESIAN_POINT ( 'NONE',  ( -129.5228709571501042, -24.51387760970725793, 9.387446482453407626 ) ) ;
#16532 = CARTESIAN_POINT ( 'NONE',  ( -68.62287095715005592, -23.47596703998600631, 11.44779298504227505 ) ) ;
#16533 = CARTESIAN_POINT ( 'NONE',  ( -17.89994474767736676, -14.32179853049041363, -1.500000000000002220 ) ) ;
#16534 = CIRCLE ( 'NONE', #18220, 12.65241003308275758 ) ;
#16535 = PERSON_AND_ORGANIZATION_ROLE ( 'creator' ) ;
#16536 = CARTESIAN_POINT ( 'NONE',  ( -96.59382141558563717, -23.96169478059713498, 10.65365249895717881 ) ) ;
#16537 = CARTESIAN_POINT ( 'NONE',  ( -2.220741593810419801, -5.876774720514411854, 19.46247113826587238 ) ) ;
#16538 = CARTESIAN_POINT ( 'NONE',  ( 20.02521558760690112, -0.9251608499524575091, 11.49999999999999645 ) ) ;
#16539 = CARTESIAN_POINT ( 'NONE',  ( -80.21014334459538020, -25.31594316633425734, 4.508707480579172255 ) ) ;
#16540 = CARTESIAN_POINT ( 'NONE',  ( -57.52287095715003318, -24.66019654487198665, 8.947790411086121054 ) ) ;
#16541 = CARTESIAN_POINT ( 'NONE',  ( 3.960454120839856706, -5.876774720514403860, 18.17119035270509997 ) ) ;
#16542 = CARTESIAN_POINT ( 'NONE',  ( -119.5228709571500758, -24.64898659630368627, 1.056161002820833028 ) ) ;
#16543 = ADVANCED_FACE ( 'NONE', ( #59263 ), #4971, .F. ) ;
#16544 = ORIENTED_EDGE ( 'NONE', *, *, #34316, .T. ) ;
#16545 = DIRECTION ( 'NONE',  ( 0.000000000000000000, -1.000000000000000000, 0.000000000000000000 ) ) ;
#16546 = CARTESIAN_POINT ( 'NONE',  ( 18.41774212405765709, -11.57998961627671441, 11.49999999999998934 ) ) ;
#16547 = CARTESIAN_POINT ( 'NONE',  ( -45.52287095715007581, -23.85229601348996198, 10.88205029486208986 ) ) ;
#16548 = CARTESIAN_POINT ( 'NONE',  ( -5.193715590271882121, 18.98282465337476665, -1.500000000000002220 ) ) ;
#16549 = FACE_OUTER_BOUND ( 'NONE', #63698, .T. ) ;
#16550 = CARTESIAN_POINT ( 'NONE',  ( -109.9698394925872549, -25.27925910355527250, 5.331473675041118021 ) ) ;
#16551 = APPROVAL_STATUS ( 'not_yet_approved' ) ;
#16552 = VECTOR ( 'NONE', #28174, 1000.000000000000000 ) ;
#16553 = EDGE_CURVE ( 'NONE', #80383, #25080, #25859, .T. ) ;
#16554 = CARTESIAN_POINT ( 'NONE',  ( -56.62287095715005592, -24.64965695001468404, 8.947790433994185832 ) ) ;
#16555 = CARTESIAN_POINT ( 'NONE',  ( 10.24059822343757808, -6.376774720514426953, 17.91871304725684766 ) ) ;
#16556 = CARTESIAN_POINT ( 'NONE',  ( -19.32567751138619982, -7.045664331180771178, 11.49999999999999645 ) ) ;
#16557 = CARTESIAN_POINT ( 'NONE',  ( -89.40841769935767047, -29.50249917535260380, 7.447779886225679213 ) ) ;
#16558 = AXIS2_PLACEMENT_3D ( 'NONE', #20801, #91322, #89831 ) ;
#16559 = ADVANCED_FACE ( 'NONE', ( #98299 ), #66984, .T. ) ;
#16560 = CARTESIAN_POINT ( 'NONE',  ( -120.6293614585003269, -23.48783264082477018, -1.443836473390085695 ) ) ;
#16561 = CARTESIAN_POINT ( 'NONE',  ( -16.68516988606489448, 15.22057433622007316, 11.49999999999999645 ) ) ;
#16562 = ORIENTED_EDGE ( 'NONE', *, *, #76438, .T. ) ;
#16563 =( LENGTH_UNIT ( ) NAMED_UNIT ( * ) SI_UNIT ( .MILLI., .METRE. ) );
#16564 = CARTESIAN_POINT ( 'NONE',  ( -99.82150581108260212, -25.31296402341794760, 4.513512821131813624 ) ) ;
#16565 = SPHERICAL_SURFACE ( 'NONE', #5672, 1.000000000000000000 ) ;
#16566 = CARTESIAN_POINT ( 'NONE',  ( -125.5896765834183810, -24.52399227489127043, 9.353111116836528183 ) ) ;
#16567 = CARTESIAN_POINT ( 'NONE',  ( 5.399550031316281640, 0.3587747205144061202, -28.54570968857217395 ) ) ;
#16568 = EDGE_CURVE ( 'NONE', #97920, #89739, #61769, .T. ) ;
#16569 = DIRECTION ( 'NONE',  ( 0.000000000000000000, 0.000000000000000000, 1.000000000000000000 ) ) ;
#16570 = CARTESIAN_POINT ( 'NONE',  ( -12.64432969575900323, -5.965225279485592225, -26.13179214487284696 ) ) ;
#16571 = ORIENTED_EDGE ( 'NONE', *, *, #36633, .F. ) ;
#16572 = VECTOR ( 'NONE', #34651, 1000.000000000000000 ) ;
#16573 = CARTESIAN_POINT ( 'NONE',  ( -79.38647268321243189, -25.31596371128505751, 5.652477663093335991 ) ) ;
#16574 = CARTESIAN_POINT ( 'NONE',  ( 4.317061085376620255, -22.40314112565372540, -1.500000000000002220 ) ) ;
#16575 = CARTESIAN_POINT ( 'NONE',  ( -74.64368143928086852, -23.73766607897670511, -1.055555164236458898 ) ) ;
#16576 = DIRECTION ( 'NONE',  ( 0.000000000000000000, 0.000000000000000000, 1.000000000000000000 ) ) ;
#16577 = DIRECTION ( 'NONE',  ( -0.000000000000000000, 2.173523156925979552E-06, -0.9999999999976378895 ) ) ;
#16578 = SECURITY_CLASSIFICATION ( '', '', #49655 ) ;
#16579 = CARTESIAN_POINT ( 'NONE',  ( 5.309366582633749054, -21.77581755331916824, 11.49999999999999645 ) ) ;
#16580 = EDGE_LOOP ( 'NONE', ( #27664, #19995, #85631, #98807 ) ) ;
#16581 = CARTESIAN_POINT ( 'NONE',  ( -43.52287095715006160, -23.47596703998600631, 11.44779298504229281 ) ) ;
#16582 = CARTESIAN_POINT ( 'NONE',  ( 21.83198049998918577, 2.282343850347359648, -1.500000000000002220 ) ) ;
#16583 = CARTESIAN_POINT ( 'NONE',  ( -5.837039262820512775, -6.376774720514415407, 19.76512419871795245 ) ) ;
#16584 = CARTESIAN_POINT ( 'NONE',  ( -34.62373385991148211, -24.66019654487199730, 8.947790411086117501 ) ) ;
#16585 = CARTESIAN_POINT ( 'NONE',  ( -121.5228709571500616, -23.72773821059536914, 11.05748984161097503 ) ) ;
#16586 = ORIENTED_EDGE ( 'NONE', *, *, #38069, .F. ) ;
#16587 = CARTESIAN_POINT ( 'NONE',  ( -48.59339690811989243, -24.15620529776627734, 10.23563542870660470 ) ) ;
#16588 = CARTESIAN_POINT ( 'NONE',  ( -112.5562042904833930, -24.66019654487199730, 8.947790411086124607 ) ) ;
#16589 = ORIENTED_EDGE ( 'NONE', *, *, #5547, .F. ) ;
#16590 = CARTESIAN_POINT ( 'NONE',  ( -12.04554601739387998, 16.56303510970703385, -1.500000000000002220 ) ) ;
#16591 = ORIENTED_EDGE ( 'NONE', *, *, #32363, .F. ) ;
#16592 = ORIENTED_EDGE ( 'NONE', *, *, #81296, .F. ) ;
#16594 = ORIENTED_EDGE ( 'NONE', *, *, #5912, .F. ) ;
#16593 = AXIS2_PLACEMENT_3D ( 'NONE', #98752, #98249, #20135 ) ;
#16595 = ORIENTED_EDGE ( 'NONE', *, *, #41703, .F. ) ;
#16596 = CARTESIAN_POINT ( 'NONE',  ( 11.92049557817732364, -19.74369927386287671, -1.500000000000002220 ) ) ;
#16597 = DIRECTION ( 'NONE',  ( -1.000000000000000000, -0.000000000000000000, -0.000000000000000000 ) ) ;
#16598 = CARTESIAN_POINT ( 'NONE',  ( -12.35269427871797987, -16.12754648828645543, -1.500000000000002220 ) ) ;
#16599 = ORIENTED_EDGE ( 'NONE', *, *, #7550, .T. ) ;
#16600 = LINE ( 'NONE', #86624, #29881 ) ;
#16601 = CARTESIAN_POINT ( 'NONE',  ( -37.58953762381672448, -23.48783264082477373, -1.443836473390072372 ) ) ;
#16602 = EDGE_CURVE ( 'NONE', #76130, #79877, #36916, .T. ) ;
#16603 = CARTESIAN_POINT ( 'NONE',  ( -46.52287095715006160, -24.65952944569304606, 1.056160979905693686 ) ) ;
#16604 = CARTESIAN_POINT ( 'NONE',  ( 4.214857194124448370, -5.876774720514403860, 18.65898740197609840 ) ) ;
#16606 = ORIENTED_EDGE ( 'NONE', *, *, #99793, .F. ) ;
#16605 = CARTESIAN_POINT ( 'NONE',  ( 20.90071823198991297, 5.034746273075951351, 11.49999999999999645 ) ) ;
#16607 = CARTESIAN_POINT ( 'NONE',  ( -89.52287095715006160, -24.64965694238407323, 8.947790433994196491 ) ) ;
#16608 = DIRECTION ( 'NONE',  ( 0.000000000000000000, 0.000000000000000000, 1.000000000000000000 ) ) ;
#16609 = ORIENTED_EDGE ( 'NONE', *, *, #9954, .T. ) ;
#16610 = CARTESIAN_POINT ( 'NONE',  ( 20.74337371777590278, 0.4424840333690017724, 11.49999999999998934 ) ) ;
#16612 = EDGE_CURVE ( 'NONE', #12412, #97853, #68373, .T. ) ;
#16611 = ORIENTED_EDGE ( 'NONE', *, *, #95259, .F. ) ;
#16614 = ORIENTED_EDGE ( 'NONE', *, *, #27249, .F. ) ;
#16613 = CARTESIAN_POINT ( 'NONE',  ( -125.5551874828237970, -24.40034930558991633, 0.3402023900116222244 ) ) ;
#16615 = ADVANCED_FACE ( 'NONE', ( #69868 ), #15073, .T. ) ;
#16616 = AXIS2_PLACEMENT_3D ( 'NONE', #46495, #63747, #46004 ) ;
#16617 = B_SPLINE_SURFACE_WITH_KNOTS ( 'NONE', 3, 1, ( 
 ( #56784, #25307 ),
 ( #24802, #56286 ),
 ( #18201, #55782 ),
 ( #87209, #2993 ),
 ( #87719, #17700 ),
 ( #17194, #79087 ),
 ( #64910, #95819 ),
 ( #26317, #20066 ),
 ( #59143, #16693 ),
 ( #51028, #47662 ),
 ( #48162, #9589 ),
 ( #71501, #78578 ),
 ( #9085, #40038 ),
 ( #82463, #5841 ),
 ( #92068, #68743 ) ),
 .UNSPECIFIED., .F., .F., .F.,
 ( 4, 1, 1, 1, 1, 1, 1, 1, 1, 1, 1, 1, 4 ),
 ( 2, 2 ),
 ( 0.000000000000000000, 0.09831997398134753596, 0.1994174736496688582, 0.3056025976021228274, 0.4161623563557467209, 0.4745823813143021375, 0.5370064812335182403, 0.6038573606499607616, 0.6740896076918744262, 0.7494169867637917593, 0.8282534808908113000, 0.9120541595560537340, 1.000000000000000000 ),
 ( 0.000000000000000000, 1.000000000000000000 ),
 .UNSPECIFIED. ) ;
#16618 = CARTESIAN_POINT ( 'NONE',  ( -75.62287095715007013, -24.51254535404255464, 9.355368623467656519 ) ) ;
#16619 = CARTESIAN_POINT ( 'NONE',  ( 14.76093561896379214, -5.965225279485572685, -26.55548769130089681 ) ) ;
#16620 = ORIENTED_EDGE ( 'NONE', *, *, #14770, .T. ) ;
#16621 = VERTEX_POINT ( 'NONE', #84084 ) ;
#16622 = CARTESIAN_POINT ( 'NONE',  ( -6.072964844751159497, -5.876774720514410077, 19.44316438561912008 ) ) ;
#16623 = B_SPLINE_CURVE_WITH_KNOTS ( 'NONE', 3,
 ( #95449, #19810, #3123, #12201 ),
 .UNSPECIFIED., .F., .F.,
 ( 4, 4 ),
 ( 0.000000000000000000, 9.999999999999592548E-05 ),
 .UNSPECIFIED. ) ;
#16624 = B_SPLINE_CURVE_WITH_KNOTS ( 'NONE', 3,
 ( #46077, #76996, #30839, #23212, #54197, #86626, #40960, #32339, #26233, #56704 ),
 .UNSPECIFIED., .F., .F.,
 ( 4, 2, 2, 2, 4 ),
 ( 0.000000000000000000, 0.0001827656628061555440, 0.0003655313256123110879, 0.0005482969884184666319, 0.0007310626512246221759 ),
 .UNSPECIFIED. ) ;
#16625 = DIRECTION ( 'NONE',  ( -0.000000000000000000, -1.000000000000000000, -0.000000000000000000 ) ) ;
#16626 = B_SPLINE_CURVE_WITH_KNOTS ( 'NONE', 3,
 ( #7976, #38927, #62282, #54667 ),
 .UNSPECIFIED., .F., .F.,
 ( 4, 4 ),
 ( 0.000000000000000000, 9.999999999998897304E-05 ),
 .UNSPECIFIED. ) ;
#16627 = CARTESIAN_POINT ( 'NONE',  ( -43.48232127904228150, -24.66019654487199375, 8.947790411086122830 ) ) ;
#16628 = CARTESIAN_POINT ( 'NONE',  ( -7.807709442696729063, 20.60712426125841645, 11.49999999999999645 ) ) ;
#16629 = DIRECTION ( 'NONE',  ( 0.000000000000000000, 1.000000000000000000, -0.000000000000000000 ) ) ;
#16630 = CARTESIAN_POINT ( 'NONE',  ( 7.090404290683943067, 21.45231405096426514, -1.500000000000002220 ) ) ;
#16631 = CARTESIAN_POINT ( 'NONE',  ( 18.73254098450790295, -9.497730595714260815, 11.49999999999998934 ) ) ;
#16632 = DIRECTION ( 'NONE',  ( 0.000000000000000000, -1.000000000000000000, 0.000000000000000000 ) ) ;
#16634 = VERTEX_POINT ( 'NONE', #23169 ) ;
#16633 = CARTESIAN_POINT ( 'NONE',  ( -99.38771510255533315, -25.29141603707036268, 5.771832689820707962 ) ) ;
#16635 = CIRCLE ( 'NONE', #52280, 0.3000000000000016542 ) ;
#16636 = VERTEX_POINT ( 'NONE', #69365 ) ;
#16637 = CARTESIAN_POINT ( 'NONE',  ( 5.717289507243529023, -5.356774720514425603, -25.39219853617311173 ) ) ;
#16638 = EDGE_CURVE ( 'NONE', #66356, #74013, #60741, .T. ) ;
#16639 = CARTESIAN_POINT ( 'NONE',  ( 4.967948717948723392, -6.376774720514415407, 20.00140224358974095 ) ) ;
#16640 = VERTEX_POINT ( 'NONE', #76962 ) ;
#16641 = CARTESIAN_POINT ( 'NONE',  ( 17.61891135320703938, 11.69080507458975227, 11.49999999999998934 ) ) ;
#16642 = CARTESIAN_POINT ( 'NONE',  ( 8.971512145086499856, -1.028487854913500810, 3.750000000000000000 ) ) ;
#16643 = CARTESIAN_POINT ( 'NONE',  ( -59.79060349298165278, -25.33009847151394922, 4.495758292450050320 ) ) ;
#16644 = CARTESIAN_POINT ( 'NONE',  ( -121.5915913388690370, -23.73766607897670156, -1.055555164236450905 ) ) ;
#16645 = B_SPLINE_CURVE_WITH_KNOTS ( 'NONE', 3,
 ( #82360, #12839, #43808, #56318, #68640, #52921 ),
 .UNSPECIFIED., .F., .F.,
 ( 4, 2, 4 ),
 ( 6.384118694780321315E-06, 0.001386860460836456411, 0.002767336802978132785 ),
 .UNSPECIFIED. ) ;
#16646 = PLANE ( 'NONE',  #10302 ) ;
#16647 = CARTESIAN_POINT ( 'NONE',  ( -80.62287095715005592, -23.47593901973091235, -1.443836447539004642 ) ) ;
#16648 = CARTESIAN_POINT ( 'NONE',  ( 14.93699691249320693, 16.48547057857716425, -1.500000000000002220 ) ) ;
#16649 = CARTESIAN_POINT ( 'NONE',  ( -114.5520207083192332, -24.51314013834316086, 0.6176544820404251679 ) ) ;
#16650 = ORIENTED_EDGE ( 'NONE', *, *, #42949, .T. ) ;
#16651 = CARTESIAN_POINT ( 'NONE',  ( -23.71328795744024021, 5.965225279485594001, -17.58350715675015152 ) ) ;
#16652 = LINE ( 'NONE', #2445, #28159 ) ;
#16653 = FACE_OUTER_BOUND ( 'NONE', #78271, .T. ) ;
#16654 = ADVANCED_FACE ( 'NONE', ( #91690 ), #52645, .T. ) ;
#16655 = CARTESIAN_POINT ( 'NONE',  ( 6.184520403203631389, 5.356774720514425603, -25.32021290018218451 ) ) ;
#16656 = DIRECTION ( 'NONE',  ( -3.773278334453079618E-23, 0.9999999999976377785, 2.173523156925979975E-06 ) ) ;
#16657 = VECTOR ( 'NONE', #14024, 1000.000000000000000 ) ;
#16658 = CARTESIAN_POINT ( 'NONE',  ( -19.16120753946698585, -3.443109951913609024, 11.49999999999998934 ) ) ;
#16659 = EDGE_CURVE ( 'NONE', #30745, #77700, #75963, .T. ) ;
#16660 = LOCAL_TIME ( 0, 54, 15.00000000000000000, #76451 ) ;
#16661 = CARTESIAN_POINT ( 'NONE',  ( -20.93543047832761417, 4.563121699532205255, -1.500000000000002220 ) ) ;
#16662 = LINE ( 'NONE', #57258, #70952 ) ;
#16663 = FACE_OUTER_BOUND ( 'NONE', #31196, .T. ) ;
#16664 = LINE ( 'NONE', #23774, #64950 ) ;
#16665 = CARTESIAN_POINT ( 'NONE',  ( -101.3340698065965455, -25.18440142138669202, 3.896482854220133518 ) ) ;
#16666 = CARTESIAN_POINT ( 'NONE',  ( 22.70222466501550329, 0.2752559529566028229, -1.500000000000002220 ) ) ;
#16667 = CIRCLE ( 'NONE', #99305, 4.450000000000000178 ) ;
#16668 = DIRECTION ( 'NONE',  ( -1.000000000000000000, -3.773278334444167608E-23, -8.201307833595939069E-29 ) ) ;
#16669 = PLANE ( 'NONE',  #70263 ) ;
#16670 = CARTESIAN_POINT ( 'NONE',  ( 18.55763160240848109, 7.024834138330111166, 11.49999999999999645 ) ) ;
#16671 = CARTESIAN_POINT ( 'NONE',  ( -123.5557599765402159, -23.96169478059714564, 10.65365249895717170 ) ) ;
#16672 = AXIS2_PLACEMENT_3D ( 'NONE', #89637, #98230, #12997 ) ;
#16673 = CARTESIAN_POINT ( 'NONE',  ( -108.6228709571500417, -23.48786465467242479, 11.44779295918253759 ) ) ;
#16674 = CARTESIAN_POINT ( 'NONE',  ( -127.5228709571500616, -23.47596703998600631, 11.44779298504227683 ) ) ;
#16675 = EDGE_CURVE ( 'NONE', #23980, #82488, #7455, .T. ) ;
#16676 = ORIENTED_EDGE ( 'NONE', *, *, #44419, .F. ) ;
#16677 = PLANE ( 'NONE',  #75241 ) ;
#16678 = LINE ( 'NONE', #69968, #81490 ) ;
#16679 = CARTESIAN_POINT ( 'NONE',  ( -51.69862270353959843, -25.27412468278110325, 3.939198053822961398 ) ) ;
#16680 = CARTESIAN_POINT ( 'NONE',  ( -20.56447267657262401, 6.860157381912782348, -1.500000000000002220 ) ) ;
#16681 = CARTESIAN_POINT ( 'NONE',  ( -56.49719084987101070, -24.35071581493543391, 9.817618358456030592 ) ) ;
#16682 = CARTESIAN_POINT ( 'NONE',  ( -19.06185424839875964, 3.971334347869299286, -1.500000000000002220 ) ) ;
#16683 = PLANE ( 'NONE',  #74962 ) ;
#16684 = ORIENTED_EDGE ( 'NONE', *, *, #48997, .T. ) ;
#16685 = CARTESIAN_POINT ( 'NONE',  ( -6.692510123977180925, 19.25193956699996178, 11.49999999999999645 ) ) ;
#16686 = CARTESIAN_POINT ( 'NONE',  ( 6.026637739148365548E-17, -29.50250786944496539, 11.44777975102276635 ) ) ;
#16687 = ADVANCED_FACE ( 'NONE', ( #15569 ), #45540, .T. ) ;
#16688 = CARTESIAN_POINT ( 'NONE',  ( -95.52287095715006160, -29.50247984919015209, -1.443849546365050029 ) ) ;
#16689 = EDGE_CURVE ( 'NONE', #76909, #83981, #85583, .T. ) ;
#16690 = ORIENTED_EDGE ( 'NONE', *, *, #99789, .T. ) ;
#16691 = LINE ( 'NONE', #47660, #45925 ) ;
#16692 = FACE_OUTER_BOUND ( 'NONE', #98289, .T. ) ;
#16693 = CARTESIAN_POINT ( 'NONE',  ( -39.26664729043937996, -25.27985447715197509, 5.049946080353571176 ) ) ;
#16694 = CARTESIAN_POINT ( 'NONE',  ( -40.62378914844666156, -25.00182538069146787, 7.747789668545040698 ) ) ;
#16695 = CARTESIAN_POINT ( 'NONE',  ( -0.4362980769230789257, -5.876774720514411854, 19.46153846153846345 ) ) ;
#16696 = CARTESIAN_POINT ( 'NONE',  ( 19.67429046578372365, -4.105084037421226739, 11.49999999999998934 ) ) ;
#16697 = EDGE_CURVE ( 'NONE', #63151, #66316, #32301, .T. ) ;
#16698 = CARTESIAN_POINT ( 'NONE',  ( -109.5201659922639550, -23.73766607897670156, -1.055555164236452903 ) ) ;
#16699 = AXIS2_PLACEMENT_3D ( 'NONE', #46207, #77140, #6640 ) ;
#16700 = ORIENTED_EDGE ( 'NONE', *, *, #92289, .F. ) ;
#16701 = CARTESIAN_POINT ( 'NONE',  ( -66.60300861680383377, -23.73791477778911840, 11.05961554403170766 ) ) ;
#16702 = EDGE_CURVE ( 'NONE', #7274, #20892, #14877, .T. ) ;
#16703 = CARTESIAN_POINT ( 'NONE',  ( -22.92702450682246251, 0.3551139841105944162, 11.49999999999999645 ) ) ;
#16704 = CARTESIAN_POINT ( 'NONE',  ( -18.45961786539058380, -13.25243217869837231, -1.500000000000002220 ) ) ;
#16705 = ORIENTED_EDGE ( 'NONE', *, *, #96172, .T. ) ;
#16706 = CARTESIAN_POINT ( 'NONE',  ( -30.47287095715007510, -24.38330924582771786, 9.665504117595752120 ) ) ;
#16707 = B_SPLINE_CURVE_WITH_KNOTS ( 'NONE', 3,
 ( #46792, #31050, #86353, #87347 ),
 .UNSPECIFIED., .F., .F.,
 ( 4, 4 ),
 ( 0.000000000000000000, 0.0001000000000000028644 ),
 .UNSPECIFIED. ) ;
#16708 = VECTOR ( 'NONE', #845, 1000.000000000000000 ) ;
#16709 = CARTESIAN_POINT ( 'NONE',  ( -91.55620429048340725, -23.48786465467241769, 11.44779295918253936 ) ) ;
#16710 = CARTESIAN_POINT ( 'NONE',  ( -38.56989630778316780, -23.48786465467240347, 11.44779295918255002 ) ) ;
#16711 = CARTESIAN_POINT ( 'NONE',  ( -112.5228709571500616, -23.48786465467241769, 11.44779295918253936 ) ) ;
#16712 = CARTESIAN_POINT ( 'NONE',  ( 32.45853543194704116, -0.3587747205144265483, 9.169203677920338080 ) ) ;
#16713 = CARTESIAN_POINT ( 'NONE',  ( -55.62287095715004170, -29.50249982740957577, 7.747779886224967605 ) ) ;
#16714 = CARTESIAN_POINT ( 'NONE',  ( -79.34687923781920915, -29.50249594249816099, 5.960400078536885360 ) ) ;
#16715 = ORIENTED_EDGE ( 'NONE', *, *, #464, .F. ) ;
#16716 = CARTESIAN_POINT ( 'NONE',  ( 17.64890103348723116, 10.21726211432410203, 11.49999999999998934 ) ) ;
#16717 = ORIENTED_EDGE ( 'NONE', *, *, #1100, .T. ) ;
#16718 = CARTESIAN_POINT ( 'NONE',  ( -15.63304604236160067, -16.83380969201049382, -1.500000000000002220 ) ) ;
#16719 = CARTESIAN_POINT ( 'NONE',  ( -1.304987980769231948, -6.376774720514413630, 19.76512419871795245 ) ) ;
#16720 = ORIENTED_EDGE ( 'NONE', *, *, #84712, .T. ) ;
#16721 = PLANE ( 'NONE',  #37997 ) ;
#16722 = CIRCLE ( 'NONE', #94447, 1.836000000000000743 ) ;
#16723 = EDGE_CURVE ( 'NONE', #3684, #82958, #49046, .T. ) ;
#16724 = FACE_OUTER_BOUND ( 'NONE', #11469, .T. ) ;
#16726 = ORIENTED_EDGE ( 'NONE', *, *, #19463, .T. ) ;
#16725 = CARTESIAN_POINT ( 'NONE',  ( -18.83571791729191958, -9.990160686573538840, 11.49999999999999645 ) ) ;
#16727 = VERTEX_POINT ( 'NONE', #63276 ) ;
#16728 = CARTESIAN_POINT ( 'NONE',  ( 6.060481786824854389, 21.40074245971799627, -1.500000000000002220 ) ) ;
#16729 = CARTESIAN_POINT ( 'NONE',  ( -3.285303218690974525, -20.39892020120133154, 11.49999999999998934 ) ) ;
#16731 = VERTEX_POINT ( 'NONE', #11828 ) ;
#16730 = AXIS2_PLACEMENT_3D ( 'NONE', #40284, #33672, #49414 ) ;
#16732 = ADVANCED_FACE ( 'NONE', ( #17576 ), #54651, .F. ) ;
#16733 = CARTESIAN_POINT ( 'NONE',  ( -4.620655831143558601, -6.376774720514410077, 19.21747685089457036 ) ) ;
#16734 = CARTESIAN_POINT ( 'NONE',  ( -68.92123217116099454, -25.31392322340849432, 5.203679841770401104 ) ) ;
#16735 = ORIENTED_EDGE ( 'NONE', *, *, #20038, .F. ) ;
#16736 = CARTESIAN_POINT ( 'NONE',  ( 0.000000000000000000, -4.056774720514426669, 4.299999999999999822 ) ) ;
#16737 = ORIENTED_EDGE ( 'NONE', *, *, #52560, .T. ) ;
#16738 = AXIS2_PLACEMENT_3D ( 'NONE', #47867, #86416, #77782 ) ;
#16739 = CARTESIAN_POINT ( 'NONE',  ( -58.49328643788003745, -24.51419770103156637, 9.386484678747176957 ) ) ;
#16740 = CARTESIAN_POINT ( 'NONE',  ( 3.889286922045745776, 20.52237432693057073, -1.500000000000002220 ) ) ;
#16741 = CARTESIAN_POINT ( 'NONE',  ( 8.176594470695947692, -20.27425322898990601, 11.49999999999999645 ) ) ;
#16742 = CARTESIAN_POINT ( 'NONE',  ( 25.30723783573411012, -5.176466091202484243, -8.329609793420479136 ) ) ;
#16743 = CARTESIAN_POINT ( 'NONE',  ( 5.088854283150510582, -3.311779300275201177, -27.56292346345011524 ) ) ;
#16744 = CARTESIAN_POINT ( 'NONE',  ( 17.87336509531889561, -13.68139028912531785, 11.49999999999998934 ) ) ;
#16745 = CARTESIAN_POINT ( 'NONE',  ( -118.5530091436460509, -24.51419770103160189, 9.386484678747169852 ) ) ;
#16746 = CARTESIAN_POINT ( 'NONE',  ( -57.62287095715005592, -23.94994826722515313, -0.6494450866351703100 ) ) ;
#16747 = DIRECTION ( 'NONE',  ( -0.000000000000000000, 1.000000000000000000, -0.000000000000000000 ) ) ;
#16748 = ORIENTED_EDGE ( 'NONE', *, *, #51155, .T. ) ;
#16749 = B_SPLINE_SURFACE_WITH_KNOTS ( 'NONE', 3, 1, ( 
 ( #80940, #43387 ),
 ( #50006, #97654 ),
 ( #44382, #34274 ),
 ( #96658, #11426 ),
 ( #42401, #89551 ),
 ( #74325, #19529 ),
 ( #65246, #20035 ),
 ( #4816, #66739 ),
 ( #90050, #51491 ),
 ( #60614, #21513 ),
 ( #68212, #31132 ),
 ( #30637, #92035 ),
 ( #22008, #53499 ),
 ( #77298, #84424 ),
 ( #23503, #15904 ),
 ( #83926, #45874 ),
 ( #37754, #91536 ),
 ( #76792, #60115 ),
 ( #76300, #30133 ),
 ( #69711, #85420 ),
 ( #52491, #83419 ),
 ( #7293, #190 ),
 ( #54482, #75308 ),
 ( #62105, #98642 ),
 ( #36762, #93026 ),
 ( #14406, #52995 ),
 ( #5805, #6796 ) ),
 .UNSPECIFIED., .F., .F., .F.,
 ( 4, 1, 1, 1, 1, 1, 1, 1, 1, 1, 1, 1, 1, 1, 1, 1, 1, 1, 1, 1, 1, 1, 1, 1, 4 ),
 ( 2, 2 ),
 ( 0.000000000000000000, 0.06527777045992599891, 0.1272054409606112602, 0.1861682170588502272, 0.2416754997382695169, 0.2941145050635431968, 0.3436091886235829174, 0.3903870759341810937, 0.4344634103958515681, 0.4766455533866958971, 0.5170022931272251210, 0.5559361803014920556, 0.5937164392999396689, 0.6300571764906928163, 0.6656014334950210998, 0.7007446912418848761, 0.7349167217326266766, 0.7686809964330385547, 0.8020868126442075585, 0.8348488267452134348, 0.8674333878737416903, 0.9001375891431748766, 0.9328060676261197282, 0.9662118838372896201, 1.000000000000000000 ),
 ( 0.000000000000000000, 1.000000000000000000 ),
 .UNSPECIFIED. ) ;
#16750 = VERTEX_POINT ( 'NONE', #48548 ) ;
#16751 = ORIENTED_EDGE ( 'NONE', *, *, #23061, .T. ) ;
#16752 = EDGE_LOOP ( 'NONE', ( #12009, #25635, #87042, #95479 ) ) ;
#16753 = ADVANCED_FACE ( 'NONE', ( #8963 ), #70367, .F. ) ;
#16754 = CARTESIAN_POINT ( 'NONE',  ( 6.831138157384286203, 20.27010762675863731, -1.500000000000002220 ) ) ;
#16755 = CARTESIAN_POINT ( 'NONE',  ( 14.50327815619135308, -17.01817589256642194, 11.49999999999999645 ) ) ;
#16756 = ORIENTED_EDGE ( 'NONE', *, *, #67096, .F. ) ;
#16757 = CARTESIAN_POINT ( 'NONE',  ( -5.931750313267273533, -20.21149935180699231, -1.500000000000002220 ) ) ;
#16758 = CARTESIAN_POINT ( 'NONE',  ( -61.58953762381672448, -23.47593901973091235, -1.443836447539007972 ) ) ;
#16759 = CARTESIAN_POINT ( 'NONE',  ( -19.95465934538571062, -0.7993260556091378310, -1.500000000000002220 ) ) ;
#16760 = APPLICATION_CONTEXT ( 'configuration controlled 3d designs of mechanical parts and assemblies' ) ;
#16761 =( BOUNDED_CURVE ( )  B_SPLINE_CURVE ( 3, ( #32396, #33386, #49141, #64879 ),
 .UNSPECIFIED., .F., .F. ) 
 B_SPLINE_CURVE_WITH_KNOTS ( ( 4, 4 ),
 ( 4.712388980384689674, 4.821597757366586912 ),
 .UNSPECIFIED. ) 
 CURVE ( )  GEOMETRIC_REPRESENTATION_ITEM ( )  RATIONAL_B_SPLINE_CURVE ( ( 1.000000000000000000, 0.9990063671772055898, 0.9990063671772055898, 1.000000000000000000 ) ) 
 REPRESENTATION_ITEM ( '' )  );
#16762 = CARTESIAN_POINT ( 'NONE',  ( -117.6228709571500701, -24.34917612406838217, 0.1852690917426713935 ) ) ;
#16763 = CARTESIAN_POINT ( 'NONE',  ( 2.911360383046243783, -5.876774720514417183, 20.24673073119071276 ) ) ;
#16764 = CARTESIAN_POINT ( 'NONE',  ( -5.411813039392390223, -21.34095290059367755, -1.500000000000002220 ) ) ;
#16765 = DIRECTION ( 'NONE',  ( -0.04171448572128191867, 0.5400267985901394674, -0.8406134417706475626 ) ) ;
#16766 = VERTEX_POINT ( 'NONE', #94699 ) ;
#16767 = DIRECTION ( 'NONE',  ( -0.9975640502598241977, 0.06975647374412534407, 3.469446951953616654E-16 ) ) ;
#16768 = VECTOR ( 'NONE', #58967, 1000.000000000000114 ) ;
#16769 = EDGE_CURVE ( 'NONE', #36724, #49066, #86655, .T. ) ;
#16770 = CARTESIAN_POINT ( 'NONE',  ( -127.5562042904833646, -23.47596703998600631, 11.44779298504227683 ) ) ;
#16771 = CARTESIAN_POINT ( 'NONE',  ( -18.54028579900546703, -9.471972883075929772, 11.49999999999999645 ) ) ;
#16772 = EDGE_CURVE ( 'NONE', #27358, #93569, #39912, .T. ) ;
#16773 = EDGE_CURVE ( 'NONE', #72803, #41185, #79049, .T. ) ;
#16774 = CARTESIAN_POINT ( 'NONE',  ( 24.50102500000003758, -9.528487854913448629, 4.028342098511015491E-15 ) ) ;
#16775 = B_SPLINE_CURVE_WITH_KNOTS ( 'NONE', 3,
 ( #21031, #81457, #42899, #35286 ),
 .UNSPECIFIED., .F., .F.,
 ( 4, 4 ),
 ( 0.000000000000000000, 0.0001000000000000028644 ),
 .UNSPECIFIED. ) ;
#16776 = VECTOR ( 'NONE', #53738, 1000.000000000000114 ) ;
#16777 = PLANE ( 'NONE',  #3634 ) ;
#16778 = EDGE_CURVE ( 'NONE', #41074, #72641, #51202, .T. ) ;
#16779 = DIRECTION ( 'NONE',  ( 0.000000000000000000, 0.000000000000000000, -1.000000000000000000 ) ) ;
#16780 = CARTESIAN_POINT ( 'NONE',  ( -16.81368161134402683, 13.12552177539105358, -1.500000000000002220 ) ) ;
#16781 = CARTESIAN_POINT ( 'NONE',  ( -29.52287095715006160, -24.56627961951908645, 8.947790480023282811 ) ) ;
#16782 = CARTESIAN_POINT ( 'NONE',  ( -3.212051231530180573, 17.72614232434105119, -9.000000000000000000 ) ) ;
#16783 = PLANE ( 'NONE',  #94026 ) ;
#16784 = DIRECTION ( 'NONE',  ( -0.000000000000000000, 1.000000000000000000, -0.000000000000000000 ) ) ;
#16785 = CARTESIAN_POINT ( 'NONE',  ( -22.36795837939145670, 2.692536522722862813, -1.500000000000002220 ) ) ;
#16786 = DIRECTION ( 'NONE',  ( -1.000000000000000000, -0.000000000000000000, -0.000000000000000000 ) ) ;
#16787 = VERTEX_POINT ( 'NONE', #48038 ) ;
#16788 = CARTESIAN_POINT ( 'NONE',  ( -80.26338284007071877, -25.29550791665888454, 4.507555199503806342 ) ) ;
#16789 = LINE ( 'NONE', #63495, #24916 ) ;
#16790 = CARTESIAN_POINT ( 'NONE',  ( -0.7274468246531539117, 19.66889477801398911, 11.49999999999999645 ) ) ;
#16791 = CARTESIAN_POINT ( 'NONE',  ( -41.52287095715006870, -23.47593901973090169, -1.443836447538997092 ) ) ;
#16792 = CARTESIAN_POINT ( 'NONE',  ( -32.52287095715003318, -24.66019654487198665, 8.947790411086131712 ) ) ;
#16793 = ADVANCED_FACE ( 'NONE', ( #64282 ), #16565, .T. ) ;
#16794 = ADVANCED_FACE ( 'NONE', ( #95206 ), #40422, .F. ) ;
#16795 = VERTEX_POINT ( 'NONE', #43296 ) ;
#16796 = CARTESIAN_POINT ( 'NONE',  ( 30.43908124610669930, -1.684774720514424784, -13.86910542224429044 ) ) ;
#16797 = CARTESIAN_POINT ( 'NONE',  ( -19.69812919673063689, 5.965225279485592225, -22.00173861453435720 ) ) ;
#16798 = CYLINDRICAL_SURFACE ( 'NONE', #22282, 1.000000000000000000 ) ;
#16799 = DIRECTION ( 'NONE',  ( 0.000000000000000000, 1.000000000000000000, 0.000000000000000000 ) ) ;
#16800 = B_SPLINE_CURVE_WITH_KNOTS ( 'NONE', 3,
 ( #24659, #71357, #25672, #8946 ),
 .UNSPECIFIED., .F., .F.,
 ( 4, 4 ),
 ( 0.000000000000000000, 1.000000000000000000 ),
 .UNSPECIFIED. ) ;
#16801 = CARTESIAN_POINT ( 'NONE',  ( 6.816645498261984848, 18.52099371530728789, -1.500000000000002220 ) ) ;
#16802 = ORIENTED_EDGE ( 'NONE', *, *, #75734, .T. ) ;
#16803 = CARTESIAN_POINT ( 'NONE',  ( 14.48468284575590204, 14.13777120147990729, 11.49999999999999645 ) ) ;
#16804 = CARTESIAN_POINT ( 'NONE',  ( -110.0285167521317788, -25.20072809708166517, 3.334473250954808954 ) ) ;
#16805 = EDGE_CURVE ( 'NONE', #69709, #79287, #90452, .T. ) ;
#16806 = VECTOR ( 'NONE', #27784, 1000.000000000000000 ) ;
#16807 = APPROVAL_STATUS ( 'not_yet_approved' ) ;
#16808 = ORIENTED_EDGE ( 'NONE', *, *, #37515, .F. ) ;
#16809 = CARTESIAN_POINT ( 'NONE',  ( -67.62287095715012697, -23.96127896941632685, -0.6493128931037859264 ) ) ;
#16810 = CARTESIAN_POINT ( 'NONE',  ( -80.51758134885872664, -25.30554031725500508, 4.968846701839494173 ) ) ;
#16811 = CARTESIAN_POINT ( 'NONE',  ( -51.36075006403625309, -25.28866304528649067, 5.655890479381174174 ) ) ;
#16812 = CARTESIAN_POINT ( 'NONE',  ( -67.62287095715005592, -24.64898659630367916, 1.056161002820824368 ) ) ;
#16813 = CARTESIAN_POINT ( 'NONE',  ( -58.62287095715004881, -23.47593901973091235, -1.443836447539007972 ) ) ;
#16814 = AXIS2_PLACEMENT_3D ( 'NONE', #47133, #63374, #78050 ) ;
#16815 = CARTESIAN_POINT ( 'NONE',  ( -120.6228709571500417, -29.50250243563736774, 8.947779886222134493 ) ) ;
#16816 = CARTESIAN_POINT ( 'NONE',  ( 14.90458806734895703, -13.33898509196910886, 11.49999999999998934 ) ) ;
#16817 = EDGE_CURVE ( 'NONE', #42155, #79844, #18478, .T. ) ;
#16818 = CARTESIAN_POINT ( 'NONE',  ( 14.76093561896379214, 3.316774720514426456, -28.39148769130088468 ) ) ;
#16819 = DIRECTION ( 'NONE',  ( 4.218136541796977197E-15, 1.000000000000000000, 1.324960360541890271E-16 ) ) ;
#16820 = ORIENTED_EDGE ( 'NONE', *, *, #11089, .T. ) ;
#16821 = EDGE_CURVE ( 'NONE', #49884, #31511, #98551, .T. ) ;
#16822 = EDGE_CURVE ( 'NONE', #11930, #69195, #44010, .T. ) ;
#16823 = CARTESIAN_POINT ( 'NONE',  ( -38.62287095715005592, -29.50248528299804818, 1.056150453629031594 ) ) ;
#16824 = CARTESIAN_POINT ( 'NONE',  ( -109.8707484289256655, -25.18430176427498779, 3.397982113237853596 ) ) ;
#16825 = CARTESIAN_POINT ( 'NONE',  ( -23.59123376470063960, -6.143225279485574397, 24.50402280011862288 ) ) ;
#16826 = CARTESIAN_POINT ( 'NONE',  ( -82.62287095715005592, -24.64965695001468404, 8.947790433994182280 ) ) ;
#16827 = CARTESIAN_POINT ( 'NONE',  ( 22.65031661608483660, -500000.0000000000582, -20.71116937900383093 ) ) ;
#16828 = LINE ( 'NONE', #55914, #87483 ) ;
#16829 = DIRECTION ( 'NONE',  ( 0.000000000000000000, -1.000000000000000000, 0.000000000000000000 ) ) ;
#16830 = ADVANCED_FACE ( 'NONE', ( #5715 ), #13314, .T. ) ;
#16831 = CARTESIAN_POINT ( 'NONE',  ( -101.9695858942169480, -25.20650842489795807, 6.812665538484691474 ) ) ;
#16832 = ORIENTED_EDGE ( 'NONE', *, *, #92599, .T. ) ;
#16833 = B_SPLINE_CURVE_WITH_KNOTS ( 'NONE', 3,
 ( #60984, #69081, #14285, #77678 ),
 .UNSPECIFIED., .F., .F.,
 ( 4, 4 ),
 ( 0.000000000000000000, 1.000000000000000000 ),
 .UNSPECIFIED. ) ;
#16834 = CARTESIAN_POINT ( 'NONE',  ( -12.35269427871797987, -16.12754648828645543, 11.49999999999998934 ) ) ;
#16835 = DIRECTION ( 'NONE',  ( 0.000000000000000000, 0.000000000000000000, 1.000000000000000000 ) ) ;
#16836 = AXIS2_PLACEMENT_3D ( 'NONE', #32561, #47797, #40184 ) ;
#16837 = DIRECTION ( 'NONE',  ( -3.773278334444166432E-23, 1.000000000000000000, 0.000000000000000000 ) ) ;
#16838 = VERTEX_POINT ( 'NONE', #83835 ) ;
#16839 = FACE_OUTER_BOUND ( 'NONE', #32191, .T. ) ;
#16840 = CARTESIAN_POINT ( 'NONE',  ( -14.30055291515510518, -14.21740073472259525, -1.500000000000002220 ) ) ;
#16841 = B_SPLINE_CURVE_WITH_KNOTS ( 'NONE', 3,
 ( #15976, #46947, #24592, #39321 ),
 .UNSPECIFIED., .F., .F.,
 ( 4, 4 ),
 ( 1.387778780781445676E-17, 0.0001000000000000028508 ),
 .UNSPECIFIED. ) ;
#16842 = TOROIDAL_SURFACE ( 'NONE', #73576, 253.2618649670780826, 0.8159999999999999476 ) ;
#16843 = CARTESIAN_POINT ( 'NONE',  ( 1.812468502196824760, -21.08352789287561180, 11.49999999999999645 ) ) ;
#16844 = CARTESIAN_POINT ( 'NONE',  ( -4.315754209668272168, 21.71352930684897942, 11.49999999999998934 ) ) ;
#16845 = B_SPLINE_CURVE_WITH_KNOTS ( 'NONE', 3,
 ( #82921, #75311, #43880, #13411, #44384, #5308 ),
 .UNSPECIFIED., .F., .F.,
 ( 4, 2, 4 ),
 ( 0.000000000000000000, 0.001380901958385383774, 0.002761803916770767548 ),
 .UNSPECIFIED. ) ;
#16846 = CARTESIAN_POINT ( 'NONE',  ( -15.41819309731374510, 13.62919173607049927, -1.500000000000002220 ) ) ;
#16847 = CARTESIAN_POINT ( 'NONE',  ( 6.996935307331598075, -5.876774720514423400, 21.22729008382901128 ) ) ;
#16848 = ORIENTED_EDGE ( 'NONE', *, *, #57124, .F. ) ;
#16849 = CARTESIAN_POINT ( 'NONE',  ( -43.52287095715008292, -24.33832256527048088, 0.1851278514138565978 ) ) ;
#16850 = VERTEX_POINT ( 'NONE', #50905 ) ;
#16851 = CARTESIAN_POINT ( 'NONE',  ( -88.55620429048337883, -24.64965694238574656, 8.947790433994196491 ) ) ;
#16852 = FACE_OUTER_BOUND ( 'NONE', #62831, .T. ) ;
#16853 = ORIENTED_EDGE ( 'NONE', *, *, #67457, .F. ) ;
#16854 = EDGE_LOOP ( 'NONE', ( #45320, #71936, #76537, #79815 ) ) ;
#16855 = ORIENTED_EDGE ( 'NONE', *, *, #24341, .T. ) ;
#16856 = CARTESIAN_POINT ( 'NONE',  ( -111.2942365085818039, -25.18155215388633650, 3.200086650108997510 ) ) ;
#16857 = CARTESIAN_POINT ( 'NONE',  ( 6.509931258083027750, -6.376774720514417183, 20.09204137875607188 ) ) ;
#16858 = CARTESIAN_POINT ( 'NONE',  ( -96.62287095715004170, -24.65952944569304606, 1.056160979905703456 ) ) ;
#16859 = CARTESIAN_POINT ( 'NONE',  ( 0.1934390699377774303, 20.68474938276070318, -1.500000000000002220 ) ) ;
#16860 = CARTESIAN_POINT ( 'NONE',  ( 21.43499300031224664, 3.042053824063517542, 11.49999999999999645 ) ) ;
#16861 = VERTEX_POINT ( 'NONE', #67141 ) ;
#16862 = DIRECTION ( 'NONE',  ( 0.000000000000000000, -0.000000000000000000, -1.000000000000000000 ) ) ;
#16863 = CARTESIAN_POINT ( 'NONE',  ( -29.62287095715004881, -24.58390616985635546, 1.056161279468100123 ) ) ;
#16864 = CARTESIAN_POINT ( 'NONE',  ( 0.3464652362752086434, -22.36268665536068667, 11.49999999999998934 ) ) ;
#16865 = CARTESIAN_POINT ( 'NONE',  ( -71.52287095715011844, -24.51283580621365132, 0.6167428607019708187 ) ) ;
#16866 = CARTESIAN_POINT ( 'NONE',  ( -84.54196537793758637, -24.65952944569303895, 1.056160979905700348 ) ) ;
#16867 = ORIENTED_EDGE ( 'NONE', *, *, #77071, .T. ) ;
#16868 = CARTESIAN_POINT ( 'NONE',  ( -100.6181544063395989, -25.31264993464104407, 4.735175672904627930 ) ) ;
#16869 = CARTESIAN_POINT ( 'NONE',  ( -114.5228709571500616, -23.48786465467241769, 11.44779295918253936 ) ) ;
#16870 = ORIENTED_EDGE ( 'NONE', *, *, #11842, .F. ) ;
#16871 = VERTEX_POINT ( 'NONE', #45286 ) ;
#16872 = LINE ( 'NONE', #15868, #74967 ) ;
#16873 = EDGE_LOOP ( 'NONE', ( #90493, #85537, #93415, #67067 ) ) ;
#16874 = FACE_OUTER_BOUND ( 'NONE', #28540, .T. ) ;
#16875 = ADVANCED_FACE ( 'NONE', ( #37167 ), #59022, .T. ) ;
#16876 = CARTESIAN_POINT ( 'NONE',  ( 16.87399902462237478, -12.92443306546820736, -1.500000000000002220 ) ) ;
#16877 = VERTEX_POINT ( 'NONE', #36175 ) ;
#16878 = CARTESIAN_POINT ( 'NONE',  ( -50.57412005914952147, -25.00158670708910691, 2.256160236439223254 ) ) ;
#16879 = EDGE_CURVE ( 'NONE', #85245, #79246, #14312, .T. ) ;
#16880 = CARTESIAN_POINT ( 'NONE',  ( -18.37375256118794553, 11.78967355450649457, 11.49999999999998934 ) ) ;
#16881 = CARTESIAN_POINT ( 'NONE',  ( -121.5228709571501327, -23.96177878511310055, 10.65340807706329329 ) ) ;
#16882 = EDGE_CURVE ( 'NONE', #18030, #66032, #33051, .T. ) ;
#16883 = DIRECTION ( 'NONE',  ( 0.1736481776669261956, -0.9848077530122089085, 0.000000000000000000 ) ) ;
#16884 = CARTESIAN_POINT ( 'NONE',  ( -35.52287095715008292, -24.62285846331435835, 9.038163153548291362 ) ) ;
#16885 = CARTESIAN_POINT ( 'NONE',  ( -17.41291239988371231, 13.16847401419012975, -1.500000000000002220 ) ) ;
#16886 = CARTESIAN_POINT ( 'NONE',  ( -30.57287095715006231, -25.26563519389461732, 3.872667977566617292 ) ) ;
#16887 = ORIENTED_EDGE ( 'NONE', *, *, #41062, .T. ) ;
#16888 = CARTESIAN_POINT ( 'NONE',  ( -28.52287095715005805, -29.50250473134420659, 10.00399446418115268 ) ) ;
#16889 = CARTESIAN_POINT ( 'NONE',  ( -85.59572655174477518, -24.15602025860895807, 10.28564288303535967 ) ) ;
#16890 = ORIENTED_EDGE ( 'NONE', *, *, #9814, .F. ) ;
#16891 = EDGE_CURVE ( 'NONE', #5613, #58474, #21421, .T. ) ;
#16892 = LINE ( 'NONE', #27393, #72964 ) ;
#16893 = EDGE_CURVE ( 'NONE', #68291, #92642, #42769, .T. ) ;
#16894 = EDGE_LOOP ( 'NONE', ( #82044, #39666, #17532, #61830 ) ) ;
#16895 = EDGE_CURVE ( 'NONE', #57446, #32453, #44788, .T. ) ;
#16896 = ORIENTED_EDGE ( 'NONE', *, *, #60770, .T. ) ;
#16897 = CARTESIAN_POINT ( 'NONE',  ( -29.10153610609932073, -25.09928765295969910, 3.502460545500531541 ) ) ;
#16898 = DIRECTION ( 'NONE',  ( 0.000000000000000000, 0.000000000000000000, -1.000000000000000000 ) ) ;
#16899 = CARTESIAN_POINT ( 'NONE',  ( 20.00388196354723291, 7.160935007556333609, -1.500000000000002220 ) ) ;
#16900 = CARTESIAN_POINT ( 'NONE',  ( -66.52287095715006160, -24.65952944569304606, 1.056160979905697239 ) ) ;
#16901 = CARTESIAN_POINT ( 'NONE',  ( -130.5728709571500588, -24.36247485673955637, 0.01136689895587465055 ) ) ;
#16902 = VECTOR ( 'NONE', #18687, 1000.000000000000114 ) ;
#16903 = DIRECTION ( 'NONE',  ( 0.000000000000000000, -2.173523156925979552E-06, 0.9999999999976378895 ) ) ;
#16904 = CARTESIAN_POINT ( 'NONE',  ( -41.52287095715005449, -23.48783264083359867, -1.443836473376375329 ) ) ;
#16905 = CARTESIAN_POINT ( 'NONE',  ( 16.99290379607386114, -9.356058476803225332, -1.500000000000002220 ) ) ;
#16906 = CARTESIAN_POINT ( 'NONE',  ( -117.5535883732406290, -24.35071581493544457, 9.817618358456019934 ) ) ;
#16907 = VERTEX_POINT ( 'NONE', #70115 ) ;
#16908 = CARTESIAN_POINT ( 'NONE',  ( -4.154358412494840280, 19.03220294597612039, 11.49999999999999645 ) ) ;
#16909 = DIRECTION ( 'NONE',  ( -0.9762960071199348056, -0.2164396139380966033, 6.123031769111886291E-17 ) ) ;
#16910 = DIRECTION ( 'NONE',  ( -0.000000000000000000, -1.000000000000000000, -0.000000000000000000 ) ) ;
#16911 = EDGE_CURVE ( 'NONE', #30482, #77370, #66848, .T. ) ;
#16912 = VERTEX_POINT ( 'NONE', #47788 ) ;
#16913 = AXIS2_PLACEMENT_3D ( 'NONE', #12106, #82620, #27840 ) ;
#16914 = CARTESIAN_POINT ( 'NONE',  ( -28.47875734969025885, -6.475225279485573360, -0.08597719988137117464 ) ) ;
#16915 = CARTESIAN_POINT ( 'NONE',  ( -128.5228709571500758, -29.50250786944525672, 11.44777988621622633 ) ) ;
#16916 = CARTESIAN_POINT ( 'NONE',  ( -91.62287095715005592, -23.72773821059536559, 11.05748984161097503 ) ) ;
#16917 = CARTESIAN_POINT ( 'NONE',  ( -10.34999999999999254, 4.999999999999999112, 2.100000000000000089 ) ) ;
#16919 = EDGE_CURVE ( 'NONE', #23684, #44074, #1108, .T. ) ;
#16918 = CARTESIAN_POINT ( 'NONE',  ( -19.15055961920884542, -4.482958728538418924, 11.49999999999998934 ) ) ;
#16920 = EDGE_LOOP ( 'NONE', ( #48596, #44479, #41159, #39484, #84430, #9317, #53112, #57188, #14147, #76016 ) ) ;
#16921 = CARTESIAN_POINT ( 'NONE',  ( -7.206546067468990735, 20.34698395366585189, -1.500000000000002220 ) ) ;
#16922 = LINE ( 'NONE', #72607, #53983 ) ;
#16923 = CARTESIAN_POINT ( 'NONE',  ( -90.52287095715001897, -23.85229601348996908, 10.88205029486208275 ) ) ;
#16924 = CARTESIAN_POINT ( 'NONE',  ( 1.767912858038628965, -23.04938964843747584, -1.500000000000002220 ) ) ;
#16925 = COORDINATED_UNIVERSAL_TIME_OFFSET ( 0, 0, .AHEAD. ) ;
#16926 = CARTESIAN_POINT ( 'NONE',  ( -38.52287095715006870, -29.50248528299804818, 1.056150453629031594 ) ) ;
#16927 = CARTESIAN_POINT ( 'NONE',  ( -105.6228709571500559, -23.47596703998600631, 11.44779298504227860 ) ) ;
#16928 = CARTESIAN_POINT ( 'NONE',  ( -84.62287095715005592, -24.64965695001469115, 8.947790433994182280 ) ) ;
#16929 = CARTESIAN_POINT ( 'NONE',  ( -104.5228709571500758, -24.50321055353806088, 9.387540953477520489 ) ) ;
#16930 = CARTESIAN_POINT ( 'NONE',  ( 6.044119082205957838, -5.876774720514423400, 21.40268112089023589 ) ) ;
#16931 = CARTESIAN_POINT ( 'NONE',  ( -124.5228709571500616, -23.48786465467241769, 11.44779295918253759 ) ) ;
#16932 = CARTESIAN_POINT ( 'NONE',  ( -114.5542467394807318, -24.15620529776629510, 10.23563542870659404 ) ) ;
#16933 = CARTESIAN_POINT ( 'NONE',  ( 7.348632388941331861, 18.53259892055224611, 11.49999999999998934 ) ) ;
#16934 = B_SPLINE_CURVE_WITH_KNOTS ( 'NONE', 3,
 ( #14309, #20927, #13309, #45282, #12314, #82828, #89950, #20420, #12813, #44289, #74713, #75218 ),
 .UNSPECIFIED., .F., .F.,
 ( 4, 2, 2, 2, 2, 4 ),
 ( -0.003357017750235514672, -0.001150730439442379169, 0.001055556871350756334, 0.002158700526747327555, 0.003261844182143899644, 0.005468131492937042953 ),
 .UNSPECIFIED. ) ;
#16935 = CARTESIAN_POINT ( 'NONE',  ( -100.9404532381483079, -25.21193246312661529, 3.416343243334487578 ) ) ;
#16936 = CARTESIAN_POINT ( 'NONE',  ( -14.51517298184297289, -13.48802281452852725, -1.500000000000002220 ) ) ;
#16937 = ORIENTED_EDGE ( 'NONE', *, *, #17846, .T. ) ;
#16938 = LINE ( 'NONE', #76820, #39413 ) ;
#16939 = EDGE_CURVE ( 'NONE', #41305, #628, #78701, .T. ) ;
#16940 = DIRECTION ( 'NONE',  ( -1.000000000000000000, 0.000000000000000000, 0.000000000000000000 ) ) ;
#16941 = VECTOR ( 'NONE', #12057, 1000.000000000000000 ) ;
#16942 = PLANE ( 'NONE',  #7009 ) ;
#16943 = CARTESIAN_POINT ( 'NONE',  ( 12.20387445076365296, 16.77033177596414504, 11.49999999999999645 ) ) ;
#16944 = CARTESIAN_POINT ( 'NONE',  ( -70.74026866089612042, -29.50249362659879537, 4.894895270847094970 ) ) ;
#16945 = B_SPLINE_CURVE_WITH_KNOTS ( 'NONE', 3,
 ( #69492, #85713, #100409, #47160 ),
 .UNSPECIFIED., .F., .F.,
 ( 4, 4 ),
 ( 0.000000000000000000, 0.002769230769230773825 ),
 .UNSPECIFIED. ) ;
#16946 = EDGE_CURVE ( 'NONE', #89020, #65068, #68617, .T. ) ;
#16947 = LINE ( 'NONE', #1236, #2031 ) ;
#16948 = CARTESIAN_POINT ( 'NONE',  ( 10.97283692364161922, -19.94330716608196852, 11.49999999999999645 ) ) ;
#16949 = EDGE_LOOP ( 'NONE', ( #87156, #10976, #72796, #72024 ) ) ;
#16950 = CARTESIAN_POINT ( 'NONE',  ( -112.2228709571500502, -23.47596703998600631, 11.44779298504227860 ) ) ;
#16951 = CARTESIAN_POINT ( 'NONE',  ( -38.52287095715008292, -23.48783264083452593, -1.443836473374935592 ) ) ;
#16952 = ORIENTED_EDGE ( 'NONE', *, *, #84929, .T. ) ;
#16953 = CARTESIAN_POINT ( 'NONE',  ( -19.21899500656021331, -6.280627263257740900, -1.500000000000002220 ) ) ;
#16954 = LINE ( 'NONE', #38790, #82449 ) ;
#16955 = CARTESIAN_POINT ( 'NONE',  ( -67.62287095715005592, -29.50250243563736774, 8.947779886222143375 ) ) ;
#16956 = VERTEX_POINT ( 'NONE', #86342 ) ;
#16957 = CARTESIAN_POINT ( 'NONE',  ( -32.62287095715004881, -23.48783264082477729, -1.443836473390074371 ) ) ;
#16958 = CARTESIAN_POINT ( 'NONE',  ( -17.89994474767736676, -14.32179853049041363, 11.49999999999998934 ) ) ;
#16959 = CARTESIAN_POINT ( 'NONE',  ( -84.52287095715003318, -24.33927499327855060, 9.819080762295811837 ) ) ;
#16960 = CARTESIAN_POINT ( 'NONE',  ( -18.81269933604069067, 6.858547123926768130, -1.500000000000002220 ) ) ;
#16961 = CARTESIAN_POINT ( 'NONE',  ( -36.62287095715007723, -23.95044443724991368, 10.65354141964650125 ) ) ;
#16962 = CARTESIAN_POINT ( 'NONE',  ( -15.18370147500227496, -14.46048895944246127, 11.49999999999999645 ) ) ;
#16963 = CARTESIAN_POINT ( 'NONE',  ( -59.56094173781918499, -25.21083105912962097, 3.409327675794633805 ) ) ;
#16964 = CARTESIAN_POINT ( 'NONE',  ( -68.99199226862026535, -25.24754449216967345, 5.787353197655024317 ) ) ;
#16965 = CARTESIAN_POINT ( 'NONE',  ( 17.21905055353458991, -13.78536315820828229, 11.49999999999998934 ) ) ;
#16966 = AXIS2_PLACEMENT_3D ( 'NONE', #19812, #12702, #81229 ) ;
#16967 = DIRECTION ( 'NONE',  ( 1.084136044942898696E-16, 0.000000000000000000, -1.000000000000000000 ) ) ;
#16968 = ORIENTED_EDGE ( 'NONE', *, *, #60948, .F. ) ;
#16969 = LINE ( 'NONE', #39308, #78410 ) ;
#16970 = PLANE ( 'NONE',  #81890 ) ;
#16971 = ORIENTED_EDGE ( 'NONE', *, *, #42606, .T. ) ;
#16972 = CARTESIAN_POINT ( 'NONE',  ( 3.325015365150250535, -6.376774720514402972, 18.26971317031913955 ) ) ;
#16973 = ORIENTED_EDGE ( 'NONE', *, *, #42594, .F. ) ;
#16974 = ORIENTED_EDGE ( 'NONE', *, *, #13101, .F. ) ;
#16975 = CARTESIAN_POINT ( 'NONE',  ( -101.6430330839730516, -25.26303730729093999, 3.986250639247583827 ) ) ;
#16976 = CARTESIAN_POINT ( 'NONE',  ( -80.62287095715004170, -23.48786465467241058, 11.44779295918254469 ) ) ;
#16977 = CARTESIAN_POINT ( 'NONE',  ( -100.5228709571500616, -24.99156044556120904, 7.747789690856173195 ) ) ;
#16978 = CARTESIAN_POINT ( 'NONE',  ( -16.44861368136865920, 12.28130381464353782, -1.500000000000002220 ) ) ;
#16979 = VECTOR ( 'NONE', #87653, 1000.000000000000000 ) ;
#16980 = VERTEX_POINT ( 'NONE', #99539 ) ;
#16981 = CARTESIAN_POINT ( 'NONE',  ( -105.6228709571500559, -29.50250786944525672, 11.44777988621622988 ) ) ;
#16982 = CARTESIAN_POINT ( 'NONE',  ( -44.58708426901613819, -24.34968618360933235, 0.1864209137778787551 ) ) ;
#16983 = DIRECTION ( 'NONE',  ( -3.773278334453079618E-23, 0.9999999999976377785, 2.173523156925979975E-06 ) ) ;
#16984 = CARTESIAN_POINT ( 'NONE',  ( -10.38793682863964563, 19.71736701935523683, -1.500000000000002220 ) ) ;
#16985 = CARTESIAN_POINT ( 'NONE',  ( -55.52287095715007581, -23.85229601348996198, 10.88205029486209519 ) ) ;
#16986 = CARTESIAN_POINT ( 'NONE',  ( -1.501937386944296460, -5.876774720514415407, 19.86422795159478483 ) ) ;
#16987 = EDGE_LOOP ( 'NONE', ( #17529, #50107, #32995, #72050 ) ) ;
#16988 = CARTESIAN_POINT ( 'NONE',  ( -47.62287095715004881, -29.50250786944525672, 11.44777988621624054 ) ) ;
#16989 = CARTESIAN_POINT ( 'NONE',  ( -118.5228709571500474, -23.94994826722564696, -0.6494450866342723616 ) ) ;
#16990 = CARTESIAN_POINT ( 'NONE',  ( 8.324980675869593227, 19.10421180063631752, -1.500000000000002220 ) ) ;
#16991 = VERTEX_POINT ( 'NONE', #16825 ) ;
#16993 = VERTEX_POINT ( 'NONE', #77706 ) ;
#16992 = CARTESIAN_POINT ( 'NONE',  ( -52.52287095715006870, -29.50250243563736774, 8.947779886222146928 ) ) ;
#16994 = EDGE_LOOP ( 'NONE', ( #65968, #25465, #48189, #4308 ) ) ;
#16995 = EDGE_CURVE ( 'NONE', #43562, #76018, #30037, .T. ) ;
#16996 = CARTESIAN_POINT ( 'NONE',  ( -103.9228709571500673, -23.47593901973090169, -1.443836447538996648 ) ) ;
#16997 = CARTESIAN_POINT ( 'NONE',  ( -17.07941033872765146, 12.18221932706078370, -1.500000000000002220 ) ) ;
#16998 = VERTEX_POINT ( 'NONE', #63022 ) ;
#16999 = DIRECTION ( 'NONE',  ( 0.000000000000000000, 0.000000000000000000, 1.000000000000000000 ) ) ;
#17001 = EDGE_CURVE ( 'NONE', #65428, #48796, #15817, .T. ) ;
#17000 = CARTESIAN_POINT ( 'NONE',  ( 30.09341516180546350, -1.682774720514426114, -11.39311774897855933 ) ) ;
#17002 = CARTESIAN_POINT ( 'NONE',  ( -95.52287095715006160, -23.48786465467241769, 11.44779295918254114 ) ) ;
#17003 = B_SPLINE_CURVE_WITH_KNOTS ( 'NONE', 3,
 ( #31746, #68314, #45489, #37862 ),
 .UNSPECIFIED., .F., .F.,
 ( 4, 4 ),
 ( 0.000000000000000000, 1.000000000000000000 ),
 .UNSPECIFIED. ) ;
#17004 = CARTESIAN_POINT ( 'NONE',  ( -100.9913061220214843, -25.25419536262793230, 7.480517119236268719 ) ) ;
#17005 = CARTESIAN_POINT ( 'NONE',  ( -59.55981030432491963, -23.73766607897669445, -1.055555164236460675 ) ) ;
#17006 = DIRECTION ( 'NONE',  ( 0.000000000000000000, 0.000000000000000000, 1.000000000000000000 ) ) ;
#17007 = CARTESIAN_POINT ( 'NONE',  ( -65.62287095715009855, -24.15516710230293995, 10.28746687063726029 ) ) ;
#17009 = VERTEX_POINT ( 'NONE', #46276 ) ;
#17008 = CARTESIAN_POINT ( 'NONE',  ( 10.53326394202159300, -19.55463526559320542, 11.49999999999999645 ) ) ;
#17010 = CARTESIAN_POINT ( 'NONE',  ( 8.160000000000000142, -2.890508098367099432, -0.2344417481469836528 ) ) ;
#17011 = CARTESIAN_POINT ( 'NONE',  ( -71.25851563654804011, -25.27180963933369284, 5.909805672228780615 ) ) ;
#17012 = ORIENTED_EDGE ( 'NONE', *, *, #9653, .F. ) ;
#17013 = EDGE_CURVE ( 'NONE', #11637, #14276, #68091, .T. ) ;
#17014 = CARTESIAN_POINT ( 'NONE',  ( -15.33504971967173702, 16.71734053393862496, -1.500000000000002220 ) ) ;
#17015 = EDGE_CURVE ( 'NONE', #31334, #38206, #88580, .T. ) ;
#17017 = VERTEX_POINT ( 'NONE', #69622 ) ;
#17016 = DIRECTION ( 'NONE',  ( 0.000000000000000000, 0.000000000000000000, 1.000000000000000000 ) ) ;
#17018 = ADVANCED_FACE ( 'NONE', ( #69105 ), #62510, .F. ) ;
#17019 = ORIENTED_EDGE ( 'NONE', *, *, #5097, .F. ) ;
#17020 = CIRCLE ( 'NONE', #80249, 2.249999999999998668 ) ;
#17021 = ADVANCED_FACE ( 'NONE', ( #23932 ), #3743, .T. ) ;
#17022 = FACE_OUTER_BOUND ( 'NONE', #6194, .T. ) ;
#17023 = CARTESIAN_POINT ( 'NONE',  ( -6.497366621441947210, -19.08602653180391329, 11.49999999999998934 ) ) ;
#17024 = CARTESIAN_POINT ( 'NONE',  ( -99.55620429048339304, -23.47596703998600631, 11.44779298504227683 ) ) ;
#17025 = VERTEX_POINT ( 'NONE', #33557 ) ;
#17026 = CARTESIAN_POINT ( 'NONE',  ( -58.62287095715004881, -23.48783264082478439, -1.443836473390069264 ) ) ;
#17027 = CARTESIAN_POINT ( 'NONE',  ( 18.65981798208652265, 12.38953945867474360, -1.500000000000002220 ) ) ;
#17028 = VERTEX_POINT ( 'NONE', #2122 ) ;
#17029 = VERTEX_POINT ( 'NONE', #72632 ) ;
#17030 = CARTESIAN_POINT ( 'NONE',  ( -112.6270362718817779, -24.15620529776628445, 10.23563542870659582 ) ) ;
#17031 = CARTESIAN_POINT ( 'NONE',  ( -94.51552167049113962, -23.96169478059713143, 10.65365249895717881 ) ) ;
#17032 = CARTESIAN_POINT ( 'NONE',  ( 5.550000000000006040, -14.50000000000000178, 12.73734666247252711 ) ) ;
#17033 = PLANE ( 'NONE',  #75727 ) ;
#17034 = DIRECTION ( 'NONE',  ( -3.773278334453080206E-23, 0.9999999999976377785, 2.173523156925979975E-06 ) ) ;
#17035 = CARTESIAN_POINT ( 'NONE',  ( -4.924063254364682507, -18.92933890202812464, 11.49999999999998934 ) ) ;
#17036 = B_SPLINE_CURVE_WITH_KNOTS ( 'NONE', 3,
 ( #31503, #61472, #99992, #92395 ),
 .UNSPECIFIED., .F., .F.,
 ( 4, 4 ),
 ( 0.000000000000000000, 9.999999999997510880E-05 ),
 .UNSPECIFIED. ) ;
#17037 = DIRECTION ( 'NONE',  ( 0.000000000000000000, 0.000000000000000000, 1.000000000000000000 ) ) ;
#17038 = VERTEX_POINT ( 'NONE', #87334 ) ;
#17039 = CARTESIAN_POINT ( 'NONE',  ( -2.374466145016132845, -21.38244973876172494, 11.49999999999998934 ) ) ;
#17040 = CARTESIAN_POINT ( 'NONE',  ( -36.52287095715006870, -24.51283580621364777, 0.6167428607019721509 ) ) ;
#17041 = CARTESIAN_POINT ( 'NONE',  ( -54.62287095715006302, -23.72773821059535493, 11.05748984161097503 ) ) ;
#17042 = DIRECTION ( 'NONE',  ( 0.000000000000000000, 0.000000000000000000, 1.000000000000000000 ) ) ;
#17043 = LINE ( 'NONE', #47002, #58537 ) ;
#17045 = VECTOR ( 'NONE', #45061, 1000.000000000000000 ) ;
#17044 = CARTESIAN_POINT ( 'NONE',  ( 21.91704834537361180, 6.644925864936762849, -1.500000000000002220 ) ) ;
#17046 = PERSON_AND_ORGANIZATION_ROLE ( 'creator' ) ;
#17047 = CARTESIAN_POINT ( 'NONE',  ( -85.22287095715007865, -23.47596703998600631, 11.44779298504227860 ) ) ;
#17048 = CARTESIAN_POINT ( 'NONE',  ( -53.51456551345987123, -23.73766607897669800, -1.055555164236460008 ) ) ;
#17049 = CARTESIAN_POINT ( 'NONE',  ( 11.39338536883839659, -16.50304575528446804, 11.49999999999999645 ) ) ;
#17050 = CARTESIAN_POINT ( 'NONE',  ( -80.35919894935766195, -25.26612373672872636, 4.505481401771154637 ) ) ;
#17051 = DIRECTION ( 'NONE',  ( -0.4771587602595986910, -0.8788171126619707119, 0.000000000000000000 ) ) ;
#17052 = CARTESIAN_POINT ( 'NONE',  ( -73.52287095715010423, -23.48783264082477018, -1.443836473390093689 ) ) ;
#17053 = LINE ( 'NONE', #56642, #42391 ) ;
#17054 = CARTESIAN_POINT ( 'NONE',  ( -118.6228709571500701, -23.48783264082478794, -1.443836473390058384 ) ) ;
#17055 = VECTOR ( 'NONE', #3432, 1000.000000000000114 ) ;
#17056 = CARTESIAN_POINT ( 'NONE',  ( -4.706806674773570620, -21.25045708977441450, 11.49999999999998934 ) ) ;
#17057 = DIRECTION ( 'NONE',  ( -1.000000000000000000, 0.000000000000000000, 0.000000000000000000 ) ) ;
#17058 = CARTESIAN_POINT ( 'NONE',  ( -6.723608784814384620, 18.44229941887336821, -1.500000000000002220 ) ) ;
#17059 = AXIS2_PLACEMENT_3D ( 'NONE', #19467, #87490, #3273 ) ;
#17060 = DIRECTION ( 'NONE',  ( -0.000000000000000000, 0.000000000000000000, 1.000000000000000000 ) ) ;
#17061 = CARTESIAN_POINT ( 'NONE',  ( -110.2093792378191921, -25.31698244681350474, 5.585409175846506535 ) ) ;
#17062 = SECURITY_CLASSIFICATION_LEVEL ( 'unclassified' ) ;
#17063 = FACE_OUTER_BOUND ( 'NONE', #26514, .T. ) ;
#17064 = CARTESIAN_POINT ( 'NONE',  ( -98.62287095715005592, -24.66019654487199730, 8.947790411086124607 ) ) ;
#17065 = CARTESIAN_POINT ( 'NONE',  ( 13.18781518674367348, -15.76626393773247337, 11.49999999999999645 ) ) ;
#17066 = CARTESIAN_POINT ( 'NONE',  ( 4.016587897052070311, -5.876774720514425177, 21.44459449800855921 ) ) ;
#17067 = ADVANCED_FACE ( 'NONE', ( #57911 ), #88855, .T. ) ;
#17068 = CARTESIAN_POINT ( 'NONE',  ( -120.5553418306319884, -24.15503026093913874, -0.2815557561904507011 ) ) ;
#17069 = CARTESIAN_POINT ( 'NONE',  ( 8.141615846073909424, -21.09679883994429161, 11.49999999999999645 ) ) ;
#17070 = EDGE_LOOP ( 'NONE', ( #13224, #38560, #81632 ) ) ;
#17071 = ADVANCED_FACE ( 'NONE', ( #79720 ), #95450, .T. ) ;
#17072 = CARTESIAN_POINT ( 'NONE',  ( -100.6258216950799778, -25.31296450549008625, 4.735305783089845733 ) ) ;
#17073 = DIRECTION ( 'NONE',  ( -0.000000000000000000, 0.000000000000000000, -1.000000000000000000 ) ) ;
#17074 = CARTESIAN_POINT ( 'NONE',  ( -125.5894637005920629, -24.63419186844610920, 9.035850630976920428 ) ) ;
#17075 = CARTESIAN_POINT ( 'NONE',  ( -27.12628703559276389, -24.76673041788330920, 2.399896000618569669 ) ) ;
#17076 = B_SPLINE_CURVE_WITH_KNOTS ( 'NONE', 3,
 ( #77295, #4449, #38241, #38741, #74925, #5429 ),
 .UNSPECIFIED., .F., .F.,
 ( 4, 2, 4 ),
 ( 0.000000000000000000, 0.001380901958385391580, 0.002761803916770783161 ),
 .UNSPECIFIED. ) ;
#17077 = DIRECTION ( 'NONE',  ( 0.9951627101165076983, -0.09824042138329622254, -8.881784197001249168E-15 ) ) ;
#17078 = CARTESIAN_POINT ( 'NONE',  ( -127.5228709571500616, -29.50250786944525672, 11.44777988621622633 ) ) ;
#17079 = B_SPLINE_CURVE_WITH_KNOTS ( 'NONE', 3,
 ( #83966, #85456, #14945, #45917, #15445, #93562 ),
 .UNSPECIFIED., .F., .F.,
 ( 4, 2, 4 ),
 ( 1.570887131794952276E-05, 0.001396322306279764325, 0.002776935741241578874 ),
 .UNSPECIFIED. ) ;
#17080 = ORIENTED_EDGE ( 'NONE', *, *, #82640, .T. ) ;
#17081 = CARTESIAN_POINT ( 'NONE',  ( -80.19887417545862718, -25.31596225461789729, 4.982290565433718399 ) ) ;
#17082 = CARTESIAN_POINT ( 'NONE',  ( 7.824713763024562674, 21.46283361357968289, -1.500000000000002220 ) ) ;
#17083 = CARTESIAN_POINT ( 'NONE',  ( 5.514125806255895004E-17, -29.50250243563707286, 8.947779751028683393 ) ) ;
#17084 = CARTESIAN_POINT ( 'NONE',  ( -72.55620429048340725, -24.66019654487199020, 8.947790411086131712 ) ) ;
#17085 = CARTESIAN_POINT ( 'NONE',  ( -82.58247480767941795, -24.66019654487199730, 8.947790411086122830 ) ) ;
#17086 = AXIS2_PLACEMENT_3D ( 'NONE', #86214, #84204, #71000 ) ;
#17087 = CARTESIAN_POINT ( 'NONE',  ( 6.846561153812083411, -21.39451737393737574, 11.49999999999999645 ) ) ;
#17088 = ORIENTED_EDGE ( 'NONE', *, *, #33182, .T. ) ;
#17089 = CARTESIAN_POINT ( 'NONE',  ( -81.62287095715005592, -29.50250786944525672, 11.44777988621623521 ) ) ;
#17090 = CARTESIAN_POINT ( 'NONE',  ( -8.017166757594178961, 20.41873492177044724, -1.500000000000002220 ) ) ;
#17092 = ADVANCED_FACE ( 'NONE', ( #65038 ), #73127, .F. ) ;
#17091 = CC_DESIGN_PERSON_AND_ORGANIZATION_ASSIGNMENT ( #66387, #97315, ( #96051 ) ) ;
#17093 = CARTESIAN_POINT ( 'NONE',  ( -114.5228709571500758, -24.33927499327856125, 9.819080762295810061 ) ) ;
#17094 = CARTESIAN_POINT ( 'NONE',  ( -34.59402351810827980, -24.15620529776627379, 10.23563542870661003 ) ) ;
#17095 = DIRECTION ( 'NONE',  ( -3.773278334453079618E-23, 0.9999999999976377785, 2.173523156925979975E-06 ) ) ;
#17096 = EDGE_LOOP ( 'NONE', ( #59932, #23722, #25104, #43084 ) ) ;
#17097 = CARTESIAN_POINT ( 'NONE',  ( -48.66106295358616052, -23.48786465467241058, 11.44779295918254824 ) ) ;
#17098 = DIRECTION ( 'NONE',  ( 3.773278334444167608E-23, -1.000000000000000000, 0.000000000000000000 ) ) ;
#17099 = EDGE_LOOP ( 'NONE', ( #8402, #77414, #54285, #7545 ) ) ;
#17100 = CARTESIAN_POINT ( 'NONE',  ( -19.64171699416042571, -5.764624264842452384, 11.49999999999998934 ) ) ;
#17101 = VERTEX_POINT ( 'NONE', #63523 ) ;
#17102 = ORIENTED_EDGE ( 'NONE', *, *, #3971, .T. ) ;
#17103 = EDGE_LOOP ( 'NONE', ( #2315, #89100, #71167, #66441 ) ) ;
#17104 = ORIENTED_EDGE ( 'NONE', *, *, #2706, .T. ) ;
#17105 = CARTESIAN_POINT ( 'NONE',  ( 19.40787663092975279, -12.54570180764831377, -1.500000000000002220 ) ) ;
#17106 = CARTESIAN_POINT ( 'NONE',  ( -40.79597241634589722, -25.30977039686255026, 4.487062071701387822 ) ) ;
#17107 = CARTESIAN_POINT ( 'NONE',  ( 16.59675031405745571, -11.69241480613374407, -1.500000000000002220 ) ) ;
#17108 = VERTEX_POINT ( 'NONE', #18821 ) ;
#17109 = PLANE ( 'NONE',  #7195 ) ;
#17110 = CARTESIAN_POINT ( 'NONE',  ( -72.52287095715009002, -23.72747288104470087, -1.053458166803226570 ) ) ;
#17111 = DIRECTION ( 'NONE',  ( -1.000000000000000000, -3.773278334444167608E-23, -8.201307833595939069E-29 ) ) ;
#17112 = CARTESIAN_POINT ( 'NONE',  ( 4.627238781264984446, -6.376774720514408301, 19.49219360614394247 ) ) ;
#17114 = ORIENTED_EDGE ( 'NONE', *, *, #60800, .F. ) ;
#17113 = CARTESIAN_POINT ( 'NONE',  ( -16.68621059303058018, 13.52761613308161870, 11.49999999999999645 ) ) ;
#17115 = FACE_OUTER_BOUND ( 'NONE', #8373, .T. ) ;
#17116 = CARTESIAN_POINT ( 'NONE',  ( 3.421177667410916001, 5.965225279485572685, 28.69411518427638441 ) ) ;
#17117 = ORIENTED_EDGE ( 'NONE', *, *, #22981, .F. ) ;
#17118 = CARTESIAN_POINT ( 'NONE',  ( 14.12806351585482112, -15.20395780304818523, 11.49999999999998934 ) ) ;
#17119 = ORIENTED_EDGE ( 'NONE', *, *, #55862, .F. ) ;
#17121 = ORIENTED_EDGE ( 'NONE', *, *, #14833, .T. ) ;
#17120 = CARTESIAN_POINT ( 'NONE',  ( -10.59832330691884117, 6.376774720514425177, -27.05373799718301697 ) ) ;
#17122 = VECTOR ( 'NONE', #13968, 1000.000000000000000 ) ;
#17123 = CARTESIAN_POINT ( 'NONE',  ( -75.62287095715004170, -24.99156045073392818, 7.747789690856161648 ) ) ;
#17124 = CARTESIAN_POINT ( 'NONE',  ( -53.52287095715008292, -23.48783264082477018, -1.443836473390094799 ) ) ;
#17125 = ORIENTED_EDGE ( 'NONE', *, *, #36009, .F. ) ;
#17126 = ORIENTED_EDGE ( 'NONE', *, *, #66768, .F. ) ;
#17127 = DIRECTION ( 'NONE',  ( -0.000000000000000000, 1.000000000000000000, -0.000000000000000000 ) ) ;
#17128 = CARTESIAN_POINT ( 'NONE',  ( -42.53413042267195010, -24.51419770103158413, 9.386484678747191168 ) ) ;
#17129 = CIRCLE ( 'NONE', #52771, 3.349999999999998757 ) ;
#17130 = CARTESIAN_POINT ( 'NONE',  ( -43.63415880193262097, -24.35071581493542325, 9.817618358456034144 ) ) ;
#17132 = ORIENTED_EDGE ( 'NONE', *, *, #38960, .F. ) ;
#17131 = CARTESIAN_POINT ( 'NONE',  ( -1.213202359833694732, 22.00568734548514627, 11.49999999999999645 ) ) ;
#17133 = AXIS2_PLACEMENT_3D ( 'NONE', #84098, #14583, #6980 ) ;
#17134 = CARTESIAN_POINT ( 'NONE',  ( -103.5953259629072392, -23.73766607897670156, -1.055555164236454901 ) ) ;
#17135 = ADVANCED_FACE ( 'NONE', ( #49803 ), #80735, .T. ) ;
#17136 = CARTESIAN_POINT ( 'NONE',  ( -12.77507031947300042, 18.62636059118606724, 11.49999999999998934 ) ) ;
#17137 = VECTOR ( 'NONE', #22444, 1000.000000000000114 ) ;
#17138 = CARTESIAN_POINT ( 'NONE',  ( 3.785439364192078937, -20.66625369722972749, -1.500000000000002220 ) ) ;
#17140 = VERTEX_POINT ( 'NONE', #9207 ) ;
#17139 = LINE ( 'NONE', #10528, #13405 ) ;
#17141 = EDGE_CURVE ( 'NONE', #81135, #75736, #89832, .T. ) ;
#17142 = VERTEX_POINT ( 'NONE', #64540 ) ;
#17143 = EDGE_CURVE ( 'NONE', #66209, #57524, #18331, .T. ) ;
#17144 = LINE ( 'NONE', #40491, #35275 ) ;
#17145 = CARTESIAN_POINT ( 'NONE',  ( 8.982289454725524536, -0.9478013341236715128, -3.727086380289611256 ) ) ;
#17146 = EDGE_LOOP ( 'NONE', ( #6377, #50580, #75604, #91813 ) ) ;
#17147 = CARTESIAN_POINT ( 'NONE',  ( 20.71511372717374755, 4.256074106246791722, -1.500000000000002220 ) ) ;
#17148 = CARTESIAN_POINT ( 'NONE',  ( 26.73860345374794178, -1.682774720514426114, -1.272392034746785860 ) ) ;
#17149 = CARTESIAN_POINT ( 'NONE',  ( -51.90898564286461436, -25.26040870674269101, 6.429377479227253112 ) ) ;
#17150 = CARTESIAN_POINT ( 'NONE',  ( -88.62287095714998486, -24.33927499327853994, 9.819080762295810061 ) ) ;
#17151 = CARTESIAN_POINT ( 'NONE',  ( -28.62287095715004881, -23.33150569529546914, 11.44779297407613150 ) ) ;
#17152 = DIRECTION ( 'NONE',  ( -1.000000000000000000, -0.000000000000000000, -7.994117400814786717E-16 ) ) ;
#17153 = CARTESIAN_POINT ( 'NONE',  ( -19.03210976516136554, 11.49075778266564107, -1.500000000000002220 ) ) ;
#17154 = CARTESIAN_POINT ( 'NONE',  ( -114.5222273449358141, -23.48783264082478794, -1.443836473390062380 ) ) ;
#17155 = EDGE_CURVE ( 'NONE', #73714, #13179, #71624, .T. ) ;
#17156 = ORIENTED_EDGE ( 'NONE', *, *, #32616, .F. ) ;
#17157 = CARTESIAN_POINT ( 'NONE',  ( -5.576843645946834016, -6.376774720514418959, 20.41272575174755133 ) ) ;
#17158 = CARTESIAN_POINT ( 'NONE',  ( -37.63490762544056167, -24.34968618360933590, 0.1864209137778856384 ) ) ;
#17159 = CARTESIAN_POINT ( 'NONE',  ( -126.6239571621962341, -24.34968618360934300, 0.1864209137778884418 ) ) ;
#17160 = CARTESIAN_POINT ( 'NONE',  ( -100.5858031092710547, -24.83618233451450763, 1.606449574219537713 ) ) ;
#17161 = CARTESIAN_POINT ( 'NONE',  ( -53.01255352321339842, -1.682774720514426114, 35.59556822165056644 ) ) ;
#17162 = CARTESIAN_POINT ( 'NONE',  ( 1.793504005174451077, 19.40006364325761012, 11.49999999999998934 ) ) ;
#17163 = B_SPLINE_CURVE_WITH_KNOTS ( 'NONE', 3,
 ( #45700, #7126, #38582, #44206, #69541, #38076 ),
 .UNSPECIFIED., .F., .F.,
 ( 4, 2, 4 ),
 ( 0.000000000000000000, 0.001380901958385383774, 0.002761803916770767548 ),
 .UNSPECIFIED. ) ;
#17164 = CARTESIAN_POINT ( 'NONE',  ( -19.74196057798672399, -8.316236533413031040, 11.49999999999998934 ) ) ;
#17165 = CARTESIAN_POINT ( 'NONE',  ( -12.64432969575900323, 5.965225279485592225, -26.13179214487284696 ) ) ;
#17166 = CARTESIAN_POINT ( 'NONE',  ( -60.62821527951275868, -24.83644354574317603, 8.397322867105112110 ) ) ;
#17167 = CARTESIAN_POINT ( 'NONE',  ( -113.5228709571500616, -29.50250243563736774, 8.947779886222136270 ) ) ;
#17168 = CARTESIAN_POINT ( 'NONE',  ( -36.62287095715005592, -23.47593901973091235, -1.443836447539011525 ) ) ;
#17169 = CARTESIAN_POINT ( 'NONE',  ( 2.720868037236281012, -22.60253418658637869, -1.500000000000002220 ) ) ;
#17170 = DIRECTION ( 'NONE',  ( 0.000000000000000000, 0.000000000000000000, -1.000000000000000000 ) ) ;
#17171 = CARTESIAN_POINT ( 'NONE',  ( -98.62287095715004170, -24.65952944569304606, 1.056160979905700792 ) ) ;
#17172 = CARTESIAN_POINT ( 'NONE',  ( -4.768723929037996356, 19.30091236029735668, 11.49999999999999645 ) ) ;
#17173 = CARTESIAN_POINT ( 'NONE',  ( 5.705253819860196529, -6.376774720514415407, 19.95963554344900714 ) ) ;
#17174 = CARTESIAN_POINT ( 'NONE',  ( -108.5895376238167245, -23.48786465467242479, 11.44779295918253759 ) ) ;
#17175 = LINE ( 'NONE', #56767, #87780 ) ;
#17176 = VERTEX_POINT ( 'NONE', #51280 ) ;
#17177 = CARTESIAN_POINT ( 'NONE',  ( 30.13634516277803144, 5.269088466187364261, 19.84760796525321780 ) ) ;
#17178 = CARTESIAN_POINT ( 'NONE',  ( -6.181720432442950219, -6.376774720514410077, 19.67464842890028720 ) ) ;
#17179 = CARTESIAN_POINT ( 'NONE',  ( -29.49875734969025842, -0.3587747205144265483, 17.86602280011862476 ) ) ;
#17180 = CARTESIAN_POINT ( 'NONE',  ( -18.79206335510377102, -10.79472360063173397, -1.500000000000002220 ) ) ;
#17181 = CARTESIAN_POINT ( 'NONE',  ( 6.817081463290844745, -0.6683258531633596844, 18.35000000000000142 ) ) ;
#17182 = CARTESIAN_POINT ( 'NONE',  ( -16.97169330436246781, 9.548981535075045102, -1.500000000000002220 ) ) ;
#17183 = AXIS2_PLACEMENT_3D ( 'NONE', #3536, #27857, #34478 ) ;
#17184 = CARTESIAN_POINT ( 'NONE',  ( -55.58900237498185959, -24.52399227489126687, 9.353111116836526406 ) ) ;
#17185 = EDGE_CURVE ( 'NONE', #34410, #52696, #83382, .T. ) ;
#17186 = VERTEX_POINT ( 'NONE', #75593 ) ;
#17187 = CARTESIAN_POINT ( 'NONE',  ( 5.143668500415711442, -19.74887971880038151, 11.49999999999999645 ) ) ;
#17188 = CARTESIAN_POINT ( 'NONE',  ( 22.81105451610979173, 8.475225279485572472, -19.61691820600746539 ) ) ;
#17189 = EDGE_CURVE ( 'NONE', #10158, #70435, #5600, .T. ) ;
#17190 = VECTOR ( 'NONE', #83474, 1000.000000000000114 ) ;
#17191 = DIRECTION ( 'NONE',  ( 1.000000000000000000, 3.773278334444167608E-23, 8.201307833595939069E-29 ) ) ;
#17192 = VERTEX_POINT ( 'NONE', #27943 ) ;
#17193 = CARTESIAN_POINT ( 'NONE',  ( -9.383883476483159569, 17.86611652351680846, 0.000000000000000000 ) ) ;
#17194 = CARTESIAN_POINT ( 'NONE',  ( -39.14714599385568761, -25.31628570854560678, 4.777938624344938212 ) ) ;
#17195 = VECTOR ( 'NONE', #62325, 1000.000000000000114 ) ;
#17196 = CARTESIAN_POINT ( 'NONE',  ( -8.349999999999971223, 27.69999999999999574, 2.100000000000000089 ) ) ;
#17197 = AXIS2_PLACEMENT_3D ( 'NONE', #86813, #49279, #17301 ) ;
#17198 = CARTESIAN_POINT ( 'NONE',  ( -74.52287095715007581, -29.50248528299804818, 1.056150453629036701 ) ) ;
#17199 = CARTESIAN_POINT ( 'NONE',  ( 19.99232773509726258, 2.034096180923423702, -1.500000000000002220 ) ) ;
#17200 = AXIS2_PLACEMENT_3D ( 'NONE', #90807, #76069, #75564 ) ;
#17201 = DIRECTION ( 'NONE',  ( 9.426781450619601849E-18, -6.307606751056558338E-17, 1.000000000000000000 ) ) ;
#17202 = ORIENTED_EDGE ( 'NONE', *, *, #31718, .F. ) ;
#17203 = CARTESIAN_POINT ( 'NONE',  ( -66.58774706379415420, -24.35071581493543036, 9.817618358456028815 ) ) ;
#17204 = VECTOR ( 'NONE', #28311, 1000.000000000000000 ) ;
#17205 = CARTESIAN_POINT ( 'NONE',  ( 8.986065527603487979, -21.13286776747340667, 11.49999999999999645 ) ) ;
#17206 = CARTESIAN_POINT ( 'NONE',  ( 21.04450177026006230, 8.645109164175620364, -1.500000000000002220 ) ) ;
#17207 = ORIENTED_EDGE ( 'NONE', *, *, #2457, .F. ) ;
#17208 = CARTESIAN_POINT ( 'NONE',  ( -45.52287095715007581, -24.83602698348159876, 1.605859176311259295 ) ) ;
#17209 = DIRECTION ( 'NONE',  ( 0.000000000000000000, 1.000000000000000000, -0.000000000000000000 ) ) ;
#17210 = DIRECTION ( 'NONE',  ( 1.000000000000000000, -5.782411586589363555E-16, 0.000000000000000000 ) ) ;
#17211 = CARTESIAN_POINT ( 'NONE',  ( -30.57287095715005876, -24.49485400407631985, 0.5870690654870184266 ) ) ;
#17212 = CC_DESIGN_PERSON_AND_ORGANIZATION_ASSIGNMENT ( #50505, #12924, ( #57555 ) ) ;
#17213 = CARTESIAN_POINT ( 'NONE',  ( 32.95803010956177559, 3.605854314291305762, -13.01399263622904812 ) ) ;
#17214 = CARTESIAN_POINT ( 'NONE',  ( -26.09825057249113556, -24.95872903603973469, 4.796238057267346200 ) ) ;
#17215 = CARTESIAN_POINT ( 'NONE',  ( -90.58953762381672448, -23.48783264082478794, -1.443836473390063713 ) ) ;
#17216 = CARTESIAN_POINT ( 'NONE',  ( -58.64946100639908622, -23.73766607897669800, -1.055555164236457344 ) ) ;
#17217 = ORIENTED_EDGE ( 'NONE', *, *, #89314, .F. ) ;
#17218 = CARTESIAN_POINT ( 'NONE',  ( -2.125485521908593078, 20.27274140177646444, -1.500000000000002220 ) ) ;
#17219 = ORIENTED_EDGE ( 'NONE', *, *, #43311, .F. ) ;
#17220 = VERTEX_POINT ( 'NONE', #89347 ) ;
#17221 = CARTESIAN_POINT ( 'NONE',  ( -22.63010559926462051, 4.001702944626347680, 11.49999999999998934 ) ) ;
#17222 = CARTESIAN_POINT ( 'NONE',  ( -1.488488975859286523, -6.376774720514411854, 19.49847411603315095 ) ) ;
#17224 = ORIENTED_EDGE ( 'NONE', *, *, #25982, .F. ) ;
#17223 = EDGE_CURVE ( 'NONE', #56438, #64548, #91330, .T. ) ;
#17225 = VECTOR ( 'NONE', #75901, 1000.000000000000000 ) ;
#17226 = CARTESIAN_POINT ( 'NONE',  ( -108.5222109042165357, -23.48786465467241413, 11.44779295918253759 ) ) ;
#17227 = DIRECTION ( 'NONE',  ( 0.000000000000000000, -0.8955258983741299916, -0.4450093991605204025 ) ) ;
#17228 = CARTESIAN_POINT ( 'NONE',  ( -98.62287095715005592, -24.66019654487199730, 8.947790411086124607 ) ) ;
#17229 = CARTESIAN_POINT ( 'NONE',  ( -119.2834334325141583, -25.28353533326600555, 5.756556888876060540 ) ) ;
#17231 = ORIENTED_EDGE ( 'NONE', *, *, #41195, .F. ) ;
#17230 = CARTESIAN_POINT ( 'NONE',  ( 10.72677997844354536, -18.41129465587203740, 11.49999999999999645 ) ) ;
#17232 = ORIENTED_EDGE ( 'NONE', *, *, #50651, .F. ) ;
#17233 = CARTESIAN_POINT ( 'NONE',  ( -21.14947813473477822, 6.846651710974520633, -1.500000000000002220 ) ) ;
#17234 = CARTESIAN_POINT ( 'NONE',  ( 7.614520588612671226, -19.20288753073135268, 11.49999999999998934 ) ) ;
#17235 = B_SPLINE_CURVE_WITH_KNOTS ( 'NONE', 3,
 ( #4066, #68334, #42145, #88304 ),
 .UNSPECIFIED., .F., .F.,
 ( 4, 4 ),
 ( 0.000000000000000000, 1.000000000000000000 ),
 .UNSPECIFIED. ) ;
#17236 = ORIENTED_EDGE ( 'NONE', *, *, #94626, .F. ) ;
#17237 = DIRECTION ( 'NONE',  ( -3.773278334444166432E-23, 1.000000000000000000, 0.000000000000000000 ) ) ;
#17238 = CARTESIAN_POINT ( 'NONE',  ( -95.59105585138695460, -24.40133493613050319, 9.663955038902802386 ) ) ;
#17239 = ORIENTED_EDGE ( 'NONE', *, *, #58997, .F. ) ;
#17240 = CARTESIAN_POINT ( 'NONE',  ( -127.6228709571500559, -24.64898659630368627, 1.056161002820834804 ) ) ;
#17241 = ORIENTED_EDGE ( 'NONE', *, *, #44990, .T. ) ;
#17242 = CARTESIAN_POINT ( 'NONE',  ( -58.62774179497608174, -24.51419770103156637, 9.386484678747176957 ) ) ;
#17243 = CARTESIAN_POINT ( 'NONE',  ( -71.09456214124740825, -25.17613501044473878, 6.773754074536313396 ) ) ;
#17244 = CARTESIAN_POINT ( 'NONE',  ( -19.40664508603899563, 7.695215611089875729, -1.500000000000002220 ) ) ;
#17245 = ADVANCED_FACE ( 'NONE', ( #28428 ), #59905, .F. ) ;
#17246 = CARTESIAN_POINT ( 'NONE',  ( -0.06377455873143267340, 21.83884041771831619, 11.49999999999999645 ) ) ;
#17247 = CARTESIAN_POINT ( 'NONE',  ( -89.81226385320383088, -25.22391155068715207, 6.409327647370969494 ) ) ;
#17248 = CARTESIAN_POINT ( 'NONE',  ( 5.087148743171193033, -3.314277014504871222, -27.56324057082087364 ) ) ;
#17249 = CARTESIAN_POINT ( 'NONE',  ( -17.89120377161202313, 13.61666483413312712, 11.49999999999998934 ) ) ;
#17250 = CIRCLE ( 'NONE', #44865, 1.699999999999998401 ) ;
#17251 = CARTESIAN_POINT ( 'NONE',  ( -118.6277898053671578, -23.73791477778912551, 11.05961554403169878 ) ) ;
#17252 = PLANE ( 'NONE',  #51734 ) ;
#17253 = CARTESIAN_POINT ( 'NONE',  ( -59.58953762381674579, -23.47596703998600276, 11.44779298504227505 ) ) ;
#17254 = ORIENTED_EDGE ( 'NONE', *, *, #81840, .F. ) ;
#17255 = EDGE_CURVE ( 'NONE', #28117, #47607, #87306, .T. ) ;
#17256 = ORIENTED_EDGE ( 'NONE', *, *, #56419, .F. ) ;
#17257 = EDGE_LOOP ( 'NONE', ( #56075, #15688, #58228, #74786, #9752, #81278, #30573 ) ) ;
#17258 = EDGE_CURVE ( 'NONE', #47463, #54335, #85053, .T. ) ;
#17259 = CARTESIAN_POINT ( 'NONE',  ( 2.499999999999994671, 18.99999999999977618, 2.100000000000000089 ) ) ;
#17260 = EDGE_LOOP ( 'NONE', ( #89250, #30683, #96846, #93485 ) ) ;
#17261 = VECTOR ( 'NONE', #33063, 1000.000000000000000 ) ;
#17262 = CARTESIAN_POINT ( 'NONE',  ( -7.526967427842778946, 20.06989004931119425, -1.500000000000002220 ) ) ;
#17263 = CARTESIAN_POINT ( 'NONE',  ( 8.681249458320607459, -20.60847208623538762, 11.49999999999999645 ) ) ;
#17264 = ORIENTED_EDGE ( 'NONE', *, *, #75936, .F. ) ;
#17265 = FACE_OUTER_BOUND ( 'NONE', #37069, .T. ) ;
#17266 = AXIS2_PLACEMENT_3D ( 'NONE', #82506, #12990, #43953 ) ;
#17267 = CARTESIAN_POINT ( 'NONE',  ( 20.75205275252385206, -3.532026382766447536, 11.49999999999998934 ) ) ;
#17268 = CARTESIAN_POINT ( 'NONE',  ( -30.47815444756320602, -24.83107907226382238, 8.370654131274083198 ) ) ;
#17269 = CARTESIAN_POINT ( 'NONE',  ( 7.348632388941331861, 18.53259892055224611, -1.500000000000002220 ) ) ;
#17270 = CARTESIAN_POINT ( 'NONE',  ( -50.63858115698904072, -24.52399227489127043, 9.353111116836521077 ) ) ;
#17271 = VECTOR ( 'NONE', #14790, 1000.000000000000000 ) ;
#17272 = DIRECTION ( 'NONE',  ( -1.000000000000000000, 0.000000000000000000, -0.000000000000000000 ) ) ;
#17273 = CARTESIAN_POINT ( 'NONE',  ( -21.42919730060085115, -5.301375089729956969, -1.500000000000002220 ) ) ;
#17274 = ORIENTED_EDGE ( 'NONE', *, *, #44403, .T. ) ;
#17275 = DIRECTION ( 'NONE',  ( -3.773278334453079030E-23, 0.9999999999976377785, 2.173523156925979128E-06 ) ) ;
#17276 = EDGE_CURVE ( 'NONE', #17142, #96497, #73620, .T. ) ;
#17277 = CARTESIAN_POINT ( 'NONE',  ( -121.5228709571500900, -23.94994826722565406, -0.6494450866342689199 ) ) ;
#17278 = CARTESIAN_POINT ( 'NONE',  ( -16.98601802344612111, -12.12340321765213069, 11.49999999999999645 ) ) ;
#17279 = AXIS2_PLACEMENT_3D ( 'NONE', #26188, #4361, #19066 ) ;
#17280 = CARTESIAN_POINT ( 'NONE',  ( 31.62961302973990030, -4.065030569019225659, 27.09489828165477476 ) ) ;
#17281 = CARTESIAN_POINT ( 'NONE',  ( -129.2228709571500644, -23.47596703998600631, 11.44779298504227860 ) ) ;
#17282 = CARTESIAN_POINT ( 'NONE',  ( -119.6228709571500701, -23.48786465467241769, 11.44779295918253759 ) ) ;
#17283 = CARTESIAN_POINT ( 'NONE',  ( -20.14006130340733236, -7.001243683211865410, -1.500000000000002220 ) ) ;
#17284 = CARTESIAN_POINT ( 'NONE',  ( -121.5228709571500616, -24.64965694238408034, 8.947790433994191162 ) ) ;
#17285 = CARTESIAN_POINT ( 'NONE',  ( -51.26173465382703398, -25.25485035848373983, 3.787228214310553120 ) ) ;
#17286 = CARTESIAN_POINT ( 'NONE',  ( -96.52287095715001897, -24.35013146730204525, 9.818937971375097717 ) ) ;
#17287 = CARTESIAN_POINT ( 'NONE',  ( -70.65333586436670998, -25.30188801935125653, 5.302352381037461093 ) ) ;
#17288 = CARTESIAN_POINT ( 'NONE',  ( -9.785633969878258398, 20.35780147342342516, -1.500000000000002220 ) ) ;
#17289 = CARTESIAN_POINT ( 'NONE',  ( -65.05438548721849656, 5.356774720514425603, 23.50402280011858736 ) ) ;
#17290 = ORIENTED_EDGE ( 'NONE', *, *, #90243, .T. ) ;
#17291 = DIRECTION ( 'NONE',  ( 0.000000000000000000, 1.000000000000000000, -0.000000000000000000 ) ) ;
#17292 = CARTESIAN_POINT ( 'NONE',  ( -31.52579011953796950, -24.66019654487199020, 8.947790411086133489 ) ) ;
#17293 = CARTESIAN_POINT ( 'NONE',  ( -10.66912846187372210, -16.51573522771486324, 11.49999999999999645 ) ) ;
#17294 = DIRECTION ( 'NONE',  ( -0.000000000000000000, -1.000000000000000000, -0.000000000000000000 ) ) ;
#17295 = DIRECTION ( 'NONE',  ( 4.335561085774420994E-16, 0.000000000000000000, -1.000000000000000000 ) ) ;
#17296 = ORIENTED_EDGE ( 'NONE', *, *, #33540, .F. ) ;
#17297 = CARTESIAN_POINT ( 'NONE',  ( -111.5228709571500616, -24.64898659630368627, 1.056161002820831474 ) ) ;
#17298 = CARTESIAN_POINT ( 'NONE',  ( -39.55620429048340014, -24.65952944569304606, 1.056160979905692354 ) ) ;
#17299 = CARTESIAN_POINT ( 'NONE',  ( -124.6262003333403925, -23.48786465467241769, 11.44779295918253581 ) ) ;
#17300 = AXIS2_PLACEMENT_3D ( 'NONE', #75757, #30589, #52443 ) ;
#17301 = DIRECTION ( 'NONE',  ( -1.000000000000000000, 0.000000000000000000, 0.000000000000000000 ) ) ;
#17302 = CARTESIAN_POINT ( 'NONE',  ( -107.5228709571500758, -24.64965694238575011, 8.947790433994192938 ) ) ;
#17303 = CARTESIAN_POINT ( 'NONE',  ( 17.05426814964238957, 9.943002105365778220, -1.500000000000002220 ) ) ;
#17304 = VERTEX_POINT ( 'NONE', #97452 ) ;
#17305 = AXIS2_PLACEMENT_3D ( 'NONE', #83912, #14390, #7783 ) ;
#17306 = CARTESIAN_POINT ( 'NONE',  ( 19.60372117168125072, 4.849774137724135237, 11.49999999999999645 ) ) ;
#17307 = CARTESIAN_POINT ( 'NONE',  ( 13.64113475014448440, 6.376774720514426953, -28.24100986136700087 ) ) ;
#17308 = EDGE_CURVE ( 'NONE', #12501, #27247, #47413, .T. ) ;
#17309 = ORIENTED_EDGE ( 'NONE', *, *, #35936, .F. ) ;
#17310 = FACE_OUTER_BOUND ( 'NONE', #76572, .T. ) ;
#17311 = CARTESIAN_POINT ( 'NONE',  ( -65.58953762381672448, -23.48786465467241058, 11.44779295918254647 ) ) ;
#17312 = LINE ( 'NONE', #34051, #65539 ) ;
#17313 = FACE_OUTER_BOUND ( 'NONE', #52575, .T. ) ;
#17314 = B_SPLINE_CURVE_WITH_KNOTS ( 'NONE', 3,
 ( #74957, #29293, #68364, #36410 ),
 .UNSPECIFIED., .F., .F.,
 ( 4, 4 ),
 ( 2.232523134950097154E-11, 0.0004693952269521748277 ),
 .UNSPECIFIED. ) ;
#17315 = PLANE ( 'NONE',  #5192 ) ;
#17316 = LINE ( 'NONE', #88340, #54334 ) ;
#17317 = CARTESIAN_POINT ( 'NONE',  ( 11.47056939498152950, -16.38825109899074661, -1.500000000000002220 ) ) ;
#17318 = B_SPLINE_CURVE_WITH_KNOTS ( 'NONE', 3,
 ( #86560, #31775, #6062, #32269 ),
 .UNSPECIFIED., .F., .F.,
 ( 4, 4 ),
 ( 1.387778780781445521E-17, 9.999999999997510880E-05 ),
 .UNSPECIFIED. ) ;
#17319 = CARTESIAN_POINT ( 'NONE',  ( -117.5895376238167245, -24.64898659630368627, 1.056161002820392270 ) ) ;
#17320 = CARTESIAN_POINT ( 'NONE',  ( 31.48454476783385658, -4.132774720514426292, -1.134026763942596494 ) ) ;
#17321 = VERTEX_POINT ( 'NONE', #66035 ) ;
#17322 = VECTOR ( 'NONE', #57864, 1000.000000000000114 ) ;
#17323 = CARTESIAN_POINT ( 'NONE',  ( 9.747210413488877734, -4.783584857593751849, -26.42012502324587686 ) ) ;
#17324 = CARTESIAN_POINT ( 'NONE',  ( -33.62287095715005592, -23.96127896941631619, -0.6493128931037960294 ) ) ;
#17325 = CARTESIAN_POINT ( 'NONE',  ( -48.55620429048338593, -24.64965694238575011, 8.947790433994207149 ) ) ;
#17326 = CARTESIAN_POINT ( 'NONE',  ( 13.57151214508650305, -9.529487854913506695, 1.500000000000000666 ) ) ;
#17327 = B_SPLINE_CURVE_WITH_KNOTS ( 'NONE', 3,
 ( #95642, #58581, #12882, #51469 ),
 .UNSPECIFIED., .F., .F.,
 ( 4, 4 ),
 ( 0.000000000000000000, 9.999999999998897304E-05 ),
 .UNSPECIFIED. ) ;
#17328 = FACE_OUTER_BOUND ( 'NONE', #77138, .T. ) ;
#17329 = ADVANCED_FACE ( 'NONE', ( #90836 ), #21309, .T. ) ;
#17330 = CARTESIAN_POINT ( 'NONE',  ( -3.108974358974359475, -5.876774720514418071, 20.36458333333334281 ) ) ;
#17332 = CIRCLE ( 'NONE', #23779, 1.999999999999963141 ) ;
#17331 = CARTESIAN_POINT ( 'NONE',  ( 7.160000000000000142, -0.4583917923827244278, 5.886156785137588443 ) ) ;
#17333 = ORIENTED_EDGE ( 'NONE', *, *, #76562, .F. ) ;
#17334 = EDGE_CURVE ( 'NONE', #73864, #55923, #38967, .T. ) ;
#17335 = AXIS2_PLACEMENT_3D ( 'NONE', #85138, #70426, #93249 ) ;
#17336 = CARTESIAN_POINT ( 'NONE',  ( -8.348131891436525009, -18.51812344263101906, 11.49999999999998934 ) ) ;
#17337 = CARTESIAN_POINT ( 'NONE',  ( 29.58033090225963591, 3.719533051881441121, 29.19816577366266941 ) ) ;
#17338 = CARTESIAN_POINT ( 'NONE',  ( -34.49704148459657205, -24.15543982623907127, -0.2315651400026575435 ) ) ;
#17339 = EDGE_CURVE ( 'NONE', #62723, #74207, #42686, .T. ) ;
#17340 = PLANE ( 'NONE',  #16836 ) ;
#17341 = EDGE_CURVE ( 'NONE', #5284, #46688, #6096, .T. ) ;
#17342 = ORIENTED_EDGE ( 'NONE', *, *, #88179, .F. ) ;
#17343 = CARTESIAN_POINT ( 'NONE',  ( 0.000000000000000000, -16.94322527948557422, 0.000000000000000000 ) ) ;
#17344 = CARTESIAN_POINT ( 'NONE',  ( -19.98115086844608612, 2.773124471107000666, -1.500000000000002220 ) ) ;
#17345 = CARTESIAN_POINT ( 'NONE',  ( -7.741094375770895653, -19.69850519626218599, 11.49999999999999645 ) ) ;
#17346 = EDGE_CURVE ( 'NONE', #78854, #61182, #35393, .T. ) ;
#17347 = CARTESIAN_POINT ( 'NONE',  ( -21.57569705560537088, 4.917917830663471435, 11.49999999999998934 ) ) ;
#17348 = CARTESIAN_POINT ( 'NONE',  ( -11.90445915685808131, 16.78794160864392992, -1.500000000000002220 ) ) ;
#17349 = DIRECTION ( 'NONE',  ( 1.000000000000000000, 0.000000000000000000, 0.000000000000000000 ) ) ;
#17350 = ORIENTED_EDGE ( 'NONE', *, *, #89177, .F. ) ;
#17351 = CARTESIAN_POINT ( 'NONE',  ( -43.52287095715007581, -23.94994826722564696, -0.6494450866342739159 ) ) ;
#17352 = ORIENTED_EDGE ( 'NONE', *, *, #64836, .T. ) ;
#17353 = LINE ( 'NONE', #18357, #65769 ) ;
#17354 = CARTESIAN_POINT ( 'NONE',  ( -61.62287095715007723, -24.51387760970724017, 9.387446482453425389 ) ) ;
#17355 = ORIENTED_EDGE ( 'NONE', *, *, #2250, .F. ) ;
#17356 = ORIENTED_EDGE ( 'NONE', *, *, #52294, .F. ) ;
#17357 =( BOUNDED_SURFACE ( )  B_SPLINE_SURFACE ( 3, 2, ( 
 ( #83456, #52026, #74356 ),
 ( #5843, #36302, #29677 ),
 ( #51531, #60152, #59648 ),
 ( #91568, #91073, #4849 ),
 ( #20561, #81974, #13944 ),
 ( #12454, #43913, #97692 ) ),
 .UNSPECIFIED., .F., .F., .F. ) 
 B_SPLINE_SURFACE_WITH_KNOTS ( ( 4, 2, 4 ),
 ( 3, 3 ),
 ( 0.04217399329892001364, 0.04576393237407583303, 0.04935387144923164549 ),
 ( 0.000000000000000000, 1.000000000000000000 ),
 .UNSPECIFIED. ) 
 GEOMETRIC_REPRESENTATION_ITEM ( )  RATIONAL_B_SPLINE_SURFACE ( (
 ( 1.000000000000000000, 0.7071067811865475727, 1.000000000000000000),
 ( 1.000000000000000000, 0.7325703083253984893, 1.000000000000000000),
 ( 1.000000000000000000, 0.7567337024450505600, 1.000000000000000000),
 ( 1.000000000000000000, 0.8025768260704856383, 1.000000000000000000),
 ( 1.000000000000000000, 0.8242588182985012280, 1.000000000000000000),
 ( 1.000000000000000000, 0.8446854842613638059, 1.000000000000000000) ) ) 
 REPRESENTATION_ITEM ( '' )  SURFACE ( )  );
#17358 = ORIENTED_EDGE ( 'NONE', *, *, #69600, .T. ) ;
#17359 = CARTESIAN_POINT ( 'NONE',  ( -100.5228709571500758, -24.62226745350440282, 0.9660975649728090753 ) ) ;
#17360 = CARTESIAN_POINT ( 'NONE',  ( 6.586338672804227024, -6.376774720514415407, 20.10086663068103618 ) ) ;
#17361 = CARTESIAN_POINT ( 'NONE',  ( 5.786755829966409692, -5.876774720514413630, 19.89762986309224857 ) ) ;
#17362 = CARTESIAN_POINT ( 'NONE',  ( -1.398219401198234957, 20.63772364298462847, -1.500000000000002220 ) ) ;
#17363 = EDGE_CURVE ( 'NONE', #48335, #79051, #89838, .T. ) ;
#17364 = CARTESIAN_POINT ( 'NONE',  ( -14.16021466491576675, 16.42052772630311352, 11.49999999999999645 ) ) ;
#17365 = ORIENTED_EDGE ( 'NONE', *, *, #30265, .T. ) ;
#17366 = DIRECTION ( 'NONE',  ( 0.000000000000000000, 1.000000000000000000, 0.000000000000000000 ) ) ;
#17367 = VECTOR ( 'NONE', #42239, 1000.000000000000000 ) ;
#17368 = DIRECTION ( 'NONE',  ( 0.000000000000000000, 0.000000000000000000, 1.000000000000000000 ) ) ;
#17369 = CARTESIAN_POINT ( 'NONE',  ( 11.64234319522276095, -19.14997049866658330, -1.500000000000002220 ) ) ;
#17370 = CARTESIAN_POINT ( 'NONE',  ( -47.48886131524788112, -24.51419770103156637, 9.386484678747176957 ) ) ;
#17371 = CARTESIAN_POINT ( 'NONE',  ( -75.62287095715004170, -29.50248789122583659, 2.256150453626215580 ) ) ;
#17372 = ORIENTED_EDGE ( 'NONE', *, *, #74387, .T. ) ;
#17373 = CARTESIAN_POINT ( 'NONE',  ( -31.62287095715006657, -23.73934037231756378, 11.05740245334329863 ) ) ;
#17374 = CARTESIAN_POINT ( 'NONE',  ( -76.62287095715007013, -23.47596703998600631, 11.44779298504227860 ) ) ;
#17375 = ORIENTED_EDGE ( 'NONE', *, *, #18637, .F. ) ;
#17376 = ORIENTED_EDGE ( 'NONE', *, *, #2578, .T. ) ;
#17378 = EDGE_CURVE ( 'NONE', #78138, #93719, #67024, .T. ) ;
#17377 = DIRECTION ( 'NONE',  ( -1.000000000000000000, -3.773278334444167608E-23, -8.201307833595939069E-29 ) ) ;
#17379 = ORIENTED_EDGE ( 'NONE', *, *, #49467, .T. ) ;
#17380 = CARTESIAN_POINT ( 'NONE',  ( 26.73860345374794178, -5.356774720496559894, 19.84760796525321425 ) ) ;
#17381 = CARTESIAN_POINT ( 'NONE',  ( 3.302162439418223627, -20.95225242093645690, -1.500000000000002220 ) ) ;
#17382 = EDGE_CURVE ( 'NONE', #40608, #60813, #39049, .T. ) ;
#17383 = ORIENTED_EDGE ( 'NONE', *, *, #96285, .T. ) ;
#17384 = CARTESIAN_POINT ( 'NONE',  ( -50.62889416934638120, -24.83618233451450408, 1.606449574219538601 ) ) ;
#17385 = CARTESIAN_POINT ( 'NONE',  ( -1.534710021792092594, -21.76038796025502009, 11.49999999999998934 ) ) ;
#17386 = CARTESIAN_POINT ( 'NONE',  ( -52.62368459130443199, -24.66019654487198665, 8.947790411086131712 ) ) ;
#17387 = CARTESIAN_POINT ( 'NONE',  ( -121.5228709571500616, -29.50250243563736774, 8.947779886222134493 ) ) ;
#17388 = CARTESIAN_POINT ( 'NONE',  ( -75.62287095715005592, -25.00158670708909625, 2.256160236439166855 ) ) ;
#17389 = CARTESIAN_POINT ( 'NONE',  ( 0.003323472525107682655, -21.86402403546210493, -1.500000000000002220 ) ) ;
#17390 = CARTESIAN_POINT ( 'NONE',  ( -30.57287095715006942, -25.14801120426701075, 3.036021546538907323 ) ) ;
#17391 = ORIENTED_EDGE ( 'NONE', *, *, #81511, .F. ) ;
#17392 = CARTESIAN_POINT ( 'NONE',  ( 22.81105451610979173, -500000.0000000000582, -16.21691820600746681 ) ) ;
#17393 = CARTESIAN_POINT ( 'NONE',  ( -85.58929132145466667, -24.52399227489127043, 9.353111116836526406 ) ) ;
#17395 = VERTEX_POINT ( 'NONE', #93327 ) ;
#17394 = EDGE_CURVE ( 'NONE', #92240, #95461, #69997, .T. ) ;
#17396 = AXIS2_PLACEMENT_3D ( 'NONE', #29396, #75559, #66986 ) ;
#17397 = ADVANCED_FACE ( 'NONE', ( #99436 ), #23817, .T. ) ;
#17398 = ORIENTED_EDGE ( 'NONE', *, *, #49694, .T. ) ;
#17399 = EDGE_CURVE ( 'NONE', #42451, #43735, #8607, .T. ) ;
#17400 = ORIENTED_EDGE ( 'NONE', *, *, #97466, .T. ) ;
#17401 = PLANE ( 'NONE',  #10287 ) ;
#17402 = CARTESIAN_POINT ( 'NONE',  ( -113.6228709571500559, -24.34917612406837861, 0.1852690917426704775 ) ) ;
#17403 = CARTESIAN_POINT ( 'NONE',  ( 20.49604761983493972, 5.601127818285958071, 11.49999999999998934 ) ) ;
#17404 = PLANE ( 'NONE',  #51537 ) ;
#17405 = DIRECTION ( 'NONE',  ( 3.773278334444166432E-23, -1.000000000000000000, 0.000000000000000000 ) ) ;
#17406 = LINE ( 'NONE', #72707, #17840 ) ;
#17407 = VECTOR ( 'NONE', #8375, 1000.000000000000000 ) ;
#17408 = DIRECTION ( 'NONE',  ( 0.000000000000000000, 0.000000000000000000, 1.000000000000000000 ) ) ;
#17409 = CARTESIAN_POINT ( 'NONE',  ( 0.06232057257353295493, 19.38168652127415825, 11.49999999999998934 ) ) ;
#17410 = CARTESIAN_POINT ( 'NONE',  ( -45.48405291254921679, -24.63355581998386867, 0.9682620441943888823 ) ) ;
#17411 = ORIENTED_EDGE ( 'NONE', *, *, #6348, .F. ) ;
#17412 = CARTESIAN_POINT ( 'NONE',  ( -6.230579426152004885, -18.48807627814308674, 11.49999999999999645 ) ) ;
#17413 = CARTESIAN_POINT ( 'NONE',  ( -5.576923076923076650, -5.876774720514417183, 20.44941907051282470 ) ) ;
#17414 = AXIS2_PLACEMENT_3D ( 'NONE', #29127, #5294, #21500 ) ;
#17415 = B_SPLINE_CURVE_WITH_KNOTS ( 'NONE', 3,
 ( #63125, #16417, #1216, #30659, #55008 ),
 .UNSPECIFIED., .F., .F.,
 ( 4, 1, 4 ),
 ( 0.000000000000000000, 0.5126593363417801807, 0.9999999999999998890 ),
 .UNSPECIFIED. ) ;
#17416 = CARTESIAN_POINT ( 'NONE',  ( -47.52287095715006160, -29.50250786944525672, 11.44777988621624054 ) ) ;
#17417 = ORIENTED_EDGE ( 'NONE', *, *, #78059, .T. ) ;
#17418 = CARTESIAN_POINT ( 'NONE',  ( -103.5562042904834072, -23.47596703998600631, 11.44779298504227683 ) ) ;
#17419 = CARTESIAN_POINT ( 'NONE',  ( -119.6228709571500559, -24.64965695001469115, 8.947790433994175174 ) ) ;
#17420 = DIRECTION ( 'NONE',  ( 0.000000000000000000, 0.000000000000000000, 1.000000000000000000 ) ) ;
#17421 = CARTESIAN_POINT ( 'NONE',  ( -80.77473702827948898, -25.03156056331435408, 7.542257620978359611 ) ) ;
#17422 = CARTESIAN_POINT ( 'NONE',  ( -19.44079195400435012, 3.002763184081948200, 11.49999999999998934 ) ) ;
#17423 = VERTEX_POINT ( 'NONE', #14197 ) ;
#17424 = CARTESIAN_POINT ( 'NONE',  ( -7.777949202540602514, -10.53666143673956768, 1.254198837351630402 ) ) ;
#17425 = CARTESIAN_POINT ( 'NONE',  ( -10.32085834726444595, 20.65377284989807194, -1.500000000000002220 ) ) ;
#17426 = COORDINATED_UNIVERSAL_TIME_OFFSET ( 0, 0, .AHEAD. ) ;
#17427 = CARTESIAN_POINT ( 'NONE',  ( 3.296548071537245495, -5.876774720514425177, 21.29143507544719682 ) ) ;
#17428 = FACE_OUTER_BOUND ( 'NONE', #93127, .T. ) ;
#17429 = CARTESIAN_POINT ( 'NONE',  ( -105.5895376238167387, -23.48786465467241769, 11.44779295918253759 ) ) ;
#17430 = CARTESIAN_POINT ( 'NONE',  ( -97.63001551305060843, -24.15620529776629155, 10.23563542870660115 ) ) ;
#17431 = DIRECTION ( 'NONE',  ( 0.000000000000000000, 2.173523156925980399E-06, -0.9999999999976378895 ) ) ;
#17432 = LINE ( 'NONE', #19799, #31183 ) ;
#17433 = CARTESIAN_POINT ( 'NONE',  ( -129.6236598164479403, -24.15543982623907837, -0.2315651400026527140 ) ) ;
#17434 = CARTESIAN_POINT ( 'NONE',  ( -0.02075734969026423599, -0.3587747205144213303, -0.08597719988137648983 ) ) ;
#17435 = CARTESIAN_POINT ( 'NONE',  ( -17.57349146297605103, 9.389787994052484876, 11.49999999999998934 ) ) ;
#17436 = CARTESIAN_POINT ( 'NONE',  ( -101.1706393923740848, -25.23780489406441419, 3.628358869520814434 ) ) ;
#17437 = CARTESIAN_POINT ( 'NONE',  ( -15.05033210666397103, 12.90603908704162173, -1.500000000000002220 ) ) ;
#17438 = ORIENTED_EDGE ( 'NONE', *, *, #97352, .T. ) ;
#17439 = DIRECTION ( 'NONE',  ( 0.000000000000000000, -2.173523156925979552E-06, 0.9999999999976378895 ) ) ;
#17440 = CARTESIAN_POINT ( 'NONE',  ( -50.93420549988994139, -25.14762240475955579, 7.017504830804345062 ) ) ;
#17441 = CARTESIAN_POINT ( 'NONE',  ( -42.52287095715005449, -23.47593901973090169, -1.443836447538997092 ) ) ;
#17442 = CARTESIAN_POINT ( 'NONE',  ( 15.70846742882596025, 13.54617332914617478, 11.49999999999999645 ) ) ;
#17443 = DIRECTION ( 'NONE',  ( 0.000000000000000000, 1.000000000000000000, -0.000000000000000000 ) ) ;
#17444 = CARTESIAN_POINT ( 'NONE',  ( -2.768609665556980293, 0.3587747205144057872, -29.41086200512614823 ) ) ;
#17445 = CARTESIAN_POINT ( 'NONE',  ( 22.80427751693360960, 0.003464389817739472934, 11.49999999999999645 ) ) ;
#17447 = EDGE_CURVE ( 'NONE', #21027, #32109, #20802, .T. ) ;
#17446 = ORIENTED_EDGE ( 'NONE', *, *, #20572, .T. ) ;
#17448 = B_SPLINE_SURFACE_WITH_KNOTS ( 'NONE', 3, 3, ( 
 ( #22840, #61939, #85767, #62438 ),
 ( #54331, #85257, #23856, #46714 ),
 ( #54832, #10648, #25869, #18746 ),
 ( #48728, #56342, #41106, #26870 ),
 ( #49230, #50214, #81659, #4040 ),
 ( #33984, #26371, #95380, #41610 ),
 ( #72062, #10144, #96379, #50709 ) ),
 .UNSPECIFIED., .F., .F., .F.,
 ( 4, 3, 4 ),
 ( 4, 4 ),
 ( 0.0004766839783834151811, 0.1029713700210900668, 0.2054660560637967259 ),
 ( 0.9197279603282626503, 0.9211650456752530358 ),
 .UNSPECIFIED. ) ;
#17449 = CARTESIAN_POINT ( 'NONE',  ( -69.58397737201534028, -24.51314013834315375, 0.6176544820404143987 ) ) ;
#17450 = PLANE ( 'NONE',  #66320 ) ;
#17451 = ORIENTED_EDGE ( 'NONE', *, *, #48666, .T. ) ;
#17452 = CARTESIAN_POINT ( 'NONE',  ( -2.107266074560359748, -20.09985696230311447, 11.49999999999998934 ) ) ;
#17453 = CARTESIAN_POINT ( 'NONE',  ( -106.5228709571500332, -23.73934037231757443, 11.05740245334327732 ) ) ;
#17454 = CARTESIAN_POINT ( 'NONE',  ( -114.6228709571500559, -24.66019654487199730, 8.947790411086122830 ) ) ;
#17455 = EDGE_CURVE ( 'NONE', #31222, #32160, #42925, .T. ) ;
#17456 = EDGE_CURVE ( 'NONE', #13848, #91650, #80122, .T. ) ;
#17457 = VECTOR ( 'NONE', #86683, 1000.000000000000114 ) ;
#17458 = EDGE_CURVE ( 'NONE', #25716, #30457, #54790, .T. ) ;
#17459 = ORIENTED_EDGE ( 'NONE', *, *, #13451, .F. ) ;
#17460 = CARTESIAN_POINT ( 'NONE',  ( -70.62287095715007013, -23.47596703998600631, 11.44779298504227505 ) ) ;
#17461 = CARTESIAN_POINT ( 'NONE',  ( -51.62287095715008434, -24.34917612406837861, 0.1852690917426609851 ) ) ;
#17462 = CARTESIAN_POINT ( 'NONE',  ( 13.87436705529610492, 14.39054836566213780, -1.500000000000002220 ) ) ;
#17463 = DIRECTION ( 'NONE',  ( -1.000000000000000000, 0.000000000000000000, 0.000000000000000000 ) ) ;
#17464 = CARTESIAN_POINT ( 'NONE',  ( -18.08314111433443827, -10.61732331186343004, 11.49999999999999645 ) ) ;
#17465 = EDGE_CURVE ( 'NONE', #26092, #95938, #43818, .T. ) ;
#17466 = FACE_OUTER_BOUND ( 'NONE', #86402, .T. ) ;
#17467 = DIRECTION ( 'NONE',  ( 0.000000000000000000, 0.000000000000000000, -1.000000000000000000 ) ) ;
#17468 = CARTESIAN_POINT ( 'NONE',  ( -8.753671783739276790, -20.25744411100385634, -1.500000000000002220 ) ) ;
#17469 = VECTOR ( 'NONE', #83370, 1000.000000000000114 ) ;
#17470 = CARTESIAN_POINT ( 'NONE',  ( 282.9764569301858046, 4.540774720514427543, 20.79159422840526616 ) ) ;
#17471 = VERTEX_POINT ( 'NONE', #46168 ) ;
#17472 = CARTESIAN_POINT ( 'NONE',  ( 2.499999999999993783, 4.999999999999997335, 2.100000000000000089 ) ) ;
#17473 = CARTESIAN_POINT ( 'NONE',  ( -118.5228709571501184, -24.51387760970726504, 9.387446482453404073 ) ) ;
#17474 = CARTESIAN_POINT ( 'NONE',  ( -81.62287095715005592, -29.50247984919015209, -1.443849546365053582 ) ) ;
#17475 = ORIENTED_EDGE ( 'NONE', *, *, #24533, .T. ) ;
#17476 = DIRECTION ( 'NONE',  ( 0.000000000000000000, 1.000000000000000000, 0.000000000000000000 ) ) ;
#17477 = ORIENTED_EDGE ( 'NONE', *, *, #66629, .T. ) ;
#17478 = AXIS2_PLACEMENT_3D ( 'NONE', #62354, #68956, #30387 ) ;
#17479 = EDGE_LOOP ( 'NONE', ( #80406, #27833, #8015, #80902 ) ) ;
#17480 = CARTESIAN_POINT ( 'NONE',  ( -78.92287095715010992, -23.47593901973090524, -1.443836447538997980 ) ) ;
#17481 = FACE_OUTER_BOUND ( 'NONE', #84862, .T. ) ;
#17482 = CARTESIAN_POINT ( 'NONE',  ( -122.6228709571500417, -23.48786465467242124, 11.44779295918253759 ) ) ;
#17483 = CARTESIAN_POINT ( 'NONE',  ( -20.49763986188970932, -1.003951800832726615, -1.500000000000002220 ) ) ;
#17484 = EDGE_CURVE ( 'NONE', #26765, #55186, #24405, .T. ) ;
#17485 = EDGE_LOOP ( 'NONE', ( #98872, #2665, #49966, #57724 ) ) ;
#17486 = CARTESIAN_POINT ( 'NONE',  ( -71.62287095715005592, -23.48786465467241413, 11.44779295918254469 ) ) ;
#17487 = CARTESIAN_POINT ( 'NONE',  ( 7.010993867624484288, -5.876774720514418071, 20.34381700913260715 ) ) ;
#17488 = CARTESIAN_POINT ( 'NONE',  ( 30.09341516180546350, -1.682774720514426114, -11.39311774897855933 ) ) ;
#17489 = CARTESIAN_POINT ( 'NONE',  ( -16.35649155429130985, -15.18990082740072367, 11.49999999999998934 ) ) ;
#17490 = CARTESIAN_POINT ( 'NONE',  ( -0.008165992925886831136, -22.94428480439657392, 3.856996771331003160 ) ) ;
#17491 = LINE ( 'NONE', #46950, #72328 ) ;
#17492 = EDGE_CURVE ( 'NONE', #39531, #62936, #98257, .T. ) ;
#17493 = ORIENTED_EDGE ( 'NONE', *, *, #59986, .F. ) ;
#17494 = CARTESIAN_POINT ( 'NONE',  ( -20.27875734969026311, 5.356774720514425603, 24.00402280011862288 ) ) ;
#17495 = DIRECTION ( 'NONE',  ( -0.000000000000000000, 1.000000000000000000, 1.020425574104004246E-16 ) ) ;
#17496 = VECTOR ( 'NONE', #48898, 1000.000000000000000 ) ;
#17497 = CARTESIAN_POINT ( 'NONE',  ( -0.6367455441941621830, -20.85161220577290919, 11.49999999999998934 ) ) ;
#17498 = ORIENTED_EDGE ( 'NONE', *, *, #54021, .T. ) ;
#17501 = ORIENTED_EDGE ( 'NONE', *, *, #26756, .F. ) ;
#17500 = EDGE_CURVE ( 'NONE', #91978, #29751, #31942, .T. ) ;
#17499 = CARTESIAN_POINT ( 'NONE',  ( 0.000000000000000000, -4.056774720514426669, 0.000000000000000000 ) ) ;
#17502 = ORIENTED_EDGE ( 'NONE', *, *, #65379, .T. ) ;
#17503 = B_SPLINE_CURVE_WITH_KNOTS ( 'NONE', 3,
 ( #67941, #52706, #22727, #23234 ),
 .UNSPECIFIED., .F., .F.,
 ( 4, 4 ),
 ( 0.000000000000000000, 0.0001000000000000028644 ),
 .UNSPECIFIED. ) ;
#17504 = DIRECTION ( 'NONE',  ( -0.000000000000000000, 1.000000000000000000, -0.000000000000000000 ) ) ;
#17505 = CARTESIAN_POINT ( 'NONE',  ( 12.48895993392301307, -16.95307763291877379, -1.500000000000002220 ) ) ;
#17506 = ORIENTED_EDGE ( 'NONE', *, *, #21802, .F. ) ;
#17507 = CARTESIAN_POINT ( 'NONE',  ( -37.55620429048341435, -24.64965694238574656, 8.947790433994205372 ) ) ;
#17508 = CARTESIAN_POINT ( 'NONE',  ( 5.105333984060716368, -3.311071866383498374, -27.56005651598365347 ) ) ;
#17509 = FACE_OUTER_BOUND ( 'NONE', #2033, .T. ) ;
#17510 = CARTESIAN_POINT ( 'NONE',  ( -101.9401486745561272, -25.25419277357474712, 6.289339016573623375 ) ) ;
#17511 = CARTESIAN_POINT ( 'NONE',  ( -59.49823463814401237, -24.34968618360933235, 0.1864209137778795600 ) ) ;
#17512 = CARTESIAN_POINT ( 'NONE',  ( -109.0819061167040047, -25.31465039088007174, 4.788656490444584080 ) ) ;
#17513 = CARTESIAN_POINT ( 'NONE',  ( 13.91401389203221406, 5.965225279485572685, 158.0376437107427137 ) ) ;
#17515 = VERTEX_POINT ( 'NONE', #47174 ) ;
#17514 = CARTESIAN_POINT ( 'NONE',  ( -21.61287440533560300, 5.199345243644041936, 11.49999999999999645 ) ) ;
#17516 = CARTESIAN_POINT ( 'NONE',  ( -120.5228709571500616, -29.50250786944525672, 11.44777988621622811 ) ) ;
#17517 = CARTESIAN_POINT ( 'NONE',  ( -37.52287095715006870, -23.48786465467240347, 11.44779295918255180 ) ) ;
#17518 = ORIENTED_EDGE ( 'NONE', *, *, #82545, .T. ) ;
#17519 = B_SPLINE_CURVE_WITH_KNOTS ( 'NONE', 3,
 ( #38739, #70200, #31630, #61609 ),
 .UNSPECIFIED., .F., .F.,
 ( 4, 4 ),
 ( 0.000000000000000000, 9.999999999998206125E-05 ),
 .UNSPECIFIED. ) ;
#17520 = CARTESIAN_POINT ( 'NONE',  ( 17.73637878876437668, -14.10177982315242318, 11.49999999999998934 ) ) ;
#17521 = ADVANCED_FACE ( 'NONE', ( #994 ), #84672, .T. ) ;
#17523 = ORIENTED_EDGE ( 'NONE', *, *, #41772, .F. ) ;
#17522 = DIRECTION ( 'NONE',  ( -3.773278334453079030E-23, 0.9999999999976377785, 2.173523156925979128E-06 ) ) ;
#17524 = ORIENTED_EDGE ( 'NONE', *, *, #97679, .F. ) ;
#17525 = CARTESIAN_POINT ( 'NONE',  ( -2.872281323269014752, -1.473225279485573358, 1.999999999999999556 ) ) ;
#17526 = ADVANCED_FACE ( 'NONE', ( #31437 ), #62912, .T. ) ;
#17527 = CARTESIAN_POINT ( 'NONE',  ( -17.16780662754360520, -10.58209718439171176, 11.49999999999998934 ) ) ;
#17528 = CARTESIAN_POINT ( 'NONE',  ( -105.5228709571501184, -24.15431212366389957, -0.2830839119429224837 ) ) ;
#17529 = ORIENTED_EDGE ( 'NONE', *, *, #74867, .T. ) ;
#17530 = DIRECTION ( 'NONE',  ( 0.000000000000000000, 0.000000000000000000, -1.000000000000000000 ) ) ;
#17531 = CARTESIAN_POINT ( 'NONE',  ( -14.11974515630795501, -17.41659395067913962, -1.500000000000002220 ) ) ;
#17532 = ORIENTED_EDGE ( 'NONE', *, *, #61716, .T. ) ;
#17533 = VERTEX_POINT ( 'NONE', #76594 ) ;
#17534 = CARTESIAN_POINT ( 'NONE',  ( -112.6299582353932607, -23.73791477778912551, 11.05961554403169878 ) ) ;
#17535 = CARTESIAN_POINT ( 'NONE',  ( -4.465079497292244959, -6.376774720514410077, 19.29815762497054976 ) ) ;
#17536 = CARTESIAN_POINT ( 'NONE',  ( -61.52287095715006160, -23.47596703998600631, 11.44779298504228926 ) ) ;
#17537 = CARTESIAN_POINT ( 'NONE',  ( -98.62287095715005592, -29.50247984919015209, -1.443849546365050029 ) ) ;
#17538 = VECTOR ( 'NONE', #41911, 1000.000000000000114 ) ;
#17539 = CARTESIAN_POINT ( 'NONE',  ( 13.10664265030973930, 5.965225279485574461, -28.64597719988137570 ) ) ;
#17540 = CARTESIAN_POINT ( 'NONE',  ( -0.9579564967699066846, 19.55851204243107233, 11.49999999999998934 ) ) ;
#17541 = CARTESIAN_POINT ( 'NONE',  ( -49.97243670601686460, -25.31053666847986960, 4.650320011491689165 ) ) ;
#17542 = ORIENTED_EDGE ( 'NONE', *, *, #86548, .T. ) ;
#17543 = CARTESIAN_POINT ( 'NONE',  ( -0.7226137440361984909, -21.50112622129444162, 11.49999999999998934 ) ) ;
#17544 = B_SPLINE_CURVE_WITH_KNOTS ( 'NONE', 3,
 ( #17460, #78346, #47418, #24563, #1743, #26074, #72266, #2754 ),
 .UNSPECIFIED., .F., .F.,
 ( 4, 2, 2, 4 ),
 ( 0.000000000000000000, 0.002001079623178223660, 0.003001619434767337224, 0.004002159246356450789 ),
 .UNSPECIFIED. ) ;
#17545 = PLANE ( 'NONE',  #41479 ) ;
#17546 = CARTESIAN_POINT ( 'NONE',  ( -121.5228709571500474, -24.34917612406837151, 0.1852690917426603190 ) ) ;
#17547 = CARTESIAN_POINT ( 'NONE',  ( -123.5228709571501184, -24.66019654487200441, 8.947790411086105067 ) ) ;
#17548 = DIRECTION ( 'NONE',  ( -0.000000000000000000, 1.000000000000000000, -0.000000000000000000 ) ) ;
#17549 = CARTESIAN_POINT ( 'NONE',  ( 21.13568926591755925, -8.834425160694816981, -1.500000000000002220 ) ) ;
#17550 = AXIS2_PLACEMENT_3D ( 'NONE', #38082, #69036, #84757 ) ;
#17551 = PERSON_AND_ORGANIZATION_ROLE ( 'creator' ) ;
#17552 = B_SPLINE_CURVE_WITH_KNOTS ( 'NONE', 3,
 ( #53468, #30105, #91503, #84893 ),
 .UNSPECIFIED., .F., .F.,
 ( 4, 4 ),
 ( 0.000000000000000000, 9.999999999998206125E-05 ),
 .UNSPECIFIED. ) ;
#17553 = CARTESIAN_POINT ( 'NONE',  ( -4.141025641025640525, -6.376774720514418959, 20.67377804487179915 ) ) ;
#17554 = PLANE ( 'NONE',  #47423 ) ;
#17555 = CARTESIAN_POINT ( 'NONE',  ( -19.91332876899582160, 2.521106391696132931, 11.49999999999999645 ) ) ;
#17556 = CARTESIAN_POINT ( 'NONE',  ( 1.000208336950358934, 0.000000000000000000, 0.000000000000000000 ) ) ;
#17557 = CARTESIAN_POINT ( 'NONE',  ( 1.876957540558651605, -5.558144974487054135, 0.000000000000000000 ) ) ;
#17558 = AXIS2_PLACEMENT_3D ( 'NONE', #42681, #74601, #5094 ) ;
#17559 = CARTESIAN_POINT ( 'NONE',  ( -88.62287095715004170, -23.47593901973091235, -1.443836447539002865 ) ) ;
#17560 = LINE ( 'NONE', #1346, #34326 ) ;
#17561 = DIRECTION ( 'NONE',  ( -3.773278334453079030E-23, 0.9999999999976377785, 2.173523156925979128E-06 ) ) ;
#17562 = CARTESIAN_POINT ( 'NONE',  ( 19.75055111929153639, -1.948201398878238066, -1.500000000000002220 ) ) ;
#17563 = CARTESIAN_POINT ( 'NONE',  ( 11.36066313177254905, -18.55813952095733654, -1.500000000000002220 ) ) ;
#17564 = CARTESIAN_POINT ( 'NONE',  ( 4.878909776184770742E-15, -6.376774720514426953, 22.50000000000000355 ) ) ;
#17565 = CARTESIAN_POINT ( 'NONE',  ( 13.00645856128228495, 14.71372164842801844, -1.500000000000002220 ) ) ;
#17566 = CARTESIAN_POINT ( 'NONE',  ( 16.09828331921171696, -3.622774695106080411, -27.82448843548682405 ) ) ;
#17567 = CARTESIAN_POINT ( 'NONE',  ( -121.6228709571500559, -23.47596703998600631, 11.44779298504227683 ) ) ;
#17568 = DIRECTION ( 'NONE',  ( -0.000000000000000000, 0.000000000000000000, 1.000000000000000000 ) ) ;
#17569 = CARTESIAN_POINT ( 'NONE',  ( 2.611202098145462891, -5.876774720514420736, 20.45574432200782766 ) ) ;
#17570 = CARTESIAN_POINT ( 'NONE',  ( 17.96566822227200433, 9.963707542159163211, 11.49999999999999645 ) ) ;
#17571 = CARTESIAN_POINT ( 'NONE',  ( 4.595037417369686850, -6.376774720514420736, 20.70846556543617467 ) ) ;
#17572 = CARTESIAN_POINT ( 'NONE',  ( -47.62287095715004170, -23.73907113216990794, -1.053371485793233697 ) ) ;
#17573 = CARTESIAN_POINT ( 'NONE',  ( 15.88279217892459094, 16.07415641707351384, 11.49999999999999645 ) ) ;
#17574 = ORIENTED_EDGE ( 'NONE', *, *, #16602, .T. ) ;
#17575 = CARTESIAN_POINT ( 'NONE',  ( -45.52287095715006160, -29.50249982740957577, 7.747779886224967605 ) ) ;
#17576 = FACE_OUTER_BOUND ( 'NONE', #47350, .T. ) ;
#17578 = EDGE_CURVE ( 'NONE', #4203, #57442, #69047, .T. ) ;
#17577 = CARTESIAN_POINT ( 'NONE',  ( -97.51608943600319890, -23.96119346886881374, -0.6495511937832056937 ) ) ;
#17579 = CARTESIAN_POINT ( 'NONE',  ( -27.54213053348642504, -24.77237661284991432, 2.282611211521436534 ) ) ;
#17580 = EDGE_CURVE ( 'NONE', #93616, #30931, #93406, .T. ) ;
#17581 = DIRECTION ( 'NONE',  ( 7.960204194457801640E-17, 1.000000000000000000, 0.000000000000000000 ) ) ;
#17582 = EDGE_CURVE ( 'NONE', #16907, #44949, #24321, .T. ) ;
#17583 = DIRECTION ( 'NONE',  ( -3.773278334453079618E-23, 0.9999999999976377785, 2.173523156925979975E-06 ) ) ;
#17584 = EDGE_CURVE ( 'NONE', #8126, #34234, #63918, .T. ) ;
#17585 = EDGE_LOOP ( 'NONE', ( #75689, #43862, #36169, #85197 ) ) ;
#17586 = CARTESIAN_POINT ( 'NONE',  ( -79.41916052885848387, -25.26750005083801653, 5.559759467608911265 ) ) ;
#17587 = CARTESIAN_POINT ( 'NONE',  ( 16.54545882101025711, 15.75737887292823558, 11.49999999999998934 ) ) ;
#17588 = DIRECTION ( 'NONE',  ( -0.6451914333552788428, 0.000000000000000000, -0.7640209514960704107 ) ) ;
#17589 = B_SPLINE_CURVE_WITH_KNOTS ( 'NONE', 3,
 ( #76620, #14729, #83247, #90863 ),
 .UNSPECIFIED., .F., .F.,
 ( 4, 4 ),
 ( 6.938893903907228378E-18, 9.999999999999591193E-05 ),
 .UNSPECIFIED. ) ;
#17590 = CARTESIAN_POINT ( 'NONE',  ( -115.5228709571500616, -24.99156044556202616, 7.747789690856173195 ) ) ;
#17591 = CARTESIAN_POINT ( 'NONE',  ( -63.63170045961884114, -24.35071581493543036, 9.817618358456027039 ) ) ;
#17592 = CARTESIAN_POINT ( 'NONE',  ( 21.70358988458699301, 5.938112137899119070, 11.49999999999999645 ) ) ;
#17593 = ORIENTED_EDGE ( 'NONE', *, *, #29623, .T. ) ;
#17594 = LINE ( 'NONE', #2380, #35160 ) ;
#17595 = CARTESIAN_POINT ( 'NONE',  ( -20.77788740438921522, -7.151594987469691134, -1.500000000000002220 ) ) ;
#17596 = CARTESIAN_POINT ( 'NONE',  ( 32.65434780274890159, 3.991214330829748747, -3.988850826987774489 ) ) ;
#17597 = B_SPLINE_CURVE_WITH_KNOTS ( 'NONE', 3,
 ( #91981, #46311, #31074, #38186 ),
 .UNSPECIFIED., .F., .F.,
 ( 4, 4 ),
 ( 0.000000000000000000, 0.0001000000000000167422 ),
 .UNSPECIFIED. ) ;
#17598 = CARTESIAN_POINT ( 'NONE',  ( -34.62916631692677782, -24.51419770103156637, 9.386484678747176957 ) ) ;
#17599 = DIRECTION ( 'NONE',  ( -0.000000000000000000, 0.000000000000000000, -1.000000000000000000 ) ) ;
#17600 = ORIENTED_EDGE ( 'NONE', *, *, #84067, .F. ) ;
#17601 = EDGE_CURVE ( 'NONE', #70795, #22449, #97012, .T. ) ;
#17602 = CARTESIAN_POINT ( 'NONE',  ( -48.62833534578886940, -24.51419770103156637, 9.386484678747178734 ) ) ;
#17603 = DIRECTION ( 'NONE',  ( 0.000000000000000000, -0.9999999999976377785, -2.173523156925979128E-06 ) ) ;
#17604 = ORIENTED_EDGE ( 'NONE', *, *, #88779, .T. ) ;
#17605 = CARTESIAN_POINT ( 'NONE',  ( -15.16157141410761966, -13.82251119679066953, -1.500000000000002220 ) ) ;
#17606 = ORIENTED_EDGE ( 'NONE', *, *, #44984, .F. ) ;
#17607 = ORIENTED_EDGE ( 'NONE', *, *, #27550, .T. ) ;
#17608 = ORIENTED_EDGE ( 'NONE', *, *, #97413, .T. ) ;
#17609 = VERTEX_POINT ( 'NONE', #33939 ) ;
#17610 = CARTESIAN_POINT ( 'NONE',  ( -81.33773576950629547, -25.20044588977664546, 6.673200621925437837 ) ) ;
#17611 = CARTESIAN_POINT ( 'NONE',  ( 21.06059016766346659, 9.494407541345388779, -1.500000000000002220 ) ) ;
#17612 = CARTESIAN_POINT ( 'NONE',  ( 7.160000000000000142, -10.77121780415746599, 1.154761385154455366 ) ) ;
#17613 = CARTESIAN_POINT ( 'NONE',  ( -13.46841296510753061, 15.22696965993213070, -1.500000000000002220 ) ) ;
#17614 = ORIENTED_EDGE ( 'NONE', *, *, #60836, .F. ) ;
#17615 = CARTESIAN_POINT ( 'NONE',  ( 29.70906083364843653, 4.222256839740661682, 27.99786980188468277 ) ) ;
#17616 = AXIS2_PLACEMENT_3D ( 'NONE', #26689, #17568, #11457 ) ;
#17617 = CARTESIAN_POINT ( 'NONE',  ( -65.05438548721848235, -6.475225279485573360, 29.49402280011861777 ) ) ;
#17618 = CARTESIAN_POINT ( 'NONE',  ( -114.6228709571500701, -24.51387760970725083, 9.387446482453411178 ) ) ;
#17619 = CARTESIAN_POINT ( 'NONE',  ( 4.572862496014544753, -5.876774720514409189, 19.20224321281611068 ) ) ;
#17621 = ORIENTED_EDGE ( 'NONE', *, *, #1889, .T. ) ;
#17620 = CARTESIAN_POINT ( 'NONE',  ( -21.25412285906045895, 3.082840150875858054, 11.49999999999999645 ) ) ;
#17622 = CARTESIAN_POINT ( 'NONE',  ( -75.62719845405518981, -24.83618233451450763, 1.606449574219540599 ) ) ;
#17623 = CARTESIAN_POINT ( 'NONE',  ( -48.62287095715004881, -24.64898659630528144, 1.056161002820821038 ) ) ;
#17624 = ORIENTED_EDGE ( 'NONE', *, *, #42921, .F. ) ;
#17625 = CARTESIAN_POINT ( 'NONE',  ( 3.485566553294195291, 20.44204155273375889, -1.500000000000002220 ) ) ;
#17626 = ORIENTED_EDGE ( 'NONE', *, *, #82644, .F. ) ;
#17628 = ORIENTED_EDGE ( 'NONE', *, *, #100335, .T. ) ;
#17627 = CARTESIAN_POINT ( 'NONE',  ( 15.29947330337543754, 6.376774720514426953, -27.16854002387008649 ) ) ;
#17629 = CARTESIAN_POINT ( 'NONE',  ( -77.52287095715010423, -23.47593901973090524, -1.443836447538997092 ) ) ;
#17630 = CARTESIAN_POINT ( 'NONE',  ( -97.52287095715006160, -23.48786465467241769, 11.44779295918254114 ) ) ;
#17631 = ORIENTED_EDGE ( 'NONE', *, *, #88871, .T. ) ;
#17632 = VERTEX_POINT ( 'NONE', #95336 ) ;
#17633 = CARTESIAN_POINT ( 'NONE',  ( -6.728471858368818559, -5.876774720514409189, 19.14926908420045137 ) ) ;
#17634 = VECTOR ( 'NONE', #30300, 1000.000000000000000 ) ;
#17635 = CARTESIAN_POINT ( 'NONE',  ( -42.48684989586963923, -24.51419770103158413, 9.386484678747191168 ) ) ;
#17636 = CARTESIAN_POINT ( 'NONE',  ( -28.67183314889459922, -24.76456359476621216, 1.897690051802386924 ) ) ;
#17638 = ORIENTED_EDGE ( 'NONE', *, *, #23752, .T. ) ;
#17637 = CARTESIAN_POINT ( 'NONE',  ( -16.14483305390557888, 14.99321182834783528, 11.49999999999999645 ) ) ;
#17639 = CARTESIAN_POINT ( 'NONE',  ( -48.98794818101416837, -25.19490310348271578, 6.713761956252816354 ) ) ;
#17640 = CARTESIAN_POINT ( 'NONE',  ( 11.79716412695777272, 19.27136520130675024, -1.500000000000002220 ) ) ;
#17641 = CARTESIAN_POINT ( 'NONE',  ( 20.40321384664088811, -4.974606123342796060, -1.500000000000002220 ) ) ;
#17643 = ORIENTED_EDGE ( 'NONE', *, *, #23500, .F. ) ;
#17642 = CARTESIAN_POINT ( 'NONE',  ( -70.62287095715009855, -24.62226745350439927, 0.9660975649728139603 ) ) ;
#17644 = VERTEX_POINT ( 'NONE', #64918 ) ;
#17645 = DIRECTION ( 'NONE',  ( -0.4771587602595986910, -0.8788171126619707119, 0.000000000000000000 ) ) ;
#17646 = EDGE_CURVE ( 'NONE', #95924, #86751, #65419, .T. ) ;
#17647 = B_SPLINE_CURVE_WITH_KNOTS ( 'NONE', 3,
 ( #65076, #87376, #48834, #57951 ),
 .UNSPECIFIED., .F., .F.,
 ( 4, 4 ),
 ( 2.775557561562891043E-17, 9.999999999996124456E-05 ),
 .UNSPECIFIED. ) ;
#17648 = CIRCLE ( 'NONE', #97032, 2.399999999999999911 ) ;
#17649 = CARTESIAN_POINT ( 'NONE',  ( 31.63608488009067443, -0.6647747205144267646, 27.34773273846992225 ) ) ;
#17650 = VERTEX_POINT ( 'NONE', #94832 ) ;
#17651 = CARTESIAN_POINT ( 'NONE',  ( 17.87031378931267867, -11.31994873005049129, -1.500000000000002220 ) ) ;
#17652 = PLANE ( 'NONE',  #28720 ) ;
#17653 = CARTESIAN_POINT ( 'NONE',  ( -50.91781549829847364, -25.26041104471375576, 7.505037088851381100 ) ) ;
#17654 = CARTESIAN_POINT ( 'NONE',  ( -32.58953762381673869, -23.47596703998600276, 11.44779298504227505 ) ) ;
#17655 = FACE_OUTER_BOUND ( 'NONE', #93370, .T. ) ;
#17656 = CARTESIAN_POINT ( 'NONE',  ( 4.129723114849880083, -21.82631191821171512, -1.500000000000002220 ) ) ;
#17657 = CARTESIAN_POINT ( 'NONE',  ( -74.62287095715002749, -24.33927499327855060, 9.819080762295817166 ) ) ;
#17658 = ORIENTED_EDGE ( 'NONE', *, *, #89411, .T. ) ;
#17659 = CARTESIAN_POINT ( 'NONE',  ( -112.5228709571500616, -24.65952944569304961, 1.056160979905704123 ) ) ;
#17660 = CARTESIAN_POINT ( 'NONE',  ( -64.62287095715007013, -23.47596703998600631, 11.44779298504227683 ) ) ;
#17661 = CARTESIAN_POINT ( 'NONE',  ( 15.46825748771582631, 11.69065726450791409, 11.49999999999999645 ) ) ;
#17662 = CARTESIAN_POINT ( 'NONE',  ( -36.52731531746556470, -24.66019654487199730, 8.947790411086113949 ) ) ;
#17663 = B_SPLINE_CURVE_WITH_KNOTS ( 'NONE', 3,
 ( #64259, #56134, #23651, #70848, #25665, #93161, #47513, #15543, #827, #71351, #33272, #9435, #78438, #8441 ),
 .UNSPECIFIED., .F., .F.,
 ( 4, 2, 2, 2, 2, 2, 4 ),
 ( 0.000000000000000000, 0.0001813126694408965036, 0.0003626253388817930073, 0.0007252506777635843883, 0.001087876016645375823, 0.001269188686086291382, 0.001450501355527207374 ),
 .UNSPECIFIED. ) ;
#17664 = CARTESIAN_POINT ( 'NONE',  ( -39.58953762381673158, -24.64965694238574656, 8.947790433994203596 ) ) ;
#17665 = CARTESIAN_POINT ( 'NONE',  ( -2.678125609936932605, 19.29598960679622976, -1.500000000000002220 ) ) ;
#17666 = CARTESIAN_POINT ( 'NONE',  ( -21.42254595866439004, -0.3319015934494286557, -1.500000000000002220 ) ) ;
#17667 = CARTESIAN_POINT ( 'NONE',  ( -17.64648606763744354, 0.3587747205144061202, -23.04404205923973237 ) ) ;
#17668 = CARTESIAN_POINT ( 'NONE',  ( -60.58606081320825609, -24.63419186845290199, 9.035850630957110496 ) ) ;
#17669 = CARTESIAN_POINT ( 'NONE',  ( -51.56024018657757324, -23.73766607897669445, -1.055555164236457788 ) ) ;
#17670 = CARTESIAN_POINT ( 'NONE',  ( -77.58172370980747701, -24.65952944569304606, 1.056160979905701458 ) ) ;
#17671 = CARTESIAN_POINT ( 'NONE',  ( -22.77908990650604792, -0.06651829912971220227, -1.500000000000002220 ) ) ;
#17672 = DIRECTION ( 'NONE',  ( -2.804877950315662205E-17, 1.000000000000000000, 0.000000000000000000 ) ) ;
#17673 = CARTESIAN_POINT ( 'NONE',  ( -102.5094055064049172, -24.65952944569305316, 1.056160979905704123 ) ) ;
#17674 = CARTESIAN_POINT ( 'NONE',  ( 14.73162737928355170, 2.682774720514426559, -27.37940951657878941 ) ) ;
#17675 = CARTESIAN_POINT ( 'NONE',  ( -5.703961651189128901, -19.02375728206049743, 11.49999999999999645 ) ) ;
#17676 = CARTESIAN_POINT ( 'NONE',  ( -84.52287095715006160, -24.65952944569304606, 1.056160979905698794 ) ) ;
#17677 = AXIS2_PLACEMENT_3D ( 'NONE', #86099, #16577, #47553 ) ;
#17678 = AXIS2_PLACEMENT_3D ( 'NONE', #29560, #46290, #115 ) ;
#17679 = CARTESIAN_POINT ( 'NONE',  ( -89.06226385320384509, -25.27880950044345809, 5.947789066509452383 ) ) ;
#17680 = CARTESIAN_POINT ( 'NONE',  ( 7.749999999999998224, 25.69999999999999574, 2.100000000000000089 ) ) ;
#17681 = ORIENTED_EDGE ( 'NONE', *, *, #16702, .T. ) ;
#17682 = CARTESIAN_POINT ( 'NONE',  ( -84.52287095715006160, -29.50250786944525672, 11.44777988621623521 ) ) ;
#17683 = CARTESIAN_POINT ( 'NONE',  ( -29.49875734969026198, 0.3587747205144265483, 2.362022800118626531 ) ) ;
#17684 = CARTESIAN_POINT ( 'NONE',  ( -51.19185979282234200, -25.10935809339517633, 3.072504015734757843 ) ) ;
#17685 = CARTESIAN_POINT ( 'NONE',  ( -21.58526226860004371, 1.989002153404973328, 11.49999999999998934 ) ) ;
#17686 = CARTESIAN_POINT ( 'NONE',  ( -67.52287095715006160, -24.65952944569304961, 1.056160979905697239 ) ) ;
#17687 = CIRCLE ( 'NONE', #97063, 1.249999999999999112 ) ;
#17688 = CARTESIAN_POINT ( 'NONE',  ( -11.39837868854680814, -15.77482985264681403, -1.500000000000002220 ) ) ;
#17689 = PLANE ( 'NONE',  #92786 ) ;
#17690 = EDGE_CURVE ( 'NONE', #48981, #56729, #98232, .T. ) ;
#17691 = ORIENTED_EDGE ( 'NONE', *, *, #89017, .F. ) ;
#17692 = CIRCLE ( 'NONE', #19272, 129.7684398600581517 ) ;
#17693 = CARTESIAN_POINT ( 'NONE',  ( -12.60687543931603471, -16.05746371069360379, 11.49999999999999645 ) ) ;
#17694 = DIRECTION ( 'NONE',  ( 0.000000000000000000, -2.173523156925979552E-06, 0.9999999999976378895 ) ) ;
#17695 = LINE ( 'NONE', #92808, #18867 ) ;
#17696 = B_SPLINE_CURVE_WITH_KNOTS ( 'NONE', 3,
 ( #32512, #72587, #78661, #5555, #11665, #4069 ),
 .UNSPECIFIED., .F., .F.,
 ( 4, 2, 4 ),
 ( 0.000000000000000000, 0.001380764517854764532, 0.002761529035709529064 ),
 .UNSPECIFIED. ) ;
#17697 = EDGE_LOOP ( 'NONE', ( #16092, #48695, #33482, #99286, #73400 ) ) ;
#17698 = CARTESIAN_POINT ( 'NONE',  ( -41.24483612983362946, -25.23676607602647337, 3.617455962827678562 ) ) ;
#17699 = CARTESIAN_POINT ( 'NONE',  ( 33.63243172119919677, 3.340070231344507423, -11.49682753434938043 ) ) ;
#17700 = CARTESIAN_POINT ( 'NONE',  ( -39.10567952407142656, -25.27985361285174903, 4.652296651879083811 ) ) ;
#17701 = EDGE_CURVE ( 'NONE', #47794, #43355, #45096, .T. ) ;
#17702 = AXIS2_PLACEMENT_3D ( 'NONE', #83097, #21201, #13087 ) ;
#17703 = LINE ( 'NONE', #18688, #6860 ) ;
#17704 = CARTESIAN_POINT ( 'NONE',  ( -1.041963229364719634, -6.376774720514417183, 20.24089781925592746 ) ) ;
#17705 = PLANE ( 'NONE',  #14344 ) ;
#17707 = ORIENTED_EDGE ( 'NONE', *, *, #15686, .F. ) ;
#17706 = ADVANCED_FACE ( 'NONE', ( #2496 ), #9099, .T. ) ;
#17708 = FACE_OUTER_BOUND ( 'NONE', #8706, .T. ) ;
#17709 = EDGE_CURVE ( 'NONE', #84649, #27354, #3944, .T. ) ;
#17710 = CARTESIAN_POINT ( 'NONE',  ( -21.48638390452810043, -8.140844714011898020, 11.49999999999999645 ) ) ;
#17711 = CARTESIAN_POINT ( 'NONE',  ( 22.67573665902413182, 1.879276792517311501, 11.49999999999998934 ) ) ;
#17712 = VERTEX_POINT ( 'NONE', #48684 ) ;
#17713 = CARTESIAN_POINT ( 'NONE',  ( -110.6256069007815626, -24.73531770709095312, 8.716586749053508498 ) ) ;
#17714 = EDGE_CURVE ( 'NONE', #80254, #56196, #36597, .T. ) ;
#17715 = CARTESIAN_POINT ( 'NONE',  ( -75.62287095715009855, -24.63345952396255356, 9.038047939301504741 ) ) ;
#17716 = CARTESIAN_POINT ( 'NONE',  ( 10.45000000000000462, 1.999999999999998668, 18.24068255301867936 ) ) ;
#17717 = EDGE_CURVE ( 'NONE', #50837, #32014, #33434, .T. ) ;
#17718 = LINE ( 'NONE', #63920, #85409 ) ;
#17719 = CARTESIAN_POINT ( 'NONE',  ( -18.33957545910867282, 11.93505917737106259, -1.500000000000002220 ) ) ;
#17720 = CARTESIAN_POINT ( 'NONE',  ( -74.52287095715007581, -23.47593901973090169, -1.443836447538996870 ) ) ;
#17721 = VECTOR ( 'NONE', #46264, 1000.000000000000000 ) ;
#17722 = DIRECTION ( 'NONE',  ( 0.000000000000000000, 0.3081562241202474017, 0.9513357669802769978 ) ) ;
#17723 = DIRECTION ( 'NONE',  ( 0.000000000000000000, -1.000000000000000000, 0.000000000000000000 ) ) ;
#17724 = FACE_OUTER_BOUND ( 'NONE', #65092, .T. ) ;
#17725 = ORIENTED_EDGE ( 'NONE', *, *, #80833, .F. ) ;
#17726 = CARTESIAN_POINT ( 'NONE',  ( 19.51578053514377586, 5.923290232019536639, -1.500000000000002220 ) ) ;
#17727 = ORIENTED_EDGE ( 'NONE', *, *, #87572, .T. ) ;
#17728 = ORIENTED_EDGE ( 'NONE', *, *, #61187, .F. ) ;
#17729 = EDGE_CURVE ( 'NONE', #12603, #26207, #56797, .T. ) ;
#17730 = CARTESIAN_POINT ( 'NONE',  ( 17.37538969058663696, -15.08583811485692117, 11.49999999999998934 ) ) ;
#17731 = CARTESIAN_POINT ( 'NONE',  ( 0.5999240985075944277, 1.411520799013914917, -8.999999999999994671 ) ) ;
#17732 = ORIENTED_EDGE ( 'NONE', *, *, #73825, .T. ) ;
#17733 = CARTESIAN_POINT ( 'NONE',  ( -101.5228709571500758, -24.65952944569304606, 1.056160979905702346 ) ) ;
#17734 = DIRECTION ( 'NONE',  ( 0.000000000000000000, 0.000000000000000000, 1.000000000000000000 ) ) ;
#17735 = CARTESIAN_POINT ( 'NONE',  ( -95.55372101787112626, -24.15503026093913874, -0.2815557561904519224 ) ) ;
#17736 = DIRECTION ( 'NONE',  ( 0.000000000000000000, 0.000000000000000000, 1.000000000000000000 ) ) ;
#17738 = VERTEX_POINT ( 'NONE', #80606 ) ;
#17737 = CARTESIAN_POINT ( 'NONE',  ( 3.515848477382193416, 21.04717058667041130, 11.49999999999999645 ) ) ;
#17739 = EDGE_LOOP ( 'NONE', ( #65063, #64202, #3667, #73022 ) ) ;
#17740 = CARTESIAN_POINT ( 'NONE',  ( -11.95080204275630464, 18.75100984808165094, -1.500000000000002220 ) ) ;
#17741 = CARTESIAN_POINT ( 'NONE',  ( 19.39950376024442846, -7.079068461131618584, 11.49999999999998934 ) ) ;
#17742 = VERTEX_POINT ( 'NONE', #3003 ) ;
#17743 = CARTESIAN_POINT ( 'NONE',  ( 22.02124265030973760, -6.143225279485574397, 13.95402280011862395 ) ) ;
#17744 = CARTESIAN_POINT ( 'NONE',  ( -95.54323508187783887, -24.92592662359561473, 8.075495903017998245 ) ) ;
#17745 = ORIENTED_EDGE ( 'NONE', *, *, #43289, .F. ) ;
#17746 = PLANE ( 'NONE',  #80223 ) ;
#17747 = VECTOR ( 'NONE', #92343, 1000.000000000000000 ) ;
#17748 = ORIENTED_EDGE ( 'NONE', *, *, #18035, .T. ) ;
#17749 = CARTESIAN_POINT ( 'NONE',  ( -49.55620429048340014, -23.48783264082477729, -1.443836473390071484 ) ) ;
#17750 = FACE_OUTER_BOUND ( 'NONE', #62933, .T. ) ;
#17751 = CARTESIAN_POINT ( 'NONE',  ( -10.06633388967972209, 18.29571535785830960, -1.500000000000002220 ) ) ;
#17753 = EDGE_CURVE ( 'NONE', #58220, #37557, #95832, .T. ) ;
#17752 = CARTESIAN_POINT ( 'NONE',  ( -9.708950231915746798, -19.59419465507263070, 11.49999999999999645 ) ) ;
#17754 = CARTESIAN_POINT ( 'NONE',  ( -107.6228709571501412, -24.35013146730204525, 9.818937971375106599 ) ) ;
#17755 = DIRECTION ( 'NONE',  ( 3.469446951953615767E-15, -1.000000000000000000, 0.000000000000000000 ) ) ;
#17756 = CARTESIAN_POINT ( 'NONE',  ( -9.984083066403742990, 20.14924292131567185, 11.49999999999998934 ) ) ;
#17757 = VECTOR ( 'NONE', #58565, 1000.000000000000114 ) ;
#17758 = CARTESIAN_POINT ( 'NONE',  ( 13.94627346685978075, -15.57361473980792255, -1.500000000000002220 ) ) ;
#17759 = CARTESIAN_POINT ( 'NONE',  ( -89.40841769935771310, -25.35030500980171553, 4.902495265462817997 ) ) ;
#17760 = EDGE_CURVE ( 'NONE', #19353, #11284, #5818, .T. ) ;
#17761 = CARTESIAN_POINT ( 'NONE',  ( -72.52287095715009002, -24.35013146730203815, 9.818937971375110152 ) ) ;
#17762 = CARTESIAN_POINT ( 'NONE',  ( 4.638796026491669444, -5.876774720514423400, 21.40644651702305268 ) ) ;
#17763 = VERTEX_POINT ( 'NONE', #19692 ) ;
#17764 = CIRCLE ( 'NONE', #87431, 80.18232118519037499 ) ;
#17765 = ORIENTED_EDGE ( 'NONE', *, *, #89088, .T. ) ;
#17766 = AXIS2_PLACEMENT_3D ( 'NONE', #29055, #98559, #59028 ) ;
#17767 = EDGE_LOOP ( 'NONE', ( #99402, #4135, #8734, #20321 ) ) ;
#17768 = CARTESIAN_POINT ( 'NONE',  ( -99.29890324015507019, -25.12215488674418751, 6.243173985830122064 ) ) ;
#17769 = ORIENTED_EDGE ( 'NONE', *, *, #40629, .T. ) ;
#17770 = VECTOR ( 'NONE', #15497, 1000.000000000000114 ) ;
#17771 = CARTESIAN_POINT ( 'NONE',  ( 6.029407872858970840, -20.54391778677962677, -1.500000000000002220 ) ) ;
#17773 = EDGE_CURVE ( 'NONE', #25724, #12032, #82601, .T. ) ;
#17772 = CARTESIAN_POINT ( 'NONE',  ( -11.68221627493902126, 19.09626523228051553, 11.49999999999999645 ) ) ;
#17774 = EDGE_LOOP ( 'NONE', ( #19251, #62653, #78916, #77882, #84146, #94398 ) ) ;
#17775 = CARTESIAN_POINT ( 'NONE',  ( -26.33488822642538452, -24.88201932036028552, 6.524121876823151034 ) ) ;
#17776 = CARTESIAN_POINT ( 'NONE',  ( 20.75205275252385206, -3.532026382766447536, -1.500000000000002220 ) ) ;
#17777 = CARTESIAN_POINT ( 'NONE',  ( -30.54990185496676247, -24.48551988174978078, 9.440108529385042857 ) ) ;
#17778 = CARTESIAN_POINT ( 'NONE',  ( -18.79874323561663729, 6.599581278811135654, -1.500000000000002220 ) ) ;
#17779 = CARTESIAN_POINT ( 'NONE',  ( -27.86046284349297864, -5.965225279485572685, -8.091963836038754465 ) ) ;
#17780 = CARTESIAN_POINT ( 'NONE',  ( -101.5910278892822447, -24.15543982623907482, -0.2315651400026588480 ) ) ;
#17781 = CARTESIAN_POINT ( 'NONE',  ( -7.807709442696729063, 20.60712426125841645, -1.500000000000002220 ) ) ;
#17782 = VERTEX_POINT ( 'NONE', #50170 ) ;
#17783 = CARTESIAN_POINT ( 'NONE',  ( 28.20688450243589784, -4.772774720514425972, -7.073367244511575613 ) ) ;
#17784 = ADVANCED_FACE ( 'NONE', ( #65913 ), #66411, .F. ) ;
#17785 = CARTESIAN_POINT ( 'NONE',  ( -96.62287095715005592, -23.48786465467241413, 11.44779295918254114 ) ) ;
#17786 = CARTESIAN_POINT ( 'NONE',  ( -4.186882374726557110, 20.40937146592452223, 11.49999999999999645 ) ) ;
#17787 = CARTESIAN_POINT ( 'NONE',  ( -25.50529870902546037, -24.92367794922509816, 4.936952632524853612 ) ) ;
#17788 = CARTESIAN_POINT ( 'NONE',  ( 0.000000000000000000, -16.94322527948557422, 0.000000000000000000 ) ) ;
#17789 = CARTESIAN_POINT ( 'NONE',  ( -129.6228709571500417, -29.50247984919015209, -1.443849546365044922 ) ) ;
#17790 = CARTESIAN_POINT ( 'NONE',  ( -6.196366259867160942, 20.41550611124569059, -1.500000000000002220 ) ) ;
#17791 = LINE ( 'NONE', #24889, #69343 ) ;
#17792 = CARTESIAN_POINT ( 'NONE',  ( -66.62287095715005592, -23.47596703998600276, 11.44779298504227683 ) ) ;
#17793 = DIRECTION ( 'NONE',  ( -0.000000000000000000, 2.173523156925979552E-06, -0.9999999999976378895 ) ) ;
#17794 = PLANE ( 'NONE',  #588 ) ;
#17795 = CC_DESIGN_DATE_AND_TIME_ASSIGNMENT ( #3717, #43770, ( #70488 ) ) ;
#17796 = CARTESIAN_POINT ( 'NONE',  ( -8.633696204196466439, -20.85254729778420923, -1.500000000000002220 ) ) ;
#17797 = B_SPLINE_CURVE_WITH_KNOTS ( 'NONE', 3,
 ( #99797, #55670, #1378, #7464 ),
 .UNSPECIFIED., .F., .F.,
 ( 4, 4 ),
 ( 2.775557561562891043E-17, 9.999999999998898659E-05 ),
 .UNSPECIFIED. ) ;
#17798 = CARTESIAN_POINT ( 'NONE',  ( -81.62287095715005592, -24.65952944569304606, 1.056160979905699460 ) ) ;
#17799 = ORIENTED_EDGE ( 'NONE', *, *, #88894, .T. ) ;
#17800 = FACE_OUTER_BOUND ( 'NONE', #74578, .T. ) ;
#17801 = CARTESIAN_POINT ( 'NONE',  ( -31.57095388386905199, -23.48786465467240347, 11.44779295918255535 ) ) ;
#17802 = CARTESIAN_POINT ( 'NONE',  ( 2.289404864003111051, -19.52285375609543294, 11.49999999999999645 ) ) ;
#17803 = FACE_OUTER_BOUND ( 'NONE', #45602, .T. ) ;
#17805 = B_SPLINE_CURVE_WITH_KNOTS ( 'NONE', 3,
 ( #19325, #44677, #29432, #45673 ),
 .UNSPECIFIED., .F., .F.,
 ( 4, 4 ),
 ( 0.8694025111800981476, 0.8704032582208635072 ),
 .UNSPECIFIED. ) ;
#17804 = DIRECTION ( 'NONE',  ( 0.1489078231574191002, -6.845827386180410961E-16, -0.9888510809027407644 ) ) ;
#17806 = ORIENTED_EDGE ( 'NONE', *, *, #89298, .T. ) ;
#17807 = CARTESIAN_POINT ( 'NONE',  ( -94.52287095715011844, -23.48783264082477373, -1.443836473390087027 ) ) ;
#17808 = CARTESIAN_POINT ( 'NONE',  ( -55.62287095715003460, -24.82558206586145033, 1.605769216559449930 ) ) ;
#17809 = DIRECTION ( 'NONE',  ( -3.773278334453079618E-23, 0.9999999999976377785, 2.173523156925979975E-06 ) ) ;
#17810 = DIRECTION ( 'NONE',  ( 0.000000000000000000, 1.734723475976807094E-15, -1.000000000000000000 ) ) ;
#17811 = CARTESIAN_POINT ( 'NONE',  ( -32.50560602629348494, -24.87219037988797865, 1.747789950295646877 ) ) ;
#17812 = LINE ( 'NONE', #34039, #82085 ) ;
#17813 = CARTESIAN_POINT ( 'NONE',  ( 14.33573519231038063, 13.56928687979844561, 11.49999999999998934 ) ) ;
#17814 = EDGE_LOOP ( 'NONE', ( #74627, #78113, #98297, #87365 ) ) ;
#17815 = CARTESIAN_POINT ( 'NONE',  ( 20.15506735835773000, -1.303320585059813741, 11.49999999999999645 ) ) ;
#17816 = CARTESIAN_POINT ( 'NONE',  ( 11.40529837385589218, 6.376774720514345240, -28.07356074678033409 ) ) ;
#17817 = CIRCLE ( 'NONE', #89162, 130.7884398600581335 ) ;
#17818 = ORIENTED_EDGE ( 'NONE', *, *, #6931, .F. ) ;
#17819 = CARTESIAN_POINT ( 'NONE',  ( -67.52287095715006160, -23.48786465467241769, 11.44779295918254647 ) ) ;
#17820 = CARTESIAN_POINT ( 'NONE',  ( -69.34990230688175927, -25.25756224058122967, 6.083752085800076870 ) ) ;
#17821 = CARTESIAN_POINT ( 'NONE',  ( -88.88918693012689687, -25.27880950044345454, 5.947789066509454159 ) ) ;
#17822 = CARTESIAN_POINT ( 'NONE',  ( -38.52287095715006870, -24.64898659630367206, 1.056161002820819261 ) ) ;
#17823 = VECTOR ( 'NONE', #83364, 1000.000000000000114 ) ;
#17824 = CARTESIAN_POINT ( 'NONE',  ( -103.6228709571501128, -23.95044443724992789, 10.65354141964649592 ) ) ;
#17825 = DIRECTION ( 'NONE',  ( -0.000000000000000000, 1.000000000000000000, -0.000000000000000000 ) ) ;
#17827 = EDGE_CURVE ( 'NONE', #79519, #5376, #67391, .T. ) ;
#17826 = CARTESIAN_POINT ( 'NONE',  ( 7.431233518514567926, -18.57414813805618081, -1.500000000000002220 ) ) ;
#17828 = CARTESIAN_POINT ( 'NONE',  ( -99.62559895716422886, -25.27532914723576241, 3.076829306349715853 ) ) ;
#17829 = VERTEX_POINT ( 'NONE', #88731 ) ;
#17830 = CIRCLE ( 'NONE', #38820, 20.00000000000000000 ) ;
#17831 = AXIS2_PLACEMENT_3D ( 'NONE', #54421, #90980, #83863 ) ;
#17832 = CARTESIAN_POINT ( 'NONE',  ( -79.49884268526720632, -24.66019654487199375, 8.947790411086119278 ) ) ;
#17833 = ADVANCED_FACE ( 'NONE', ( #57786 ), #28315, .T. ) ;
#17834 = DIRECTION ( 'NONE',  ( 0.000000000000000000, 0.000000000000000000, -1.000000000000000000 ) ) ;
#17835 = CARTESIAN_POINT ( 'NONE',  ( 13.91401389203221406, 6.376774720514426953, 28.26920385068457264 ) ) ;
#17836 = VECTOR ( 'NONE', #28314, 1000.000000000000000 ) ;
#17837 = EDGE_CURVE ( 'NONE', #93974, #1915, #70226, .T. ) ;
#17838 = CARTESIAN_POINT ( 'NONE',  ( -119.4336609825042927, -25.40057329150818077, 4.607792141311822576 ) ) ;
#17839 = CARTESIAN_POINT ( 'NONE',  ( -103.5228709571500900, -23.96127896941633395, -0.6493128931038035789 ) ) ;
#17840 = VECTOR ( 'NONE', #47866, 999.9999999999998863 ) ;
#17841 = CARTESIAN_POINT ( 'NONE',  ( 14.74567117936177851, 4.687674228468470261, -27.80582190761142414 ) ) ;
#17842 = CARTESIAN_POINT ( 'NONE',  ( -75.62287095715004170, -29.50249982740957577, 7.747779886224967605 ) ) ;
#17843 = VERTEX_POINT ( 'NONE', #21191 ) ;
#17844 = CARTESIAN_POINT ( 'NONE',  ( 13.49383759531269433, -15.17088004136028090, -1.500000000000002220 ) ) ;
#17845 = VERTEX_POINT ( 'NONE', #96829 ) ;
#17846 = EDGE_CURVE ( 'NONE', #81283, #67869, #10745, .T. ) ;
#17847 = LINE ( 'NONE', #112, #14491 ) ;
#17848 = CARTESIAN_POINT ( 'NONE',  ( -127.5210440253001849, -24.51419770103158768, 9.386484678747160970 ) ) ;
#17849 = CARTESIAN_POINT ( 'NONE',  ( -59.54824621938957563, -24.15620529776628089, 10.23563542870661180 ) ) ;
#17850 = DIRECTION ( 'NONE',  ( -0.9762960071199348056, -0.2164396139380966033, -0.000000000000000000 ) ) ;
#17851 = B_SPLINE_CURVE_WITH_KNOTS ( 'NONE', 3,
 ( #83328, #13808, #81344, #11825 ),
 .UNSPECIFIED., .F., .F.,
 ( 4, 4 ),
 ( 2.775557561562891351E-17, 0.0001000000000000167286 ),
 .UNSPECIFIED. ) ;
#17852 = CARTESIAN_POINT ( 'NONE',  ( -86.55620429048337883, -23.47593901973091235, -1.443836447539002865 ) ) ;
#17853 = CARTESIAN_POINT ( 'NONE',  ( -9.620199658202244208, 18.81650055922726494, 11.49999999999999645 ) ) ;
#17854 = CARTESIAN_POINT ( 'NONE',  ( 22.09269804725545683, -1.632937629565654580, -1.500000000000002220 ) ) ;
#17855 = CARTESIAN_POINT ( 'NONE',  ( -18.11865614447288664, 9.752654332028551920, 11.49999999999998934 ) ) ;
#17856 = ORIENTED_EDGE ( 'NONE', *, *, #93861, .F. ) ;
#17857 = DIRECTION ( 'NONE',  ( 0.000000000000000000, 1.000000000000000000, 0.000000000000000000 ) ) ;
#17858 = VERTEX_POINT ( 'NONE', #90220 ) ;
#17859 = CARTESIAN_POINT ( 'NONE',  ( -54.50229491303872464, -24.15543982623906416, -0.2315651400026691176 ) ) ;
#17860 = DIRECTION ( 'NONE',  ( -0.000000000000000000, 1.000000000000000000, -0.000000000000000000 ) ) ;
#17861 = VERTEX_POINT ( 'NONE', #35442 ) ;
#17862 = ORIENTED_EDGE ( 'NONE', *, *, #49822, .T. ) ;
#17863 = ORIENTED_EDGE ( 'NONE', *, *, #82532, .T. ) ;
#17864 = CARTESIAN_POINT ( 'NONE',  ( -81.62287095715008434, -24.33927499327855060, 9.819080762295817166 ) ) ;
#17865 = CARTESIAN_POINT ( 'NONE',  ( 7.116579217368891541, -5.876774720514415407, 20.51774267661129869 ) ) ;
#17866 = CARTESIAN_POINT ( 'NONE',  ( 5.557675543255346184, -5.876774720514415407, 20.10561748372801461 ) ) ;
#17867 = CARTESIAN_POINT ( 'NONE',  ( -13.38394104848841693, -15.81244124602197765, -1.500000000000002220 ) ) ;
#17868 = CARTESIAN_POINT ( 'NONE',  ( -6.994818212361641585, 20.52682044044541598, 11.49999999999999645 ) ) ;
#17869 = ORIENTED_EDGE ( 'NONE', *, *, #11527, .T. ) ;
#17870 = DIRECTION ( 'NONE',  ( 1.000000000000000000, 0.000000000000000000, -2.168404344971008868E-16 ) ) ;
#17871 = LINE ( 'NONE', #86873, #30228 ) ;
#17872 = CARTESIAN_POINT ( 'NONE',  ( 15.70178742502441693, -15.98865493379879332, 11.49999999999998934 ) ) ;
#17873 = CARTESIAN_POINT ( 'NONE',  ( -79.35008398046767297, -25.27874868537385922, 6.078937478087434343 ) ) ;
#17874 = CARTESIAN_POINT ( 'NONE',  ( -58.52287095715006160, -23.47596703998600631, 11.44779298504228926 ) ) ;
#17876 = EDGE_LOOP ( 'NONE', ( #33811, #5854, #62803, #9255 ) ) ;
#17875 = EDGE_CURVE ( 'NONE', #29613, #60506, #41298, .T. ) ;
#17877 = CARTESIAN_POINT ( 'NONE',  ( -45.62287095715004881, -24.99132157543083821, 2.256160258750667502 ) ) ;
#17878 = CARTESIAN_POINT ( 'NONE',  ( -35.63736055960579563, -24.63419186844611986, 9.035850630976925757 ) ) ;
#17879 = VERTEX_POINT ( 'NONE', #44546 ) ;
#17880 = ORIENTED_EDGE ( 'NONE', *, *, #36432, .T. ) ;
#17881 = CIRCLE ( 'NONE', #79442, 252.4458649670781085 ) ;
#17882 = EDGE_CURVE ( 'NONE', #60254, #26341, #19199, .T. ) ;
#17883 = CARTESIAN_POINT ( 'NONE',  ( -39.52287095715006870, -24.66019654487198665, 8.947790411086131712 ) ) ;
#17884 = VERTEX_POINT ( 'NONE', #74002 ) ;
#17885 = EDGE_CURVE ( 'NONE', #72803, #53441, #58285, .T. ) ;
#17886 = PLANE ( 'NONE',  #74655 ) ;
#17887 = CARTESIAN_POINT ( 'NONE',  ( -1.624102159174229731, 21.17438964843747584, -1.500000000000002220 ) ) ;
#17888 = ORIENTED_EDGE ( 'NONE', *, *, #90952, .F. ) ;
#17889 = CARTESIAN_POINT ( 'NONE',  ( -88.51806581271243601, -23.73766607897670156, -1.055555164236456678 ) ) ;
#17890 = CARTESIAN_POINT ( 'NONE',  ( -11.04117723084791614, -18.81814233335528286, 11.49999999999998934 ) ) ;
#17891 = CARTESIAN_POINT ( 'NONE',  ( -103.6235449969178859, -24.66019654487200086, 8.947790411086119278 ) ) ;
#17892 = B_SPLINE_CURVE_WITH_KNOTS ( 'NONE', 3,
 ( #59536, #98068, #12838, #66674, #5238, #60041, #36688, #50929, #51922, #90970, #5733, #82852, #51424, #28576, #58540, #97584, #13335, #44315 ),
 .UNSPECIFIED., .F., .F.,
 ( 4, 2, 2, 2, 2, 2, 2, 2, 4 ),
 ( 0.000000000000000000, 0.0002166463785664153835, 0.0004332927571328307670, 0.0008665855142656615339, 0.001083231892832076104, 0.001299878271398490675, 0.001733171028531327621, 0.002599756542797003901, 0.003466342057062679963 ),
 .UNSPECIFIED. ) ;
#17893 = DIRECTION ( 'NONE',  ( 0.000000000000000000, 2.173523156925980399E-06, -0.9999999999976378895 ) ) ;
#17894 = CARTESIAN_POINT ( 'NONE',  ( -50.52287095715006160, -24.99156044556120193, 7.747789690856173195 ) ) ;
#17895 = CARTESIAN_POINT ( 'NONE',  ( -15.13543854793762300, 15.80457324685279374, -1.500000000000002220 ) ) ;
#17896 = DIRECTION ( 'NONE',  ( 4.335561085774420994E-16, 0.000000000000000000, -1.000000000000000000 ) ) ;
#17897 = VERTEX_POINT ( 'NONE', #73500 ) ;
#17898 = CARTESIAN_POINT ( 'NONE',  ( -65.62287095715007013, -24.15431212366392089, -0.2830839119429129358 ) ) ;
#17899 = CARTESIAN_POINT ( 'NONE',  ( -85.62651978001045450, -24.83644354573578994, 8.397322867130101898 ) ) ;
#17900 = ORIENTED_EDGE ( 'NONE', *, *, #15294, .T. ) ;
#17901 = VERTEX_POINT ( 'NONE', #13578 ) ;
#17902 = VECTOR ( 'NONE', #66353, 1000.000000000000114 ) ;
#17903 = ORIENTED_EDGE ( 'NONE', *, *, #72460, .F. ) ;
#17904 = CARTESIAN_POINT ( 'NONE',  ( -28.88940304597720399, -25.00679290501443219, 2.971342454648660425 ) ) ;
#17905 = CIRCLE ( 'NONE', #35729, 1.150000000000003464 ) ;
#17906 = FACE_OUTER_BOUND ( 'NONE', #70884, .T. ) ;
#17907 = CARTESIAN_POINT ( 'NONE',  ( -20.82729772986975547, -4.079710536234080642, -1.500000000000002220 ) ) ;
#17908 = LINE ( 'NONE', #72204, #25592 ) ;
#17909 = PLANE ( 'NONE',  #57637 ) ;
#17910 = EDGE_CURVE ( 'NONE', #82409, #17980, #12590, .T. ) ;
#17911 = CARTESIAN_POINT ( 'NONE',  ( 13.91401389203221406, 6.376774720514426953, 158.0376437107427137 ) ) ;
#17912 = CARTESIAN_POINT ( 'NONE',  ( -68.62287095715005592, -29.50248528299804818, 1.056150453629036701 ) ) ;
#17913 = EDGE_CURVE ( 'NONE', #24333, #81001, #36926, .T. ) ;
#17914 = CIRCLE ( 'NONE', #82722, 12.23252173913042995 ) ;
#17915 = CARTESIAN_POINT ( 'NONE',  ( -8.724563080612403709, -17.33930400145671413, 11.49999999999998934 ) ) ;
#17916 = DIRECTION ( 'NONE',  ( 0.000000000000000000, -1.000000000000000000, 0.000000000000000000 ) ) ;
#17917 = VERTEX_POINT ( 'NONE', #13077 ) ;
#17918 = CARTESIAN_POINT ( 'NONE',  ( 9.662506626059768067, -16.94115208737379774, 11.49999999999999645 ) ) ;
#17919 = CARTESIAN_POINT ( 'NONE',  ( -5.314757719055156038, -5.876774720514410077, 19.55912026249540858 ) ) ;
#17920 = DIRECTION ( 'NONE',  ( -3.773278334453080206E-23, 0.9999999999976377785, 2.173523156925979975E-06 ) ) ;
#17921 = ORIENTED_EDGE ( 'NONE', *, *, #28818, .T. ) ;
#17922 = CARTESIAN_POINT ( 'NONE',  ( 4.527536911777373163, -5.876774720514421624, 21.53954785142818196 ) ) ;
#17923 = EDGE_CURVE ( 'NONE', #82726, #90388, #47226, .T. ) ;
#17924 = CARTESIAN_POINT ( 'NONE',  ( 0.1645010273463760886, -0.3687607960183749145, 1.417169167140625907 ) ) ;
#17925 = EDGE_CURVE ( 'NONE', #43385, #39577, #4982, .T. ) ;
#17926 = CARTESIAN_POINT ( 'NONE',  ( -88.52287095715006160, -23.47593901973090524, -1.443836447538996426 ) ) ;
#17927 = CARTESIAN_POINT ( 'NONE',  ( -81.43785252974821276, -25.24813914738149734, 7.210847438489675021 ) ) ;
#17928 = CARTESIAN_POINT ( 'NONE',  ( 16.09843989366402539, -11.26760994518913428, -1.500000000000002220 ) ) ;
#17929 = VERTEX_POINT ( 'NONE', #98314 ) ;
#17930 = DIRECTION ( 'NONE',  ( -3.773278334453079618E-23, 0.9999999999976377785, 2.173523156925979975E-06 ) ) ;
#17931 = CARTESIAN_POINT ( 'NONE',  ( 21.75596283627254479, -7.788036635067100200, -1.500000000000002220 ) ) ;
#17932 = PERSON_AND_ORGANIZATION ( #70597, #27821 ) ;
#17933 = CARTESIAN_POINT ( 'NONE',  ( 3.787259615384621192, -5.876774720514425177, 21.48076923076922640 ) ) ;
#17934 = DIRECTION ( 'NONE',  ( -1.000000000000000000, -0.000000000000000000, -0.000000000000000000 ) ) ;
#17935 = CARTESIAN_POINT ( 'NONE',  ( -115.6228709571500843, -24.52323809116982645, 9.355190652339407720 ) ) ;
#17936 = CARTESIAN_POINT ( 'NONE',  ( -29.52287095715007226, -23.86488628232234888, 10.65372853282540433 ) ) ;
#17937 = CARTESIAN_POINT ( 'NONE',  ( -81.90384961113220186, -25.20144873054373136, 6.835696071488102099 ) ) ;
#17938 = CARTESIAN_POINT ( 'NONE',  ( 6.179707021866671646, -5.876774720514425177, 21.45334750074374242 ) ) ;
#17939 = CARTESIAN_POINT ( 'NONE',  ( -73.52287095715011844, -24.51387760970724372, 9.387446482453396968 ) ) ;
#17940 = CARTESIAN_POINT ( 'NONE',  ( -114.5946007866755281, -23.48786465467241769, 11.44779295918253759 ) ) ;
#17942 = EDGE_CURVE ( 'NONE', #17028, #7900, #28819, .T. ) ;
#17941 = CARTESIAN_POINT ( 'NONE',  ( -18.10700488460823721, -8.296952762055457953, -1.500000000000002220 ) ) ;
#17943 = PLANE ( 'NONE',  #80854 ) ;
#17944 = CARTESIAN_POINT ( 'NONE',  ( 19.87125486832220744, 0.9792442318621276121, -1.500000000000002220 ) ) ;
#17945 = ORIENTED_EDGE ( 'NONE', *, *, #11965, .T. ) ;
#17946 = CYLINDRICAL_SURFACE ( 'NONE', #21575, 1.149999999999998135 ) ;
#17947 = CARTESIAN_POINT ( 'NONE',  ( -55.52287095715005449, -24.99132157543083821, 2.256160258750667502 ) ) ;
#17948 = CARTESIAN_POINT ( 'NONE',  ( -35.62287095715005592, -24.99156045073392463, 7.747789690856161648 ) ) ;
#17949 = CARTESIAN_POINT ( 'NONE',  ( -2.100290975465340271, -20.70549805216813510, 11.49999999999999645 ) ) ;
#17950 = CARTESIAN_POINT ( 'NONE',  ( -7.617563585130437076, -5.876774720514411854, 19.95084900476494383 ) ) ;
#17951 = AXIS2_PLACEMENT_3D ( 'NONE', #41228, #47838, #80282 ) ;
#17952 = EDGE_CURVE ( 'NONE', #55213, #4924, #15762, .T. ) ;
#17953 = CARTESIAN_POINT ( 'NONE',  ( -126.6228709571500559, -24.64898659630529565, 1.056161002820834804 ) ) ;
#17954 = CARTESIAN_POINT ( 'NONE',  ( 21.74077840044056842, -6.890983112422549794, 11.49999999999999645 ) ) ;
#17955 = ORIENTED_EDGE ( 'NONE', *, *, #37866, .F. ) ;
#17956 = CARTESIAN_POINT ( 'NONE',  ( -76.52287095715007581, -29.50250243563736774, 8.947779886222141599 ) ) ;
#17957 = EDGE_CURVE ( 'NONE', #79287, #56311, #36441, .T. ) ;
#17958 = CARTESIAN_POINT ( 'NONE',  ( -41.62287095715006302, -29.50248528299804818, 1.056150453629031594 ) ) ;
#17959 = ORIENTED_EDGE ( 'NONE', *, *, #25901, .T. ) ;
#17960 = CARTESIAN_POINT ( 'NONE',  ( 8.473373031455752269, -18.34320851062214430, -1.500000000000002220 ) ) ;
#17961 = CARTESIAN_POINT ( 'NONE',  ( 6.955725288069978696, -6.376774720514426065, 21.70430095680336890 ) ) ;
#17962 = EDGE_CURVE ( 'NONE', #46989, #72780, #2487, .T. ) ;
#17963 = DIRECTION ( 'NONE',  ( 0.000000000000000000, -1.000000000000000000, 0.000000000000000000 ) ) ;
#17964 = EDGE_CURVE ( 'NONE', #23326, #50923, #86041, .T. ) ;
#17965 = DIRECTION ( 'NONE',  ( 0.9496245541219264785, 0.000000000000000000, 0.3133898629642195011 ) ) ;
#17966 = ORIENTED_EDGE ( 'NONE', *, *, #5788, .F. ) ;
#17967 = CARTESIAN_POINT ( 'NONE',  ( -20.47705334459679705, -22.77463087841388045, 11.50200000000000422 ) ) ;
#17968 = CARTESIAN_POINT ( 'NONE',  ( -104.5228709571500758, -23.47596703998600631, 11.44779298504228215 ) ) ;
#17969 = VECTOR ( 'NONE', #78296, 1000.000000000000114 ) ;
#17970 = CARTESIAN_POINT ( 'NONE',  ( -1.591348192139008466, -19.94584644712825039, -1.500000000000002220 ) ) ;
#17971 = CARTESIAN_POINT ( 'NONE',  ( 18.89479412359299815, 9.153864009170110450, 11.49999999999999645 ) ) ;
#17972 = CARTESIAN_POINT ( 'NONE',  ( -28.16800187962948598, -24.70123718975396798, 8.197761918552000537 ) ) ;
#17973 = CARTESIAN_POINT ( 'NONE',  ( -124.5194960560089612, -24.65952944569305316, 1.056160979905707009 ) ) ;
#17974 = CARTESIAN_POINT ( 'NONE',  ( 21.54648482299927181, -4.703075207800759827, 11.49999999999998934 ) ) ;
#17975 = CARTESIAN_POINT ( 'NONE',  ( -53.62287095715005592, -24.64965695001467694, 8.947790433994185832 ) ) ;
#17976 = ORIENTED_EDGE ( 'NONE', *, *, #93305, .T. ) ;
#17977 = DIRECTION ( 'NONE',  ( -0.000000000000000000, -1.000000000000000000, -0.000000000000000000 ) ) ;
#17978 = CARTESIAN_POINT ( 'NONE',  ( -49.52164473449563076, -25.18440224513725667, 3.857971350860132986 ) ) ;
#17979 = CARTESIAN_POINT ( 'NONE',  ( -72.63498201661158760, -24.15543982623907127, -0.2315651400026661755 ) ) ;
#17980 = VERTEX_POINT ( 'NONE', #99317 ) ;
#17981 = CARTESIAN_POINT ( 'NONE',  ( 2.590388488674697953, -6.376774720514415407, 19.94764386045124027 ) ) ;
#17982 = ORIENTED_EDGE ( 'NONE', *, *, #24937, .T. ) ;
#17983 = ORIENTED_EDGE ( 'NONE', *, *, #32131, .F. ) ;
#17984 = CARTESIAN_POINT ( 'NONE',  ( -80.62287095715005592, -29.50248789122583659, 2.256150453626215580 ) ) ;
#17985 = DIRECTION ( 'NONE',  ( -3.773278334453079030E-23, 0.9999999999976377785, 2.173523156925979128E-06 ) ) ;
#17986 = CARTESIAN_POINT ( 'NONE',  ( -122.5562042904834215, -23.48786465467241769, 11.44779295918253759 ) ) ;
#17987 = CARTESIAN_POINT ( 'NONE',  ( -5.951451697817415010, -19.63005813332872762, -1.500000000000002220 ) ) ;
#17988 = ORIENTED_EDGE ( 'NONE', *, *, #89143, .T. ) ;
#17989 = FACE_OUTER_BOUND ( 'NONE', #5166, .T. ) ;
#17990 = PLANE ( 'NONE',  #2941 ) ;
#17991 = CARTESIAN_POINT ( 'NONE',  ( -114.5228709571500616, -29.50250243563736774, 8.947779886222136270 ) ) ;
#17992 = CARTESIAN_POINT ( 'NONE',  ( -15.13915969582853549, -16.40262476207453801, -1.500000000000002220 ) ) ;
#17993 = CARTESIAN_POINT ( 'NONE',  ( -101.5228709571500758, -24.64965694238407323, 8.947790433994194714 ) ) ;
#17995 = EDGE_CURVE ( 'NONE', #96649, #15961, #53666, .T. ) ;
#17994 = LINE ( 'NONE', #33723, #75624 ) ;
#17996 = ORIENTED_EDGE ( 'NONE', *, *, #60573, .F. ) ;
#17997 = CARTESIAN_POINT ( 'NONE',  ( -43.55620429048338593, -24.65952944569304606, 1.056160979905693020 ) ) ;
#17998 = CARTESIAN_POINT ( 'NONE',  ( -6.741682653110981249, -0.3587747205144265483, 30.62569541381301619 ) ) ;
#17999 = CARTESIAN_POINT ( 'NONE',  ( 20.80141654084381386, -1.409215765453083469, 11.49999999999998934 ) ) ;
#18000 = VERTEX_POINT ( 'NONE', #68874 ) ;
#18002 = EDGE_LOOP ( 'NONE', ( #74390, #15510, #92244, #49321 ) ) ;
#18001 = CARTESIAN_POINT ( 'NONE',  ( -112.5228709571500616, -24.64965694238408034, 8.947790433994192938 ) ) ;
#18003 = ORIENTED_EDGE ( 'NONE', *, *, #94827, .T. ) ;
#18004 = CARTESIAN_POINT ( 'NONE',  ( -68.94101663640660149, -25.25935064844479783, 6.247842340801990524 ) ) ;
#18005 = CARTESIAN_POINT ( 'NONE',  ( 15.37114825158464271, 14.37155165002682544, -1.500000000000002220 ) ) ;
#18006 = EDGE_LOOP ( 'NONE', ( #64819, #65851, #52673, #63825 ) ) ;
#18007 = CARTESIAN_POINT ( 'NONE',  ( -89.52287095715006160, -29.50250786944525672, 11.44777988621623344 ) ) ;
#18008 = DIRECTION ( 'NONE',  ( 0.000000000000000000, -0.000000000000000000, -1.000000000000000000 ) ) ;
#18009 = FACE_OUTER_BOUND ( 'NONE', #71415, .T. ) ;
#18010 = CARTESIAN_POINT ( 'NONE',  ( -100.8646123533485621, -25.03152439226099091, 7.517421852973264151 ) ) ;
#18011 = CARTESIAN_POINT ( 'NONE',  ( -73.62287095715005592, -24.65952944569304606, 1.056160979905698794 ) ) ;
#18012 = CARTESIAN_POINT ( 'NONE',  ( 4.495418090846292181, 21.21921847905042569, -1.500000000000002220 ) ) ;
#18013 = CARTESIAN_POINT ( 'NONE',  ( -20.27875734969026311, -6.143225279485574397, 24.00402280011862288 ) ) ;
#18015 = VERTEX_POINT ( 'NONE', #29311 ) ;
#18014 = CARTESIAN_POINT ( 'NONE',  ( -17.34812393562427246, -13.96779696820907191, 11.49999999999999645 ) ) ;
#18016 = CARTESIAN_POINT ( 'NONE',  ( -50.92793838057655620, -25.31441747217130001, 5.312585239957233973 ) ) ;
#18017 = B_SPLINE_CURVE_WITH_KNOTS ( 'NONE', 3,
 ( #65122, #96042, #97040, #67110, #80317, #98019 ),
 .UNSPECIFIED., .F., .F.,
 ( 4, 2, 4 ),
 ( 6.384118678617895067E-06, 0.001386860460828379972, 0.002767336802978142326 ),
 .UNSPECIFIED. ) ;
#18018 = CARTESIAN_POINT ( 'NONE',  ( -54.55620429048339304, -24.64898659630528499, 1.056161002820821260 ) ) ;
#18019 = ORIENTED_EDGE ( 'NONE', *, *, #45555, .T. ) ;
#18021 = ORIENTED_EDGE ( 'NONE', *, *, #31712, .T. ) ;
#18020 = LINE ( 'NONE', #72319, #94397 ) ;
#18022 = VERTEX_POINT ( 'NONE', #46052 ) ;
#18023 = CIRCLE ( 'NONE', #53671, 1.306876713926001354 ) ;
#18024 = EDGE_CURVE ( 'NONE', #49490, #89148, #33932, .T. ) ;
#18025 = CARTESIAN_POINT ( 'NONE',  ( 11.25103634530202790, -16.72154935384561725, 11.49999999999998934 ) ) ;
#18026 = LINE ( 'NONE', #79419, #94335 ) ;
#18027 = ORIENTED_EDGE ( 'NONE', *, *, #88515, .F. ) ;
#18028 = CARTESIAN_POINT ( 'NONE',  ( -130.5728709571500588, -24.36716509058404156, 9.983964055416601369 ) ) ;
#18029 = CARTESIAN_POINT ( 'NONE',  ( 22.03792223356247604, -4.036589945906135846, -1.500000000000002220 ) ) ;
#18030 = VERTEX_POINT ( 'NONE', #91699 ) ;
#18031 = ORIENTED_EDGE ( 'NONE', *, *, #53126, .F. ) ;
#18032 = CARTESIAN_POINT ( 'NONE',  ( -112.5515187183059425, -24.51419770103158413, 9.386484678747166299 ) ) ;
#18033 = CARTESIAN_POINT ( 'NONE',  ( -101.5957436026087635, -23.73791477778911485, 11.05961554403170233 ) ) ;
#18034 = CARTESIAN_POINT ( 'NONE',  ( -24.90875734969025501, 5.965225279485572685, 30.00402280011862288 ) ) ;
#18035 = EDGE_CURVE ( 'NONE', #90358, #5613, #22183, .T. ) ;
#18036 = ADVANCED_FACE ( 'NONE', ( #7465 ), #4578, .T. ) ;
#18037 = CARTESIAN_POINT ( 'NONE',  ( -41.52287095715004739, -23.73907113217657283, -1.053371485781501526 ) ) ;
#18038 = EDGE_CURVE ( 'NONE', #76361, #1269, #35189, .T. ) ;
#18039 = CARTESIAN_POINT ( 'NONE',  ( -30.59162032554853639, -24.82935162629096482, 1.633150109380538950 ) ) ;
#18040 = AXIS2_PLACEMENT_3D ( 'NONE', #65749, #9934, #79946 ) ;
#18041 = CARTESIAN_POINT ( 'NONE',  ( -6.824658503225996320, 18.35159230250476270, 11.49999999999998934 ) ) ;
#18042 = CARTESIAN_POINT ( 'NONE',  ( -46.55319784584757770, -23.96119346886880308, -0.6495511937832144644 ) ) ;
#18044 = EDGE_CURVE ( 'NONE', #62667, #71923, #56170, .T. ) ;
#18043 = ORIENTED_EDGE ( 'NONE', *, *, #80633, .T. ) ;
#18045 = CARTESIAN_POINT ( 'NONE',  ( -0.8555947871142663974, 21.52075748220454798, -1.500000000000002220 ) ) ;
#18046 = CARTESIAN_POINT ( 'NONE',  ( -128.5214471550031305, -24.51314013834317151, 0.6176544820404290537 ) ) ;
#18047 = CARTESIAN_POINT ( 'NONE',  ( -114.5228709571500758, -23.94994826722565762, -0.6494450866342721396 ) ) ;
#18048 = CARTESIAN_POINT ( 'NONE',  ( -101.7587321196599532, -25.26650786476337984, 3.907930402413430482 ) ) ;
#18049 = DIRECTION ( 'NONE',  ( -3.773278334453079030E-23, 0.9999999999976377785, 2.173523156925979128E-06 ) ) ;
#18050 = CARTESIAN_POINT ( 'NONE',  ( 11.31314246093949727, 19.96360691973900359, -1.500000000000002220 ) ) ;
#18051 = PERSON_AND_ORGANIZATION_ROLE ( 'design_owner' ) ;
#18052 = CARTESIAN_POINT ( 'NONE',  ( -93.62287095715008434, -24.34917612406837861, 0.1852690917426652040 ) ) ;
#18053 = CARTESIAN_POINT ( 'NONE',  ( -49.66058267289122341, -23.48783264082477018, -1.443836473390093911 ) ) ;
#18054 = CARTESIAN_POINT ( 'NONE',  ( -11.36185547594953249, 16.55520930037988592, 11.49999999999999645 ) ) ;
#18055 = CARTESIAN_POINT ( 'NONE',  ( -8.499999999999987566, 19.99999999999999289, 0.000000000000000000 ) ) ;
#18056 = DIRECTION ( 'NONE',  ( -3.773278334453079618E-23, 0.9999999999976377785, 2.173523156925979975E-06 ) ) ;
#18057 = PLANE ( 'NONE',  #92753 ) ;
#18058 = FACE_OUTER_BOUND ( 'NONE', #60120, .T. ) ;
#18059 = CARTESIAN_POINT ( 'NONE',  ( 14.61581676223891613, 3.582999323269832725, -27.35847991879931485 ) ) ;
#18061 = EDGE_CURVE ( 'NONE', #98531, #20076, #15586, .T. ) ;
#18060 = CARTESIAN_POINT ( 'NONE',  ( 18.78741845327603599, -6.401996767227196905, -1.500000000000002220 ) ) ;
#18062 = DIRECTION ( 'NONE',  ( 1.000000000000000000, 0.000000000000000000, -2.168404344971008868E-16 ) ) ;
#18063 = CARTESIAN_POINT ( 'NONE',  ( -10.66912846187372210, -16.51573522771486324, -1.500000000000002220 ) ) ;
#18064 = DIRECTION ( 'NONE',  ( -0.000000000000000000, -0.000000000000000000, -1.000000000000000000 ) ) ;
#18065 = EDGE_CURVE ( 'NONE', #92149, #40482, #6063, .T. ) ;
#18066 = CARTESIAN_POINT ( 'NONE',  ( -58.55620429048339304, -23.48786465467241058, 11.44779295918254469 ) ) ;
#18067 = CALENDAR_DATE ( 2026, 9, 10 ) ;
#18068 = CARTESIAN_POINT ( 'NONE',  ( -57.52287095715003318, -23.95044443724990657, 10.65354141964648882 ) ) ;
#18069 = CARTESIAN_POINT ( 'NONE',  ( 2.598243466966731585, -6.376774720514413630, 20.31174627870924709 ) ) ;
#18070 = CARTESIAN_POINT ( 'NONE',  ( 6.296002175621457475, 19.65409743616946514, 11.49999999999999645 ) ) ;
#18071 = CARTESIAN_POINT ( 'NONE',  ( 4.415069475862049231, -6.376774720514424288, 21.13806644168711557 ) ) ;
#18072 = ADVANCED_FACE ( 'NONE', ( #9475 ), #1871, .T. ) ;
#18073 = CARTESIAN_POINT ( 'NONE',  ( -120.5877768927123412, -25.00158670708911046, 2.256160236439219258 ) ) ;
#18074 = CARTESIAN_POINT ( 'NONE',  ( -14.16962031475959272, 17.58799634409329471, 11.49999999999999645 ) ) ;
#18075 = CIRCLE ( 'NONE', #97524, 1.306876713926001798 ) ;
#18076 = ORIENTED_EDGE ( 'NONE', *, *, #25593, .F. ) ;
#18077 = CARTESIAN_POINT ( 'NONE',  ( -69.38174606678134637, -25.25639464550703295, 6.471609011167150705 ) ) ;
#18078 = DIRECTION ( 'NONE',  ( 1.000000000000000000, 3.773278334444166432E-23, 8.201307841325785021E-29 ) ) ;
#18079 = CARTESIAN_POINT ( 'NONE',  ( 30.61643171304412903, 3.316774720514426456, 27.37433008668283207 ) ) ;
#18080 = CARTESIAN_POINT ( 'NONE',  ( -39.62287095715004170, -23.94994826722515313, -0.6494450866351729745 ) ) ;
#18081 = B_SPLINE_CURVE_WITH_KNOTS ( 'NONE', 3,
 ( #94378, #9646, #2050, #78134 ),
 .UNSPECIFIED., .F., .F.,
 ( 4, 4 ),
 ( 0.000000000000000000, 9.999999999998897304E-05 ),
 .UNSPECIFIED. ) ;
#18082 = CARTESIAN_POINT ( 'NONE',  ( -26.59548113855183615, -24.93063557578396328, 7.895922241538460895 ) ) ;
#18083 = EDGE_CURVE ( 'NONE', #36438, #34988, #53345, .T. ) ;
#18084 = CARTESIAN_POINT ( 'NONE',  ( -75.58953762381673869, -23.47593901973091235, -1.443836447539004642 ) ) ;
#18085 = EDGE_CURVE ( 'NONE', #47977, #12723, #75478, .T. ) ;
#18086 = VERTEX_POINT ( 'NONE', #71891 ) ;
#18087 = CARTESIAN_POINT ( 'NONE',  ( -80.43221577628075636, -25.26749876250476490, 4.967019860322055891 ) ) ;
#18088 = CARTESIAN_POINT ( 'NONE',  ( -22.57016884136470125, -3.422276288085174478, -1.500000000000002220 ) ) ;
#18090 = EDGE_CURVE ( 'NONE', #27395, #38340, #56674, .T. ) ;
#18089 = CARTESIAN_POINT ( 'NONE',  ( -74.49656298872699267, -24.65952944569304606, 1.056160979905701902 ) ) ;
#18091 = CARTESIAN_POINT ( 'NONE',  ( -122.6228709571500417, -29.50250786944525672, 11.44777988621622811 ) ) ;
#18092 = FACE_OUTER_BOUND ( 'NONE', #27702, .T. ) ;
#18093 = CARTESIAN_POINT ( 'NONE',  ( -19.72384299526936857, -10.77339039931002773, 11.49999999999999645 ) ) ;
#18094 = ORIENTED_EDGE ( 'NONE', *, *, #57130, .F. ) ;
#18095 = CYLINDRICAL_SURFACE ( 'NONE', #57849, 6.099999999999999645 ) ;
#18096 = VECTOR ( 'NONE', #16046, 1000.000000000000114 ) ;
#18097 = CARTESIAN_POINT ( 'NONE',  ( -21.97012646571106842, -0.5360883523215664859, 11.49999999999998934 ) ) ;
#18098 = CARTESIAN_POINT ( 'NONE',  ( -54.62287095715007723, -24.34917612406837861, 0.1852690917426598194 ) ) ;
#18099 = CARTESIAN_POINT ( 'NONE',  ( -34.52200844785745204, -23.48786465467240347, 11.44779295918255535 ) ) ;
#18100 = FACE_OUTER_BOUND ( 'NONE', #62262, .T. ) ;
#18101 = VERTEX_POINT ( 'NONE', #10473 ) ;
#18102 = CARTESIAN_POINT ( 'NONE',  ( -51.70072539166535108, -25.27314792116673203, 3.987152059579775809 ) ) ;
#18103 = DIRECTION ( 'NONE',  ( 1.000000000000000000, 3.773278334444167608E-23, 8.201307833595939069E-29 ) ) ;
#18104 = ORIENTED_EDGE ( 'NONE', *, *, #22488, .F. ) ;
#18105 = CARTESIAN_POINT ( 'NONE',  ( -54.53711127335206044, -24.51419770103157347, 9.386484678747178734 ) ) ;
#18106 = CARTESIAN_POINT ( 'NONE',  ( 16.11427877760282001, 12.65940972936023812, 11.49999999999998934 ) ) ;
#18107 = APPLICATION_CONTEXT ( 'configuration controlled 3d designs of mechanical parts and assemblies' ) ;
#18108 = EDGE_LOOP ( 'NONE', ( #6266, #50302, #60210, #79753 ) ) ;
#18109 = ORIENTED_EDGE ( 'NONE', *, *, #24836, .T. ) ;
#18110 = VERTEX_POINT ( 'NONE', #41431 ) ;
#18111 = ORIENTED_EDGE ( 'NONE', *, *, #17729, .F. ) ;
#18112 = CARTESIAN_POINT ( 'NONE',  ( -84.62287095715004170, -24.34917612406837861, 0.1852690917426652040 ) ) ;
#18113 = CARTESIAN_POINT ( 'NONE',  ( 11.75533340255842596, 19.88161105567325038, -1.500000000000002220 ) ) ;
#18114 = CARTESIAN_POINT ( 'NONE',  ( -104.6250114612373494, -24.51419770103158768, 9.386484678747164523 ) ) ;
#18115 = CARTESIAN_POINT ( 'NONE',  ( -16.75749313124890350, -11.57646860041911019, -1.500000000000002220 ) ) ;
#18116 = EDGE_LOOP ( 'NONE', ( #34364, #77960, #68670, #16344 ) ) ;
#18117 = CARTESIAN_POINT ( 'NONE',  ( 29.71114493364435916, 4.339464138238508184, 27.93491297891351621 ) ) ;
#18118 = CARTESIAN_POINT ( 'NONE',  ( 33.74607884027702909, 0.3587747205144265483, -4.999864028243830916 ) ) ;
#18119 = CARTESIAN_POINT ( 'NONE',  ( 31.64143112576189765, -0.3587747205144265483, 14.03360796525321774 ) ) ;
#18120 = CARTESIAN_POINT ( 'NONE',  ( -70.48669981260067630, -25.00158670708910691, 2.256160236439221034 ) ) ;
#18121 = ORIENTED_EDGE ( 'NONE', *, *, #26642, .F. ) ;
#18122 = FACE_OUTER_BOUND ( 'NONE', #1288, .T. ) ;
#18123 = CARTESIAN_POINT ( 'NONE',  ( -49.11003834631243592, -25.26385671119021836, 4.144493137612085043 ) ) ;
#18124 = LOCAL_TIME ( 0, 54, 15.00000000000000000, #40890 ) ;
#18125 = EDGE_LOOP ( 'NONE', ( #36737, #94143, #9761, #69540 ) ) ;
#18126 = CARTESIAN_POINT ( 'NONE',  ( -18.04518632387085830, 10.29925911722504317, -1.500000000000002220 ) ) ;
#18127 = ORIENTED_EDGE ( 'NONE', *, *, #67198, .T. ) ;
#18129 = ORIENTED_EDGE ( 'NONE', *, *, #64581, .T. ) ;
#18128 = CARTESIAN_POINT ( 'NONE',  ( -91.52287095715006160, -24.64898659630368272, 1.056161002820827921 ) ) ;
#18130 = CYLINDRICAL_SURFACE ( 'NONE', #42248, 3.060000000000000053 ) ;
#18131 = CARTESIAN_POINT ( 'NONE',  ( -40.62287095715004170, -25.00158670708908204, 2.256160236439166411 ) ) ;
#18132 = VERTEX_POINT ( 'NONE', #33815 ) ;
#18133 = VERTEX_POINT ( 'NONE', #64800 ) ;
#18134 = LINE ( 'NONE', #49103, #47781 ) ;
#18135 = CARTESIAN_POINT ( 'NONE',  ( -127.6228709571500559, -29.50250786944525672, 11.44777988621622633 ) ) ;
#18136 = DIRECTION ( 'NONE',  ( -0.8788171126619707119, 0.4771587602595986910, -0.000000000000000000 ) ) ;
#18138 = ORIENTED_EDGE ( 'NONE', *, *, #45920, .F. ) ;
#18137 = CARTESIAN_POINT ( 'NONE',  ( -22.07534667767119174, -0.2742745133902674826, 11.49999999999999645 ) ) ;
#18139 = CARTESIAN_POINT ( 'NONE',  ( -48.87575205656965238, -25.25459236073634983, 6.222261992663564278 ) ) ;
#18140 = CARTESIAN_POINT ( 'NONE',  ( -20.50338545487000275, 9.463669735852004550, 11.49999999999998934 ) ) ;
#18142 = ORIENTED_EDGE ( 'NONE', *, *, #91154, .T. ) ;
#18141 = CARTESIAN_POINT ( 'NONE',  ( -70.62287095715005592, -23.47593901973091235, -1.443836447539006196 ) ) ;
#18143 = ORIENTED_EDGE ( 'NONE', *, *, #8547, .T. ) ;
#18144 = CARTESIAN_POINT ( 'NONE',  ( -88.52287095715010423, -24.51387760970724727, 9.387446482453404073 ) ) ;
#18145 = AXIS2_PLACEMENT_3D ( 'NONE', #49120, #88671, #19142 ) ;
#18146 = DIRECTION ( 'NONE',  ( -3.773278334453079030E-23, 0.9999999999976377785, 2.173523156925979128E-06 ) ) ;
#18147 = VERTEX_POINT ( 'NONE', #95716 ) ;
#18148 = CARTESIAN_POINT ( 'NONE',  ( -0.1268723920767304558, 21.18662008908366445, 11.49999999999998934 ) ) ;
#18149 = CARTESIAN_POINT ( 'NONE',  ( -34.62287095715003460, -23.73934037231755667, 11.05740245334329508 ) ) ;
#18150 = ADVANCED_FACE ( 'NONE', ( #49555 ), #72324, .F. ) ;
#18151 = CARTESIAN_POINT ( 'NONE',  ( 29.71615239255367413, -4.563867803339911156, 27.78418661847934246 ) ) ;
#18152 = DIRECTION ( 'NONE',  ( 0.000000000000000000, -1.000000000000000000, 0.000000000000000000 ) ) ;
#18153 = DIRECTION ( 'NONE',  ( -1.000000000000000000, -3.773278334444167608E-23, -8.201307833595939069E-29 ) ) ;
#18154 = CARTESIAN_POINT ( 'NONE',  ( -15.91109736606077441, 15.52988587838853540, -1.500000000000002220 ) ) ;
#18155 = EDGE_CURVE ( 'NONE', #89454, #92378, #11975, .T. ) ;
#18156 = CARTESIAN_POINT ( 'NONE',  ( -114.5180551983652322, -24.15543982623907837, -0.2315651400026444429 ) ) ;
#18157 = ADVANCED_FACE ( 'NONE', ( #10980 ), #33684, .T. ) ;
#18158 = ORIENTED_EDGE ( 'NONE', *, *, #81844, .T. ) ;
#18159 = CARTESIAN_POINT ( 'NONE',  ( -112.5228709571500474, -24.51283580621457858, 0.6167428607047616973 ) ) ;
#18160 = CARTESIAN_POINT ( 'NONE',  ( -4.286263797015736595E-16, -4.056774720514426669, -3.500000000000000000 ) ) ;
#18161 = CARTESIAN_POINT ( 'NONE',  ( 11.20917403917954225, 15.81763734437701885, 11.49999999999999645 ) ) ;
#18162 = ADVANCED_FACE ( 'NONE', ( #12961 ), #50541, .F. ) ;
#18163 = EDGE_CURVE ( 'NONE', #80744, #64204, #13922, .T. ) ;
#18164 = DIRECTION ( 'NONE',  ( -0.000000000000000000, -0.000000000000000000, -1.000000000000000000 ) ) ;
#18165 = CARTESIAN_POINT ( 'NONE',  ( -77.62287095715005592, -23.47593901973091235, -1.443836447539004642 ) ) ;
#18166 = CARTESIAN_POINT ( 'NONE',  ( 16.53150372360616771, 10.32350692489952593, 11.49999999999998934 ) ) ;
#18167 = CARTESIAN_POINT ( 'NONE',  ( 21.39645853268639186, 0.3907444525687319703, 11.49999999999998934 ) ) ;
#18168 = CARTESIAN_POINT ( 'NONE',  ( -62.52287095715006160, -23.47596703998600631, 11.44779298504228926 ) ) ;
#18169 = DIRECTION ( 'NONE',  ( 0.000000000000000000, 0.000000000000000000, 1.000000000000000000 ) ) ;
#18170 = VECTOR ( 'NONE', #79209, 1000.000000000000000 ) ;
#18171 = DIRECTION ( 'NONE',  ( -3.773278334453079618E-23, 0.9999999999976377785, 2.173523156925979975E-06 ) ) ;
#18172 = CARTESIAN_POINT ( 'NONE',  ( -77.50095171770020386, -24.51314013834315375, 0.6176544820404117342 ) ) ;
#18173 = CARTESIAN_POINT ( 'NONE',  ( 6.135622925040504327, -21.92205258971886650, -1.500000000000002220 ) ) ;
#18174 = DIRECTION ( 'NONE',  ( 1.000000000000000000, -1.009709539272096573E-17, 1.369364893872201492E-16 ) ) ;
#18175 = CARTESIAN_POINT ( 'NONE',  ( -102.5855002951087585, -24.65952944569305316, 1.056160979905705677 ) ) ;
#18176 = CARTESIAN_POINT ( 'NONE',  ( -127.6228709571500559, -23.48783264082479505, -1.443836473390056829 ) ) ;
#18177 = CARTESIAN_POINT ( 'NONE',  ( 10.08953278062578462, 17.19620541797624824, 11.49999999999999645 ) ) ;
#18178 = CARTESIAN_POINT ( 'NONE',  ( -31.52287095715006160, -23.47593901973090169, -1.443836447538997536 ) ) ;
#18179 = CARTESIAN_POINT ( 'NONE',  ( -39.63465047039538547, -24.35071581493543036, 9.817618358456035921 ) ) ;
#18180 = FACE_OUTER_BOUND ( 'NONE', #59110, .T. ) ;
#18181 = ORIENTED_EDGE ( 'NONE', *, *, #74807, .F. ) ;
#18182 = PLANE ( 'NONE',  #31500 ) ;
#18183 = EDGE_CURVE ( 'NONE', #17742, #34210, #99805, .T. ) ;
#18184 = CARTESIAN_POINT ( 'NONE',  ( -77.52287095715007581, -24.51283580621364422, 0.6167428607019788123 ) ) ;
#18185 = LOCAL_TIME ( 0, 54, 15.00000000000000000, #80467 ) ;
#18186 = CARTESIAN_POINT ( 'NONE',  ( -17.90551237062050305, -12.20792721910736667, 11.49999999999998934 ) ) ;
#18187 = CARTESIAN_POINT ( 'NONE',  ( -35.52287095715006870, -29.50250243563736774, 8.947779886222148704 ) ) ;
#18188 = CARTESIAN_POINT ( 'NONE',  ( 12.63578256557813795, 14.83599306707809085, -1.500000000000002220 ) ) ;
#18189 = CARTESIAN_POINT ( 'NONE',  ( -93.52287095715010423, -24.34917612406837861, 0.1852690917426536021 ) ) ;
#18190 = VECTOR ( 'NONE', #36879, 1000.000000000000000 ) ;
#18191 = EDGE_CURVE ( 'NONE', #13725, #33057, #90596, .T. ) ;
#18192 = VERTEX_POINT ( 'NONE', #52042 ) ;
#18193 = LOCAL_TIME ( 0, 54, 15.00000000000000000, #17426 ) ;
#18194 = CARTESIAN_POINT ( 'NONE',  ( -86.62287095715004170, -29.50247984919015209, -1.443849546365051806 ) ) ;
#18195 = CARTESIAN_POINT ( 'NONE',  ( 5.028806042385554953, -19.83023610923392610, 11.49999999999999645 ) ) ;
#18196 = LINE ( 'NONE', #17188, #34349 ) ;
#18197 = DIRECTION ( 'NONE',  ( 5.238131417152343399E-15, 0.000000000000000000, -1.000000000000000000 ) ) ;
#18198 = EDGE_LOOP ( 'NONE', ( #60927, #87393, #28449, #65498, #47694, #21931 ) ) ;
#18199 = CARTESIAN_POINT ( 'NONE',  ( -72.52287095715007581, -23.96127896941631619, -0.6493128931038039120 ) ) ;
#18200 = CARTESIAN_POINT ( 'NONE',  ( 33.55975867735808293, 4.270419025147584868, -12.32584534477734728 ) ) ;
#18201 = CARTESIAN_POINT ( 'NONE',  ( -39.04762117679405264, -25.31628479640222906, 4.358277408297509758 ) ) ;
#18202 = B_SPLINE_CURVE_WITH_KNOTS ( 'NONE', 3,
 ( #51575, #36848, #28229, #13988 ),
 .UNSPECIFIED., .F., .F.,
 ( 4, 4 ),
 ( 0.3007147330300765087, 0.3097211643021920424 ),
 .UNSPECIFIED. ) ;
#18203 = CARTESIAN_POINT ( 'NONE',  ( -110.6228709571500559, -29.50247984919015209, -1.443849546365048253 ) ) ;
#18204 = LINE ( 'NONE', #97198, #80323 ) ;
#18205 = CARTESIAN_POINT ( 'NONE',  ( -109.5151497621329213, -24.34968618360934300, 0.1864209137778879422 ) ) ;
#18206 = ORIENTED_EDGE ( 'NONE', *, *, #15175, .T. ) ;
#18207 = CARTESIAN_POINT ( 'NONE',  ( -66.51027937953499247, -23.96169478059713143, 10.65365249895718058 ) ) ;
#18208 = ADVANCED_FACE ( 'NONE', ( #41945 ), #34821, .T. ) ;
#18209 = CARTESIAN_POINT ( 'NONE',  ( 3.929728083993185184, -22.62717521373229701, 11.49999999999999645 ) ) ;
#18210 = CARTESIAN_POINT ( 'NONE',  ( 18.68554041145753786, -12.99315341008173519, -1.500000000000002220 ) ) ;
#18211 = CARTESIAN_POINT ( 'NONE',  ( -110.6241301225872888, -24.92592662359561828, 8.075495903018000021 ) ) ;
#18212 = B_SPLINE_SURFACE_WITH_KNOTS ( 'NONE', 3, 3, ( 
 ( #47748, #17287, #33021, #78167 ),
 ( #61972, #16283, #92899, #31006 ),
 ( #39621, #63996, #48251, #47243 ),
 ( #23376, #70072, #8681, #40638 ) ),
 .UNSPECIFIED., .F., .F., .F.,
 ( 4, 4 ),
 ( 4, 4 ),
 ( 0.5218268152168922258, 0.6546831510031384527 ),
 ( 0.5925805111453674723, 0.6124317898845940134 ),
 .UNSPECIFIED. ) ;
#18213 = CARTESIAN_POINT ( 'NONE',  ( -11.64875734969026233, -0.3587747205144265483, 31.02402280011862246 ) ) ;
#18214 = CARTESIAN_POINT ( 'NONE',  ( -113.6228709571500559, -24.65952944569304961, 1.056160979905706565 ) ) ;
#18215 = DIRECTION ( 'NONE',  ( 0.000000000000000000, 0.000000000000000000, 1.000000000000000000 ) ) ;
#18216 = CARTESIAN_POINT ( 'NONE',  ( -82.62287095715005592, -23.48783264082478084, -1.443836473390065933 ) ) ;
#18217 = EDGE_CURVE ( 'NONE', #98343, #47218, #57665, .T. ) ;
#18218 = CARTESIAN_POINT ( 'NONE',  ( -1.606994170628035068, 21.82944698466814870, 11.49999999999998934 ) ) ;
#18219 = FACE_OUTER_BOUND ( 'NONE', #16114, .T. ) ;
#18220 = AXIS2_PLACEMENT_3D ( 'NONE', #34380, #11041, #33877 ) ;
#18221 = CARTESIAN_POINT ( 'NONE',  ( -115.6228709571500417, -23.85196035786902513, -0.8779234886474898136 ) ) ;
#18222 = PLANE ( 'NONE',  #32250 ) ;
#18223 = PLANE ( 'NONE',  #12819 ) ;
#18224 = ORIENTED_EDGE ( 'NONE', *, *, #61337, .T. ) ;
#18225 = PRODUCT_DEFINITION_SHAPE ( 'NONE', 'NONE',  #100422 ) ;
#18226 = CARTESIAN_POINT ( 'NONE',  ( -16.87313589883980214, -11.49665204554024989, 11.49999999999998934 ) ) ;
#18227 = ORIENTED_EDGE ( 'NONE', *, *, #98310, .F. ) ;
#18228 = VERTEX_POINT ( 'NONE', #42448 ) ;
#18229 = CARTESIAN_POINT ( 'NONE',  ( 10.47623847176155820, -20.49086732513842080, 11.49999999999998934 ) ) ;
#18230 = CARTESIAN_POINT ( 'NONE',  ( 31.93426202889373400, -5.965225279485572685, 6.907000118922836940 ) ) ;
#18231 = VERTEX_POINT ( 'NONE', #58164 ) ;
#18232 = CARTESIAN_POINT ( 'NONE',  ( -32.52287095715006160, -29.50248528299804818, 1.056150453629029817 ) ) ;
#18233 = CARTESIAN_POINT ( 'NONE',  ( -50.22287095715005734, -23.47593901973090169, -1.443836447538997980 ) ) ;
#18234 = LINE ( 'NONE', #11118, #38172 ) ;
#18235 = CARTESIAN_POINT ( 'NONE',  ( -53.48691055854919085, -24.66019654487199375, 8.947790411086122830 ) ) ;
#18237 = ORIENTED_EDGE ( 'NONE', *, *, #36265, .F. ) ;
#18236 = CARTESIAN_POINT ( 'NONE',  ( 20.74164082462262471, 5.259929546262127609, 11.49999999999999645 ) ) ;
#18238 = CIRCLE ( 'NONE', #74928, 2.249999999999998668 ) ;
#18239 = EDGE_LOOP ( 'NONE', ( #96702, #99328, #11265, #78231 ) ) ;
#18240 = CARTESIAN_POINT ( 'NONE',  ( -20.66209241242137296, -8.185968977665980972, 11.49999999999998934 ) ) ;
#18241 = CARTESIAN_POINT ( 'NONE',  ( 7.914317726235799100, 19.11507755054979896, -1.500000000000002220 ) ) ;
#18242 = EDGE_LOOP ( 'NONE', ( #35900, #13266, #45234, #49572, #70198 ) ) ;
#18243 = CARTESIAN_POINT ( 'NONE',  ( -6.072964844751159497, -5.876774720514410077, 19.44316438561912008 ) ) ;
#18244 = CARTESIAN_POINT ( 'NONE',  ( 3.672440828437461224, -5.876774720514403860, 18.52532110411518573 ) ) ;
#18245 = ORIENTED_EDGE ( 'NONE', *, *, #89441, .T. ) ;
#18246 = DIRECTION ( 'NONE',  ( 0.000000000000000000, -0.9999999999976377785, -2.173523156925979975E-06 ) ) ;
#18247 = ORIENTED_EDGE ( 'NONE', *, *, #25756, .F. ) ;
#18248 = CARTESIAN_POINT ( 'NONE',  ( -91.52287095715006160, -24.64898659630368272, 1.056161002820827921 ) ) ;
#18249 = CARTESIAN_POINT ( 'NONE',  ( -70.32380231474228083, -25.12298712672050982, 7.101635559041870494 ) ) ;
#18250 = CARTESIAN_POINT ( 'NONE',  ( 20.36350155627077640, -4.707376482769925374, -1.500000000000002220 ) ) ;
#18251 = CARTESIAN_POINT ( 'NONE',  ( 13.86046232669119149, 16.88393516940953276, 11.49999999999999645 ) ) ;
#18252 = DIRECTION ( 'NONE',  ( 4.986391167143583514E-16, -1.000000000000000000, 0.000000000000000000 ) ) ;
#18253 = FACE_OUTER_BOUND ( 'NONE', #19221, .T. ) ;
#18254 = CARTESIAN_POINT ( 'NONE',  ( 22.09666729679958053, 4.251135690456572469, -1.500000000000002220 ) ) ;
#18255 = CARTESIAN_POINT ( 'NONE',  ( -9.975069251262826953, -18.38325097723136992, -1.500000000000002220 ) ) ;
#18256 = CARTESIAN_POINT ( 'NONE',  ( -26.10989220437014424, -24.97066886156136079, 5.384402865666523041 ) ) ;
#18257 = CARTESIAN_POINT ( 'NONE',  ( -53.58953762381672448, -24.64898659630528499, 1.056161002820821704 ) ) ;
#18258 = VECTOR ( 'NONE', #29641, 1000.000000000000000 ) ;
#18259 = CARTESIAN_POINT ( 'NONE',  ( -31.24388727629347784, -24.87219037989215309, 1.747789950310770779 ) ) ;
#18260 = VERTEX_POINT ( 'NONE', #73878 ) ;
#18261 = APPROVAL_PERSON_ORGANIZATION ( #86323, #28897, #63006 ) ;
#18262 = ORIENTED_EDGE ( 'NONE', *, *, #19539, .T. ) ;
#18263 = ORIENTED_EDGE ( 'NONE', *, *, #74378, .F. ) ;
#18264 = CARTESIAN_POINT ( 'NONE',  ( -38.62287095715005592, -24.66019654487199020, 8.947790411086137041 ) ) ;
#18265 = ORIENTED_EDGE ( 'NONE', *, *, #38909, .F. ) ;
#18266 = CARTESIAN_POINT ( 'NONE',  ( 18.17913347391500523, 11.28257676469832660, -1.500000000000002220 ) ) ;
#18267 = VECTOR ( 'NONE', #29407, 1000.000000000000114 ) ;
#18268 = CARTESIAN_POINT ( 'NONE',  ( 22.01400519847025450, -3.885951517071169370, 11.49999999999999645 ) ) ;
#18269 = ORIENTED_EDGE ( 'NONE', *, *, #75986, .T. ) ;
#18270 = FACE_OUTER_BOUND ( 'NONE', #19266, .T. ) ;
#18271 = CARTESIAN_POINT ( 'NONE',  ( -12.45680796028966597, 17.00782699154285638, 11.49999999999998934 ) ) ;
#18272 = CARTESIAN_POINT ( 'NONE',  ( -30.57655019826978560, -25.31558489090919650, 5.002391647799127483 ) ) ;
#18273 = ADVANCED_FACE ( 'NONE', ( #4377 ), #66286, .T. ) ;
#18274 = CARTESIAN_POINT ( 'NONE',  ( 3.050049012211247579, -6.376774720514426065, 21.53019692557248632 ) ) ;
#18275 = DIRECTION ( 'NONE',  ( 0.000000000000000000, 0.000000000000000000, -1.000000000000000000 ) ) ;
#18276 = CARTESIAN_POINT ( 'NONE',  ( -80.74930246458728789, -25.29534355928818457, 4.554285777995756845 ) ) ;
#18277 = CARTESIAN_POINT ( 'NONE',  ( 13.08019894233326319, 17.74467248152726384, -1.500000000000002220 ) ) ;
#18278 = EDGE_LOOP ( 'NONE', ( #54098, #72833, #45806, #73511 ) ) ;
#18279 = CARTESIAN_POINT ( 'NONE',  ( -65.63042416189901473, -24.73531770709095312, 8.716586749053508498 ) ) ;
#18280 = ADVANCED_FACE ( 'NONE', ( #53547 ), #67784, .T. ) ;
#18281 = LINE ( 'NONE', #95405, #27106 ) ;
#18282 = CARTESIAN_POINT ( 'NONE',  ( -27.96875734969026084, -3.316774720514426456, 24.50402280011861933 ) ) ;
#18283 = ADVANCED_FACE ( 'NONE', ( #84972 ), #45437, .T. ) ;
#18284 = CARTESIAN_POINT ( 'NONE',  ( -29.85518128034571461, -24.80592719104361521, 8.290116722409051064 ) ) ;
#18285 = EDGE_CURVE ( 'NONE', #20207, #87834, #29694, .T. ) ;
#18286 = PLANE ( 'NONE',  #50569 ) ;
#18287 = CARTESIAN_POINT ( 'NONE',  ( -38.62287095715004881, -24.35013146730202038, 9.818937971375113705 ) ) ;
#18288 = CARTESIAN_POINT ( 'NONE',  ( 1.434216325579209750, -21.26356369375713484, 11.49999999999998934 ) ) ;
#18289 = DIRECTION ( 'NONE',  ( 0.000000000000000000, 0.000000000000000000, 1.000000000000000000 ) ) ;
#18290 = ADVANCED_FACE ( 'NONE', ( #21566 ), #22066, .T. ) ;
#18291 = CARTESIAN_POINT ( 'NONE',  ( -117.5228709571501184, -24.35013146730205236, 9.818937971375092388 ) ) ;
#18292 = CARTESIAN_POINT ( 'NONE',  ( -37.62287095715005592, -29.50250786944525672, 11.44777988621624232 ) ) ;
#18293 = FACE_OUTER_BOUND ( 'NONE', #45181, .T. ) ;
#18294 = CARTESIAN_POINT ( 'NONE',  ( 21.27769986149581172, 7.469961712261545372, -1.500000000000002220 ) ) ;
#18295 = VECTOR ( 'NONE', #21382, 1000.000000000000000 ) ;
#18296 = B_SPLINE_SURFACE_WITH_KNOTS ( 'NONE', 3, 3, ( 
 ( #57307, #10602, #95341, #3008 ),
 ( #33945, #64925, #32949, #11102 ),
 ( #65918, #71518, #48179, #34447 ),
 ( #96341, #72020, #25828, #26332 ),
 ( #50175, #96835, #79109, #9604 ),
 ( #40566, #2503, #2002, #25326 ),
 ( #63922, #48689, #79612, #60788 ) ),
 .UNSPECIFIED., .F., .F., .F.,
 ( 4, 3, 4 ),
 ( 4, 4 ),
 ( 0.7945040050992244751, 0.8970133687736505657, 0.9995227324480766562 ),
 ( 0.6096489174824381019, 0.6109430964335138547 ),
 .UNSPECIFIED. ) ;
#18297 = CARTESIAN_POINT ( 'NONE',  ( -89.40841769935769889, -25.23397913219577049, 6.409327625469732226 ) ) ;
#18298 = EDGE_LOOP ( 'NONE', ( #85616, #12978 ) ) ;
#18299 = CARTESIAN_POINT ( 'NONE',  ( -35.62287095715005592, -25.00182538069145011, 7.747789668545097541 ) ) ;
#18300 = CARTESIAN_POINT ( 'NONE',  ( 30.00738719773716312, 4.772774720514425972, -9.049252915307087974 ) ) ;
#18301 = CARTESIAN_POINT ( 'NONE',  ( -9.297559507673007317, 17.40068379117045083, 11.49999999999999645 ) ) ;
#18302 = CARTESIAN_POINT ( 'NONE',  ( -0.02075734969026423599, -0.3587747205144213303, -0.08597719988137648983 ) ) ;
#18303 = CARTESIAN_POINT ( 'NONE',  ( -67.58779132469727813, -24.34968618360933235, 0.1864209137778811143 ) ) ;
#18304 = EDGE_LOOP ( 'NONE', ( #23275, #29257, #65944, #44344 ) ) ;
#18305 = CARTESIAN_POINT ( 'NONE',  ( -19.77875734969026311, -6.143225279485574397, 29.49402280011862487 ) ) ;
#18306 = LINE ( 'NONE', #32526, #91784 ) ;
#18307 = AXIS2_PLACEMENT_3D ( 'NONE', #13365, #66700, #97120 ) ;
#18308 = CARTESIAN_POINT ( 'NONE',  ( -124.5202219396526857, -24.35071581493544457, 9.817618358456016381 ) ) ;
#18309 = LINE ( 'NONE', #3594, #3226 ) ;
#18311 = EDGE_CURVE ( 'NONE', #40376, #24964, #60664, .T. ) ;
#18310 = CARTESIAN_POINT ( 'NONE',  ( -120.5895376238167245, -24.99132157543166954, 2.256160258750667502 ) ) ;
#18312 = CARTESIAN_POINT ( 'NONE',  ( -68.52287095715006160, -24.64965694238407323, 8.947790433994200043 ) ) ;
#18313 = CARTESIAN_POINT ( 'NONE',  ( 5.507670110241905448, 19.00313184189250038, -1.500000000000002220 ) ) ;
#18314 = ORIENTED_EDGE ( 'NONE', *, *, #99023, .T. ) ;
#18315 = VECTOR ( 'NONE', #75326, 1000.000000000000114 ) ;
#18316 = CARTESIAN_POINT ( 'NONE',  ( 13.23653054071972512, 15.24542462990338088, 11.49999999999999645 ) ) ;
#18317 = CARTESIAN_POINT ( 'NONE',  ( 6.127395130496778641, -5.876774720514417183, 20.13872869980892943 ) ) ;
#18318 = EDGE_LOOP ( 'NONE', ( #77533, #77212, #23385, #97434 ) ) ;
#18319 = CARTESIAN_POINT ( 'NONE',  ( -110.6228709571500985, -24.63287334234179937, 0.9662140553045460711 ) ) ;
#18320 = CARTESIAN_POINT ( 'NONE',  ( -100.6814946224345846, -25.30267106336103922, 4.736250553104468963 ) ) ;
#18321 = DIRECTION ( 'NONE',  ( -1.000000000000000000, -0.000000000000000000, -0.000000000000000000 ) ) ;
#18322 = CARTESIAN_POINT ( 'NONE',  ( -122.5562042904833930, -23.47596703998600631, 11.44779298504227683 ) ) ;
#18323 = CARTESIAN_POINT ( 'NONE',  ( -52.55620429048339304, -24.64898659630528144, 1.056161002820821038 ) ) ;
#18324 = CARTESIAN_POINT ( 'NONE',  ( -96.52287095715006160, -24.65952944569304606, 1.056160979905702346 ) ) ;
#18325 = CARTESIAN_POINT ( 'NONE',  ( 19.65109224456760728, -3.968444974485820786, -1.500000000000002220 ) ) ;
#18326 = CARTESIAN_POINT ( 'NONE',  ( 27.86270917940689174, 0.3587747205144265483, 29.49402280011862487 ) ) ;
#18327 = ORIENTED_EDGE ( 'NONE', *, *, #44409, .T. ) ;
#18328 = CIRCLE ( 'NONE', #96122, 0.8160000000000007248 ) ;
#18330 = CARTESIAN_POINT ( 'NONE',  ( -73.62287095715007013, -24.50321055353806088, 9.387540953477531147 ) ) ;
#18329 = APPROVAL_PERSON_ORGANIZATION ( #94181, #76640, #30794 ) ;
#18331 = LINE ( 'NONE', #42194, #54296 ) ;
#18332 = PLANE ( 'NONE',  #1430 ) ;
#18333 = PLANE ( 'NONE',  #15730 ) ;
#18334 = CARTESIAN_POINT ( 'NONE',  ( -101.7380495759637284, -25.24922313465046386, 3.830795054426443524 ) ) ;
#18335 = DIRECTION ( 'NONE',  ( 0.000000000000000000, -1.000000000000000000, 0.000000000000000000 ) ) ;
#18336 = VECTOR ( 'NONE', #16521, 1000.000000000000000 ) ;
#18337 = EDGE_CURVE ( 'NONE', #534, #99971, #84477, .T. ) ;
#18338 = CARTESIAN_POINT ( 'NONE',  ( -73.62287095715005592, -23.48783264082478084, -1.443836473390067487 ) ) ;
#18339 = ORIENTED_EDGE ( 'NONE', *, *, #23929, .T. ) ;
#18340 = CARTESIAN_POINT ( 'NONE',  ( -18.82647582233506611, 7.659846263794035437, 11.49999999999998934 ) ) ;
#18341 = VECTOR ( 'NONE', #91246, 1000.000000000000000 ) ;
#18342 = ORIENTED_EDGE ( 'NONE', *, *, #53679, .F. ) ;
#18343 = EDGE_CURVE ( 'NONE', #20587, #38439, #14957, .T. ) ;
#18344 = CARTESIAN_POINT ( 'NONE',  ( -32.61958528550577086, -23.48783264082477729, -1.443836473390076147 ) ) ;
#18345 = CARTESIAN_POINT ( 'NONE',  ( -127.5898610374712803, -24.15620529776628800, 10.23563542870658871 ) ) ;
#18346 = ORIENTED_EDGE ( 'NONE', *, *, #47666, .F. ) ;
#18347 = CARTESIAN_POINT ( 'NONE',  ( -59.63756292401139802, -24.15620529776628445, 10.23563542870661180 ) ) ;
#18348 = CARTESIAN_POINT ( 'NONE',  ( -50.28030459868799795, -25.12215419117113768, 7.099251938033546594 ) ) ;
#18349 = CARTESIAN_POINT ( 'NONE',  ( -86.52287095715006160, -23.47593901973090169, -1.443836447538996648 ) ) ;
#18350 = CARTESIAN_POINT ( 'NONE',  ( 18.68757921870947669, -9.911485057863893999, 11.49999999999999645 ) ) ;
#18351 = CARTESIAN_POINT ( 'NONE',  ( 19.07224962250127831, -11.27678277851665634, -1.500000000000002220 ) ) ;
#18353 = CARTESIAN_POINT ( 'NONE',  ( 11.93631617611541351, -16.73449621718459923, -1.500000000000002220 ) ) ;
#18352 = PRODUCT_RELATED_PRODUCT_CATEGORY ( 'detail', '', ( #5326 ) ) ;
#18354 = VERTEX_POINT ( 'NONE', #99680 ) ;
#18355 = CARTESIAN_POINT ( 'NONE',  ( -91.52287095715006160, -23.47596703998600631, 11.44779298504228393 ) ) ;
#18356 = ORIENTED_EDGE ( 'NONE', *, *, #97462, .F. ) ;
#18357 = CARTESIAN_POINT ( 'NONE',  ( -116.6228709571500559, -29.50250243563736774, 8.947779886222134493 ) ) ;
#18358 = DIRECTION ( 'NONE',  ( -3.773278334453079618E-23, 0.9999999999976377785, 2.173523156925979975E-06 ) ) ;
#18359 = VERTEX_POINT ( 'NONE', #46417 ) ;
#18360 = ORIENTED_EDGE ( 'NONE', *, *, #79548, .T. ) ;
#18361 = ORIENTED_EDGE ( 'NONE', *, *, #90534, .T. ) ;
#18362 = CARTESIAN_POINT ( 'NONE',  ( -70.52287095715007581, -23.48786465467241769, 11.44779295918254647 ) ) ;
#18363 = CARTESIAN_POINT ( 'NONE',  ( 7.116579217368891541, -6.376774720514415407, 20.51774267661129869 ) ) ;
#18364 = CARTESIAN_POINT ( 'NONE',  ( -91.62287095715004170, -24.65952944569304606, 1.056160979905700792 ) ) ;
#18365 = CARTESIAN_POINT ( 'NONE',  ( 13.32396043830641830, 15.83023408377254704, -1.500000000000002220 ) ) ;
#18366 = CARTESIAN_POINT ( 'NONE',  ( 15.40532884848888884, -15.22192433072940609, 11.49999999999999645 ) ) ;
#18367 = VERTEX_POINT ( 'NONE', #22555 ) ;
#18368 = CIRCLE ( 'NONE', #15174, 1.250000000000001110 ) ;
#18369 = CARTESIAN_POINT ( 'NONE',  ( -60.52287095715003318, -24.52323809117613607, 9.355190652322249889 ) ) ;
#18370 = DIRECTION ( 'NONE',  ( -1.000000000000000000, 0.000000000000000000, -0.000000000000000000 ) ) ;
#18371 = CARTESIAN_POINT ( 'NONE',  ( -8.193370562272118462, -20.86776251599019361, 11.49999999999998934 ) ) ;
#18372 = DIRECTION ( 'NONE',  ( -1.000000000000000000, -0.000000000000000000, -0.000000000000000000 ) ) ;
#18373 = CARTESIAN_POINT ( 'NONE',  ( -71.62287095715005592, -24.65952944569304606, 1.056160979905699016 ) ) ;
#18374 = EDGE_LOOP ( 'NONE', ( #30323, #71689, #96482, #99079 ) ) ;
#18375 = CARTESIAN_POINT ( 'NONE',  ( -31.62287095715005236, -24.66019654487199020, 8.947790411086138818 ) ) ;
#18376 = CARTESIAN_POINT ( 'NONE',  ( -89.40841769935767047, -25.05712065398430966, 7.447789548358837663 ) ) ;
#18377 = CIRCLE ( 'NONE', #21543, 129.7684398600581233 ) ;
#18378 = VERTEX_POINT ( 'NONE', #91586 ) ;
#18379 = ORIENTED_EDGE ( 'NONE', *, *, #6797, .F. ) ;
#18380 = FACE_OUTER_BOUND ( 'NONE', #14211, .T. ) ;
#18381 = ORIENTED_EDGE ( 'NONE', *, *, #33550, .F. ) ;
#18382 = B_SPLINE_CURVE_WITH_KNOTS ( 'NONE', 3,
 ( #51963, #59084, #90021, #81908, #82892, #12386 ),
 .UNSPECIFIED., .F., .F.,
 ( 4, 2, 4 ),
 ( 1.570887131794638196E-05, 0.001396322306279759555, 0.002776935741241572803 ),
 .UNSPECIFIED. ) ;
#18383 = PLANE ( 'NONE',  #66586 ) ;
#18384 = CARTESIAN_POINT ( 'NONE',  ( -9.361133326760958440, -19.03884994183470880, -1.500000000000002220 ) ) ;
#18385 = EDGE_LOOP ( 'NONE', ( #93843, #77218, #35075, #38856 ) ) ;
#18386 = CARTESIAN_POINT ( 'NONE',  ( -88.55459573829534747, -23.96119346886880308, -0.6495511937832096905 ) ) ;
#18387 = CARTESIAN_POINT ( 'NONE',  ( 11.26692973276593968, -18.67385317477220497, 11.49999999999998934 ) ) ;
#18388 = CARTESIAN_POINT ( 'NONE',  ( -52.53661446490540499, -24.51419770103158413, 9.386484678747187615 ) ) ;
#18389 = CARTESIAN_POINT ( 'NONE',  ( -111.9545715455114987, -29.50249917535260380, 7.447779886225679213 ) ) ;
#18390 = CARTESIAN_POINT ( 'NONE',  ( 5.329826657887789310, -5.876774720514418071, 20.66144943787464783 ) ) ;
#18391 = CARTESIAN_POINT ( 'NONE',  ( -19.96805355746080934, -8.928269573510897672, -1.500000000000002220 ) ) ;
#18392 = CARTESIAN_POINT ( 'NONE',  ( -109.5228709571500616, -23.73934037231757443, 11.05740245334328087 ) ) ;
#18393 = ORIENTED_EDGE ( 'NONE', *, *, #66406, .T. ) ;
#18394 = DIRECTION ( 'NONE',  ( -0.000000000000000000, 1.000000000000000000, -0.000000000000000000 ) ) ;
#18395 = DIRECTION ( 'NONE',  ( 1.000000000000000000, 0.000000000000000000, 0.000000000000000000 ) ) ;
#18396 = ORIENTED_EDGE ( 'NONE', *, *, #50954, .T. ) ;
#18397 = VECTOR ( 'NONE', #50363, 1000.000000000000000 ) ;
#18398 = CARTESIAN_POINT ( 'NONE',  ( -30.61271081598701471, -24.37855497370575009, 0.3021426168933804557 ) ) ;
#18399 = EDGE_LOOP ( 'NONE', ( #70892, #91823, #8261, #96750 ) ) ;
#18400 = EDGE_CURVE ( 'NONE', #48069, #43651, #68760, .T. ) ;
#18401 = LINE ( 'NONE', #49370, #56683 ) ;
#18402 = CARTESIAN_POINT ( 'NONE',  ( -82.55439603937421111, -23.96119346886881019, -0.6495511937831923710 ) ) ;
#18403 = CARTESIAN_POINT ( 'NONE',  ( 1.624102159173431259, 21.17561035156254334, 11.49999999999998934 ) ) ;
#18404 = CARTESIAN_POINT ( 'NONE',  ( 10.46399479596398052, 2.894108053847758821, -27.03001098546561920 ) ) ;
#18405 = ADVANCED_FACE ( 'NONE', ( #76352 ), #63650, .T. ) ;
#18406 = CARTESIAN_POINT ( 'NONE',  ( -30.62200344337180269, -24.13759587396041439, -0.5132947483565731828 ) ) ;
#18407 = CARTESIAN_POINT ( 'NONE',  ( -67.52287095715006160, -29.50250243563736774, 8.947779886222143375 ) ) ;
#18408 = CARTESIAN_POINT ( 'NONE',  ( -68.64584877695018861, -23.73766607897669445, -1.055555164236457788 ) ) ;
#18410 = CARTESIAN_POINT ( 'NONE',  ( 1.664315604108443925, 19.36118569274438528, 11.49999999999998934 ) ) ;
#18409 = AXIS2_PLACEMENT_3D ( 'NONE', #38512, #22267, #29397 ) ;
#18411 = CARTESIAN_POINT ( 'NONE',  ( -45.54237047602679667, -24.40034930558990922, 0.3402023900116019073 ) ) ;
#18412 = EDGE_LOOP ( 'NONE', ( #56330, #77080, #48091, #35086 ) ) ;
#18413 = CARTESIAN_POINT ( 'NONE',  ( 18.23270504744370868, -6.907985942191454676, 11.49999999999999645 ) ) ;
#18414 = CARTESIAN_POINT ( 'NONE',  ( -5.238752036864926964, -5.876774720514408301, 19.51517878119694061 ) ) ;
#18415 = CIRCLE ( 'NONE', #63786, 21.24999999999998579 ) ;
#18416 = CARTESIAN_POINT ( 'NONE',  ( -42.58953762381671737, -23.48786465467240347, 11.44779295918255180 ) ) ;
#18417 = EDGE_CURVE ( 'NONE', #20796, #97996, #90894, .T. ) ;
#18418 = ORIENTED_EDGE ( 'NONE', *, *, #55648, .F. ) ;
#18419 = DIRECTION ( 'NONE',  ( 0.000000000000000000, -0.9999999999976377785, -2.173523156925979128E-06 ) ) ;
#18420 = CARTESIAN_POINT ( 'NONE',  ( -89.54842567568222478, -24.34968618360934300, 0.1864209137778942982 ) ) ;
#18421 = CARTESIAN_POINT ( 'NONE',  ( -80.62287095715007013, -23.47596703998600631, 11.44779298504227860 ) ) ;
#18422 = CARTESIAN_POINT ( 'NONE',  ( -81.88534077628074215, -25.03155785007460565, 6.293943450071303403 ) ) ;
#18423 = CARTESIAN_POINT ( 'NONE',  ( 5.252985061998082017, 18.97096265210048571, 11.49999999999998934 ) ) ;
#18424 = EDGE_LOOP ( 'NONE', ( #75738, #39968, #65614, #9623 ) ) ;
#18425 = B_SPLINE_CURVE_WITH_KNOTS ( 'NONE', 3,
 ( #963, #100394, #8580, #1474 ),
 .UNSPECIFIED., .F., .F.,
 ( 4, 4 ),
 ( 0.000000000000000000, 9.999999999999592548E-05 ),
 .UNSPECIFIED. ) ;
#18426 = DIRECTION ( 'NONE',  ( 3.773278334444166432E-23, -1.000000000000000000, 0.000000000000000000 ) ) ;
#18427 = CARTESIAN_POINT ( 'NONE',  ( 18.33865528945960577, 14.04639130150205872, -1.500000000000002220 ) ) ;
#18428 = PERSON_AND_ORGANIZATION ( #70597, #27821 ) ;
#18429 = ORIENTED_EDGE ( 'NONE', *, *, #42383, .T. ) ;
#18430 = CARTESIAN_POINT ( 'NONE',  ( -93.58414072440028519, -24.65952944569305316, 1.056160979905701458 ) ) ;
#18431 = PLANE ( 'NONE',  #91165 ) ;
#18432 = LINE ( 'NONE', #33151, #84735 ) ;
#18433 = CARTESIAN_POINT ( 'NONE',  ( -105.6228709571500559, -23.85229601348997974, 10.88205029486207565 ) ) ;
#18434 = CARTESIAN_POINT ( 'NONE',  ( -80.91017088437544658, -25.27183487616304447, 3.712349674769177987 ) ) ;
#18435 = CARTESIAN_POINT ( 'NONE',  ( -69.41551097411255000, -25.24515161617911119, 5.862899549986941850 ) ) ;
#18436 = CARTESIAN_POINT ( 'NONE',  ( -50.62287095715007013, -23.84047902841600930, -0.8780736468305810893 ) ) ;
#18437 = CARTESIAN_POINT ( 'NONE',  ( -10.29545327866581950, 17.06371652956568852, 11.49999999999998934 ) ) ;
#18438 = CARTESIAN_POINT ( 'NONE',  ( -75.56672023527714543, -23.48786465467241058, 11.44779295918254824 ) ) ;
#18439 = CARTESIAN_POINT ( 'NONE',  ( 17.36586316225375981, 9.700842922841564686, -1.500000000000002220 ) ) ;
#18440 = ORIENTED_EDGE ( 'NONE', *, *, #1862, .T. ) ;
#18441 = CARTESIAN_POINT ( 'NONE',  ( -122.5228709571500758, -24.33927499327855770, 9.819080762295801179 ) ) ;
#18442 = EDGE_CURVE ( 'NONE', #72919, #45742, #94970, .T. ) ;
#18443 = VECTOR ( 'NONE', #8043, 1000.000000000000114 ) ;
#18444 = DIRECTION ( 'NONE',  ( 0.000000000000000000, -0.000000000000000000, -1.000000000000000000 ) ) ;
#18445 = LINE ( 'NONE', #66150, #36541 ) ;
#18446 = CARTESIAN_POINT ( 'NONE',  ( -80.58144581644191362, -24.92592662359561473, 8.075495903017996469 ) ) ;
#18447 = CARTESIAN_POINT ( 'NONE',  ( 14.74948264216024008, 14.65492983226340407, 11.49999999999999645 ) ) ;
#18448 = DIRECTION ( 'NONE',  ( -1.000000000000000000, 0.000000000000000000, 0.000000000000000000 ) ) ;
#18449 = ADVANCED_FACE ( 'NONE', ( #39799 ), #7473, .T. ) ;
#18450 = CARTESIAN_POINT ( 'NONE',  ( -50.61312830650895478, -25.18704472134033168, 3.308904489557473294 ) ) ;
#18451 = CARTESIAN_POINT ( 'NONE',  ( 16.42120958226126604, -15.83219868413775622, 11.49999999999999645 ) ) ;
#18452 = ORIENTED_EDGE ( 'NONE', *, *, #22090, .T. ) ;
#18453 = FACE_OUTER_BOUND ( 'NONE', #40672, .T. ) ;
#18454 = CARTESIAN_POINT ( 'NONE',  ( -92.52287095715006160, -23.47596703998600631, 11.44779298504228393 ) ) ;
#18455 = ORIENTED_EDGE ( 'NONE', *, *, #19976, .F. ) ;
#18456 = CARTESIAN_POINT ( 'NONE',  ( 18.20877288740043198, -8.745817889818592761, -1.500000000000002220 ) ) ;
#18457 = CARTESIAN_POINT ( 'NONE',  ( -55.52287095715005449, -25.00158670708909270, 2.256160236439166411 ) ) ;
#18458 = PLANE ( 'NONE',  #4802 ) ;
#18459 = CARTESIAN_POINT ( 'NONE',  ( 16.00000000000000000, 0.000000000000000000, 0.000000000000000000 ) ) ;
#18460 = VERTEX_POINT ( 'NONE', #70255 ) ;
#18461 = CARTESIAN_POINT ( 'NONE',  ( -109.5895376238167103, -24.64965694238407679, 8.947790433994649462 ) ) ;
#18462 = CARTESIAN_POINT ( 'NONE',  ( -51.29687923781917647, -25.18439801854641047, 3.993462348633455061 ) ) ;
#18463 = CARTESIAN_POINT ( 'NONE',  ( 2.999408428739025023, -19.78128511538675127, -1.500000000000002220 ) ) ;
#18464 = CARTESIAN_POINT ( 'NONE',  ( 20.88312143257166653, -1.666129412636018214, 11.49999999999999645 ) ) ;
#18465 = CARTESIAN_POINT ( 'NONE',  ( -29.35807781927573501, -25.00935022314251199, 7.267259836917594029 ) ) ;
#18466 = DIRECTION ( 'NONE',  ( 0.000000000000000000, 0.000000000000000000, 1.000000000000000000 ) ) ;
#18467 = CARTESIAN_POINT ( 'NONE',  ( 9.306852550357104903, -20.00191182576189064, 11.49999999999998934 ) ) ;
#18468 = ADVANCED_FACE ( 'NONE', ( #24070 ), #64171, .F. ) ;
#18469 = CC_DESIGN_DATE_AND_TIME_ASSIGNMENT ( #23649, #85054, ( #3602 ) ) ;
#18470 = CARTESIAN_POINT ( 'NONE',  ( -40.20932372006943467, -25.27806103562203077, 5.067940379994220201 ) ) ;
#18471 = VERTEX_POINT ( 'NONE', #39298 ) ;
#18472 = DIRECTION ( 'NONE',  ( -3.773278334453079030E-23, 0.9999999999976377785, 2.173523156925979128E-06 ) ) ;
#18473 = CARTESIAN_POINT ( 'NONE',  ( -118.6228709571500559, -24.64898659630368627, 1.056161002820833028 ) ) ;
#18474 = CARTESIAN_POINT ( 'NONE',  ( -89.62287095715004170, -29.50247984919015209, -1.443849546365051806 ) ) ;
#18475 = VERTEX_POINT ( 'NONE', #25577 ) ;
#18476 = CARTESIAN_POINT ( 'NONE',  ( 2.710830299132254595, -6.376774720514410077, 19.05039662921485544 ) ) ;
#18477 = ORIENTED_EDGE ( 'NONE', *, *, #97862, .T. ) ;
#18478 = B_SPLINE_CURVE_WITH_KNOTS ( 'NONE', 3,
 ( #97566, #20426, #74232, #4727, #6707, #28547, #74717, #52899, #52396, #35677, #59516, #66652, #13814, #20931, #76212, #44293, #12817, #97069 ),
 .UNSPECIFIED., .F., .F.,
 ( 4, 2, 2, 2, 2, 2, 2, 2, 4 ),
 ( 0.004711333090593606242, 0.005300197173489861781, 0.005889061256386118187, 0.006477925339282373726, 0.007066789422178629265, 0.007655653505074885672, 0.008244517587971140343, 0.008833381670867397617, 0.009422245753763653156 ),
 .UNSPECIFIED. ) ;
#18479 = ORIENTED_EDGE ( 'NONE', *, *, #3465, .F. ) ;
#18480 = CARTESIAN_POINT ( 'NONE',  ( 22.81105451610979173, -1.475225279485572916, -19.61691820600746539 ) ) ;
#18481 = CARTESIAN_POINT ( 'NONE',  ( 24.71017632900190719, -5.356774720514427379, 1.647607965253213624 ) ) ;
#18482 = CARTESIAN_POINT ( 'NONE',  ( -51.52287095715007581, -24.33832256527048798, 0.1851278514138590403 ) ) ;
#18483 = CARTESIAN_POINT ( 'NONE',  ( -20.35906544237474236, -2.577633573104691322, -1.500000000000002220 ) ) ;
#18484 = VERTEX_POINT ( 'NONE', #47925 ) ;
#18485 = DIRECTION ( 'NONE',  ( -3.773278334453079618E-23, 0.9999999999976377785, 2.173523156925979975E-06 ) ) ;
#18486 = EDGE_CURVE ( 'NONE', #70518, #80790, #30321, .T. ) ;
#18487 = CARTESIAN_POINT ( 'NONE',  ( 7.166666666666668739, -5.876774720514419847, 20.78665865384614975 ) ) ;
#18488 = CYLINDRICAL_SURFACE ( 'NONE', #4319, 2.349999999999999645 ) ;
#18489 = CARTESIAN_POINT ( 'NONE',  ( 19.83320176327591255, -10.20924650237717835, -1.500000000000002220 ) ) ;
#18490 = CARTESIAN_POINT ( 'NONE',  ( 32.23865423223558935, -4.540774720514431095, 2.161924922174277341 ) ) ;
#18491 = CARTESIAN_POINT ( 'NONE',  ( -124.6228709571500417, -24.51283580621365488, 0.6167428607019822540 ) ) ;
#18492 = ORIENTED_EDGE ( 'NONE', *, *, #78006, .T. ) ;
#18493 = CARTESIAN_POINT ( 'NONE',  ( -43.62287095715004881, -24.65952944569304606, 1.056160979905692576 ) ) ;
#18494 = LINE ( 'NONE', #17998, #52347 ) ;
#18495 = CARTESIAN_POINT ( 'NONE',  ( 7.204507412156021751, -19.57454612608841771, 11.49999999999998934 ) ) ;
#18496 = ORIENTED_EDGE ( 'NONE', *, *, #8216, .F. ) ;
#18498 = EDGE_LOOP ( 'NONE', ( #50860, #5399, #52475, #30917 ) ) ;
#18497 = CARTESIAN_POINT ( 'NONE',  ( 14.73162737928355170, -2.682774720514426559, -27.37940951657878941 ) ) ;
#18499 = ORIENTED_EDGE ( 'NONE', *, *, #80729, .T. ) ;
#18500 = FACE_OUTER_BOUND ( 'NONE', #87251, .T. ) ;
#18501 = CARTESIAN_POINT ( 'NONE',  ( -21.07084664159375009, 0.3847054351051909515, -1.500000000000002220 ) ) ;
#18502 = ORIENTED_EDGE ( 'NONE', *, *, #41309, .F. ) ;
#18503 = DIRECTION ( 'NONE',  ( 0.000000000000000000, 1.084202172485504434E-16, -1.000000000000000000 ) ) ;
#18504 = LINE ( 'NONE', #79900, #38520 ) ;
#18505 = DIRECTION ( 'NONE',  ( 0.000000000000000000, -2.173523156925980399E-06, 0.9999999999976378895 ) ) ;
#18506 = CARTESIAN_POINT ( 'NONE',  ( -86.50455038639833560, -24.51419770103155926, 9.386484678747184063 ) ) ;
#18507 = CARTESIAN_POINT ( 'NONE',  ( -59.59827915153204714, -23.96119346886879597, -0.6495511937832131322 ) ) ;
#18508 = CARTESIAN_POINT ( 'NONE',  ( -6.179238894844691465, -20.81818906610659425, -1.500000000000002220 ) ) ;
#18509 = CARTESIAN_POINT ( 'NONE',  ( 5.184553252003285984, 5.965225279485572685, -28.06387035751381731 ) ) ;
#18510 = EDGE_CURVE ( 'NONE', #9237, #31838, #43638, .T. ) ;
#18512 = VERTEX_POINT ( 'NONE', #56550 ) ;
#18511 = CARTESIAN_POINT ( 'NONE',  ( -8.951960448472247478, 20.35530821588910300, 11.49999999999999645 ) ) ;
#18513 = CARTESIAN_POINT ( 'NONE',  ( -50.49683564601712504, -25.31441722724132504, 5.199897239935473259 ) ) ;
#18514 = DIRECTION ( 'NONE',  ( 0.000000000000000000, 0.000000000000000000, 1.000000000000000000 ) ) ;
#18515 = CARTESIAN_POINT ( 'NONE',  ( -87.52287095715004739, -24.51283580621451108, 0.6167428607045201128 ) ) ;
#18516 = VERTEX_POINT ( 'NONE', #56046 ) ;
#18517 = VECTOR ( 'NONE', #67039, 1000.000000000000000 ) ;
#18519 = ORIENTED_EDGE ( 'NONE', *, *, #50598, .F. ) ;
#18518 = CARTESIAN_POINT ( 'NONE',  ( -5.941268476065055815, -6.376774720514417183, 20.11414146978959749 ) ) ;
#18520 = VECTOR ( 'NONE', #85353, 1000.000000000000000 ) ;
#18521 = VERTEX_POINT ( 'NONE', #63156 ) ;
#18522 = CARTESIAN_POINT ( 'NONE',  ( 30.46555845599590029, -5.356774720514427379, 2.040766579062852415 ) ) ;
#18523 = ADVANCED_FACE ( 'NONE', ( #24567 ), #40309, .F. ) ;
#18524 = CARTESIAN_POINT ( 'NONE',  ( -35.52287095715008292, -24.82558206586143257, 1.605769216559448820 ) ) ;
#18525 = CARTESIAN_POINT ( 'NONE',  ( -105.5228709571501469, -24.63287334234180648, 0.9662140553045298619 ) ) ;
#18526 = EDGE_LOOP ( 'NONE', ( #98368, #47726, #80169, #56781 ) ) ;
#18527 = CARTESIAN_POINT ( 'NONE',  ( -130.5728709571500872, -25.35233180439156797, 6.153150975227889674 ) ) ;
#18528 = CARTESIAN_POINT ( 'NONE',  ( -21.65924713590726469, 5.634197536097032888, -1.500000000000002220 ) ) ;
#18529 = EDGE_CURVE ( 'NONE', #19170, #10252, #65410, .T. ) ;
#18530 = ORIENTED_EDGE ( 'NONE', *, *, #10647, .T. ) ;
#18531 = CARTESIAN_POINT ( 'NONE',  ( -87.52287095715006160, -29.50248528299804818, 1.056150453629040253 ) ) ;
#18532 = DIRECTION ( 'NONE',  ( 0.000000000000000000, -2.173523156925980399E-06, 0.9999999999976378895 ) ) ;
#18533 = CARTESIAN_POINT ( 'NONE',  ( -44.62287095715004881, -23.48786465467240347, 11.44779295918255180 ) ) ;
#18534 = DIRECTION ( 'NONE',  ( -3.773278334453079030E-23, 0.9999999999976377785, 2.173523156925979128E-06 ) ) ;
#18535 = EDGE_CURVE ( 'NONE', #84685, #50583, #80427, .T. ) ;
#18536 = B_SPLINE_CURVE_WITH_KNOTS ( 'NONE', 3,
 ( #47816, #10248, #78738, #9239, #33589, #40201 ),
 .UNSPECIFIED., .F., .F.,
 ( 4, 2, 4 ),
 ( 1.570887131794952276E-05, 0.001396322306279762157, 0.002776935741241574537 ),
 .UNSPECIFIED. ) ;
#18537 = B_SPLINE_CURVE_WITH_KNOTS ( 'NONE', 3,
 ( #14438, #98177, #99659, #45410 ),
 .UNSPECIFIED., .F., .F.,
 ( 4, 4 ),
 ( 0.000000000000000000, 1.000000000000000000 ),
 .UNSPECIFIED. ) ;
#18538 = CARTESIAN_POINT ( 'NONE',  ( -63.93036092109726098, -24.37907397113049868, 9.703205396196695531 ) ) ;
#18539 = CARTESIAN_POINT ( 'NONE',  ( 17.63768857353127828, -8.544740250177758512, -1.500000000000002220 ) ) ;
#18540 = CARTESIAN_POINT ( 'NONE',  ( -50.28106314917847897, -25.31259380064802400, 4.732491477755599085 ) ) ;
#18541 = VERTEX_POINT ( 'NONE', #48427 ) ;
#18542 = AXIS2_PLACEMENT_3D ( 'NONE', #29968, #60937, #91868 ) ;
#18543 = CARTESIAN_POINT ( 'NONE',  ( -21.28347836979250118, 3.227085873532868021, -1.500000000000002220 ) ) ;
#18544 = FACE_OUTER_BOUND ( 'NONE', #82706, .T. ) ;
#18545 = CARTESIAN_POINT ( 'NONE',  ( -81.42380231474228935, -25.30394809369661857, 5.197789011868366060 ) ) ;
#18546 = CARTESIAN_POINT ( 'NONE',  ( -113.5228709571501327, -24.66019654487200441, 8.947790411086112172 ) ) ;
#18547 = DIRECTION ( 'NONE',  ( 0.000000000000000000, -1.000000000000000000, 0.000000000000000000 ) ) ;
#18548 = CARTESIAN_POINT ( 'NONE',  ( -12.73177969873712279, -19.06072230859735939, -1.500000000000002220 ) ) ;
#18549 = CALENDAR_DATE ( 2026, 9, 10 ) ;
#18550 = CARTESIAN_POINT ( 'NONE',  ( -31.52287095715006160, -24.66019654487198665, 8.947790411086131712 ) ) ;
#18551 = DIRECTION ( 'NONE',  ( -3.773278334444166432E-23, 1.000000000000000000, 0.000000000000000000 ) ) ;
#18552 = CARTESIAN_POINT ( 'NONE',  ( 11.77038589110637901, 16.27938679534767275, 11.49999999999999645 ) ) ;
#18553 = CARTESIAN_POINT ( 'NONE',  ( -110.3139465455115129, -25.10927396271619116, 2.832404819606896496 ) ) ;
#18554 = DIRECTION ( 'NONE',  ( -0.000000000000000000, 1.000000000000000000, -0.000000000000000000 ) ) ;
#18555 = CARTESIAN_POINT ( 'NONE',  ( -121.6228709571500417, -23.72773821059535848, 11.05748984161097503 ) ) ;
#18556 = CARTESIAN_POINT ( 'NONE',  ( 14.10331789289311111, 5.152774720514426754, -26.41276880514442738 ) ) ;
#18557 = CARTESIAN_POINT ( 'NONE',  ( 15.10352928271630724, 2.682774720514426559, -27.29968155418892195 ) ) ;
#18558 = CARTESIAN_POINT ( 'NONE',  ( -17.59554656748941071, 9.132484154288260214, 11.49999999999998934 ) ) ;
#18559 = LINE ( 'NONE', #49533, #80420 ) ;
#18560 = CARTESIAN_POINT ( 'NONE',  ( 18.75866648459458830, -6.009157199652424453, -1.500000000000002220 ) ) ;
#18561 = CARTESIAN_POINT ( 'NONE',  ( 30.93860345374796594, -0.6647747205144267646, 23.11160796525322070 ) ) ;
#18562 = PERSON_AND_ORGANIZATION ( #25850, #52372 ) ;
#18563 = CARTESIAN_POINT ( 'NONE',  ( -57.52287095715005449, -24.50321055353803956, 9.387540953477520489 ) ) ;
#18564 = CARTESIAN_POINT ( 'NONE',  ( 5.202077965628057576, -2.038091937962834166, -2.869745073849994963E-16 ) ) ;
#18565 = CARTESIAN_POINT ( 'NONE',  ( -13.12974562303265813, -15.89414520977026513, 11.49999999999999645 ) ) ;
#18566 = AXIS2_PLACEMENT_3D ( 'NONE', #38046, #54293, #29931 ) ;
#18567 = DIRECTION ( 'NONE',  ( -0.000000000000000000, 1.000000000000000000, -0.000000000000000000 ) ) ;
#18569 = ADVANCED_FACE ( 'NONE', ( #71763 ), #9849, .F. ) ;
#18568 = CARTESIAN_POINT ( 'NONE',  ( 4.697487806458584991, -22.17256498326293013, 11.49999999999999645 ) ) ;
#18570 = ORIENTED_EDGE ( 'NONE', *, *, #24774, .T. ) ;
#18571 = DIRECTION ( 'NONE',  ( -1.000000000000000000, -3.773278334444166432E-23, -8.201307841325785021E-29 ) ) ;
#18572 = CARTESIAN_POINT ( 'NONE',  ( -97.51358978418939216, -24.15543982623907837, -0.2315651400026600415 ) ) ;
#18573 = B_SPLINE_CURVE_WITH_KNOTS ( 'NONE', 3,
 ( #55632, #56636, #87062, #50021 ),
 .UNSPECIFIED., .F., .F.,
 ( 4, 4 ),
 ( 0.000000000000000000, 1.000000000000000000 ),
 .UNSPECIFIED. ) ;
#18574 = CARTESIAN_POINT ( 'NONE',  ( -110.6228709571500417, -24.14406661707770141, 10.28769366152062226 ) ) ;
#18575 = CARTESIAN_POINT ( 'NONE',  ( -93.52287095715006160, -24.64965694238407323, 8.947790433994196491 ) ) ;
#18576 = ORIENTED_EDGE ( 'NONE', *, *, #30402, .T. ) ;
#18577 = CARTESIAN_POINT ( 'NONE',  ( 3.535601659403828201, -22.84449096179584160, 11.49999999999999645 ) ) ;
#18578 = CARTESIAN_POINT ( 'NONE',  ( -21.78311099772515647, -6.823855485095160489, 11.49999999999998934 ) ) ;
#18579 = PLANE ( 'NONE',  #82720 ) ;
#18580 = CARTESIAN_POINT ( 'NONE',  ( -63.62365448271125956, -24.66019654487200086, 8.947790411086121054 ) ) ;
#18581 = CARTESIAN_POINT ( 'NONE',  ( 8.356338879324495039, -20.90460381316865934, 11.49999999999999645 ) ) ;
#18582 = ORIENTED_EDGE ( 'NONE', *, *, #91461, .T. ) ;
#18583 = CARTESIAN_POINT ( 'NONE',  ( 30.09341516180546350, -4.772774720514425972, -11.39311774897855933 ) ) ;
#18584 = CARTESIAN_POINT ( 'NONE',  ( -19.92591009635028243, 9.278653061003369729, 11.49999999999998934 ) ) ;
#18585 = CARTESIAN_POINT ( 'NONE',  ( -118.5228709571500758, -23.47596703998600631, 11.44779298504227860 ) ) ;
#18586 = ADVANCED_FACE ( 'NONE', ( #76182 ), #30013, .F. ) ;
#18587 = CARTESIAN_POINT ( 'NONE',  ( -111.5187080011053240, -23.96119346886881019, -0.6495511937832035843 ) ) ;
#18588 = DIRECTION ( 'NONE',  ( -3.773278334453079618E-23, 0.9999999999976377785, 2.173523156925979975E-06 ) ) ;
#18589 = ORIENTED_EDGE ( 'NONE', *, *, #12075, .F. ) ;
#18590 = CARTESIAN_POINT ( 'NONE',  ( -48.50069532262279637, -24.15620529776628089, 10.23563542870660470 ) ) ;
#18591 = CARTESIAN_POINT ( 'NONE',  ( -52.52287095715006870, -29.50248528299804818, 1.056150453629033370 ) ) ;
#18592 = ORIENTED_EDGE ( 'NONE', *, *, #14290, .F. ) ;
#18593 = EDGE_CURVE ( 'NONE', #45083, #21005, #38765, .T. ) ;
#18594 = CARTESIAN_POINT ( 'NONE',  ( -54.58254524432665278, -24.51419770103157347, 9.386484678747176957 ) ) ;
#18595 = CARTESIAN_POINT ( 'NONE',  ( 15.48611046165106941, -13.43736321338083783, 11.49999999999998934 ) ) ;
#18596 = ORIENTED_EDGE ( 'NONE', *, *, #73131, .T. ) ;
#18597 = EDGE_LOOP ( 'NONE', ( #54419, #46195, #78345, #38722 ) ) ;
#18598 = ORIENTED_EDGE ( 'NONE', *, *, #43165, .T. ) ;
#18599 = CARTESIAN_POINT ( 'NONE',  ( -49.85569807066763559, -25.31193038000811057, 5.303933706555637784 ) ) ;
#18600 = CARTESIAN_POINT ( 'NONE',  ( 22.67273400128462058, 4.441195646929153362, 11.49999999999998934 ) ) ;
#18601 = CARTESIAN_POINT ( 'NONE',  ( -104.5531557358278008, -24.15620529776629155, 10.23563542870659759 ) ) ;
#18602 = CARTESIAN_POINT ( 'NONE',  ( 19.78452974690265975, -4.759501717958375622, -1.500000000000002220 ) ) ;
#18603 = ORIENTED_EDGE ( 'NONE', *, *, #8212, .F. ) ;
#18604 = FACE_OUTER_BOUND ( 'NONE', #35058, .T. ) ;
#18605 = EDGE_CURVE ( 'NONE', #45470, #68982, #56942, .T. ) ;
#18606 = CARTESIAN_POINT ( 'NONE',  ( -51.40142156539464935, -25.18959696641875112, 3.254916540799400515 ) ) ;
#18607 = EDGE_CURVE ( 'NONE', #42749, #14525, #21888, .T. ) ;
#18608 = CARTESIAN_POINT ( 'NONE',  ( -105.5461413990837940, -25.00158670708910691, 2.256160236439218369 ) ) ;
#18609 = CARTESIAN_POINT ( 'NONE',  ( -70.34543693012690824, -25.25855381946792377, 7.563173725924075441 ) ) ;
#18610 = VERTEX_POINT ( 'NONE', #37134 ) ;
#18611 = CARTESIAN_POINT ( 'NONE',  ( -28.88251580808842789, -25.21531814767515556, 2.994893284986237081 ) ) ;
#18612 = CARTESIAN_POINT ( 'NONE',  ( -49.46456330771200527, -25.31573792550670277, 4.758318069380484516 ) ) ;
#18613 = ADVANCED_FACE ( 'NONE', ( #61984 ), #23387, .F. ) ;
#18614 = VECTOR ( 'NONE', #45404, 1000.000000000000114 ) ;
#18615 = EDGE_LOOP ( 'NONE', ( #44390, #13695, #2491, #33466 ) ) ;
#18616 = CARTESIAN_POINT ( 'NONE',  ( -8.830788454959730416, 18.81286502489961876, -1.500000000000002220 ) ) ;
#18617 = ORIENTED_EDGE ( 'NONE', *, *, #45900, .F. ) ;
#18619 = ORIENTED_EDGE ( 'NONE', *, *, #85580, .T. ) ;
#18618 = CARTESIAN_POINT ( 'NONE',  ( -125.6238070234729491, -24.83618233451450763, 1.606449574219537046 ) ) ;
#18620 = CARTESIAN_POINT ( 'NONE',  ( -82.55620429048337883, -24.64898659630528854, 1.056161002820828143 ) ) ;
#18621 = CARTESIAN_POINT ( 'NONE',  ( -102.6228709571500559, -24.64898659630368272, 1.056161002820829697 ) ) ;
#18622 = ORIENTED_EDGE ( 'NONE', *, *, #50945, .F. ) ;
#18623 = ORIENTED_EDGE ( 'NONE', *, *, #73694, .T. ) ;
#18624 = CARTESIAN_POINT ( 'NONE',  ( 3.300000000000006040, 0.000000000000000000, 0.000000000000000000 ) ) ;
#18625 = FACE_OUTER_BOUND ( 'NONE', #1545, .T. ) ;
#18626 = CARTESIAN_POINT ( 'NONE',  ( -43.57657991008606757, -24.66019654487199375, 8.947790411086121054 ) ) ;
#18627 = EDGE_CURVE ( 'NONE', #85108, #85219, #85303, .T. ) ;
#18629 = VERTEX_POINT ( 'NONE', #85814 ) ;
#18628 = CARTESIAN_POINT ( 'NONE',  ( 10.81757466760856801, -19.22619917341675588, 11.49999999999999645 ) ) ;
#18630 = CARTESIAN_POINT ( 'NONE',  ( -48.87380231474225667, -25.26256937810135028, 6.137091986423513390 ) ) ;
#18631 = CARTESIAN_POINT ( 'NONE',  ( -18.09186581907994196, -13.49991075323410250, 11.49999999999998934 ) ) ;
#18633 = ORIENTED_EDGE ( 'NONE', *, *, #45769, .F. ) ;
#18632 = PLANE ( 'NONE',  #99237 ) ;
#18634 = ORIENTED_EDGE ( 'NONE', *, *, #34263, .T. ) ;
#18635 = CARTESIAN_POINT ( 'NONE',  ( 1.876957540558651605, -5.558144974487054135, 0.000000000000000000 ) ) ;
#18636 = AXIS2_PLACEMENT_3D ( 'NONE', #56803, #80613, #95839 ) ;
#18637 = EDGE_CURVE ( 'NONE', #96235, #7232, #32655, .T. ) ;
#18638 = EDGE_CURVE ( 'NONE', #79877, #2526, #16833, .T. ) ;
#18639 = LINE ( 'NONE', #32881, #323 ) ;
#18640 = ORIENTED_EDGE ( 'NONE', *, *, #38482, .F. ) ;
#18641 = CARTESIAN_POINT ( 'NONE',  ( -20.81765089029956783, 3.879123387127271005, -1.500000000000002220 ) ) ;
#18642 = CARTESIAN_POINT ( 'NONE',  ( -78.94558681842012504, -25.27791652114184373, 6.087055360511715030 ) ) ;
#18643 = CARTESIAN_POINT ( 'NONE',  ( -7.326845193947049140, -5.876774720514417183, 20.33046051580616265 ) ) ;
#18644 = DIRECTION ( 'NONE',  ( 0.000000000000000000, 0.000000000000000000, -1.000000000000000000 ) ) ;
#18645 = CARTESIAN_POINT ( 'NONE',  ( -22.15176777451872425, 1.842445310382735624, -1.500000000000002220 ) ) ;
#18646 = CARTESIAN_POINT ( 'NONE',  ( -114.6244202119018922, -24.51314013834316086, 0.6176544820404237246 ) ) ;
#18647 = EDGE_CURVE ( 'NONE', #62723, #95252, #51304, .T. ) ;
#18648 = VECTOR ( 'NONE', #34715, 1000.000000000000114 ) ;
#18649 = ORIENTED_EDGE ( 'NONE', *, *, #72695, .T. ) ;
#18650 = CARTESIAN_POINT ( 'NONE',  ( 5.271800844830267785, -3.316774720514427344, -28.56638892017480913 ) ) ;
#18651 = CARTESIAN_POINT ( 'NONE',  ( -104.6228709571500559, -23.47593901973091235, -1.443836447539001089 ) ) ;
#18652 = VECTOR ( 'NONE', #35707, 1000.000000000000114 ) ;
#18653 = EDGE_CURVE ( 'NONE', #71190, #57577, #64140, .T. ) ;
#18654 = CARTESIAN_POINT ( 'NONE',  ( -36.63501922174244640, -24.35071581493542325, 9.817618358456030592 ) ) ;
#18655 = CARTESIAN_POINT ( 'NONE',  ( -40.45829750704998418, -25.18492896333868103, 3.293943116708551777 ) ) ;
#18656 = EDGE_CURVE ( 'NONE', #41839, #40469, #15286, .T. ) ;
#18657 = CARTESIAN_POINT ( 'NONE',  ( -7.007757480239389380, 18.17491015770016816, 11.49999999999998934 ) ) ;
#18658 = CARTESIAN_POINT ( 'NONE',  ( -4.378498130703003532, 20.98420022172975763, 11.49999999999998934 ) ) ;
#18659 = CARTESIAN_POINT ( 'NONE',  ( -1.174900045708346497, -6.376774720514413630, 19.48569229636960998 ) ) ;
#18660 = DIRECTION ( 'NONE',  ( -0.9890158633619159367, -0.1478094111296165969, 0.000000000000000000 ) ) ;
#18661 = CARTESIAN_POINT ( 'NONE',  ( 5.395440699609677537, -5.965225279485594001, -28.51842087987364138 ) ) ;
#18662 = CARTESIAN_POINT ( 'NONE',  ( 7.803535043518188274, -21.38454823780343617, -1.500000000000002220 ) ) ;
#18663 = PERSON ( 'NAUO-PER8', 'UNSPECIFIED', 'UNSPECIFIED', ('UNSPECIFIED'), ('UNSPECIFIED'), ('UNSPECIFIED') ) ;
#18664 = EDGE_CURVE ( 'NONE', #61038, #32532, #570, .T. ) ;
#18665 = DIRECTION ( 'NONE',  ( 0.000000000000000000, 0.000000000000000000, 1.000000000000000000 ) ) ;
#18666 = CARTESIAN_POINT ( 'NONE',  ( -102.5982546441761940, -23.48783264082478439, -1.443836473390064601 ) ) ;
#18667 = DIRECTION ( 'NONE',  ( -3.773278334453079030E-23, 0.9999999999976377785, 2.173523156925979128E-06 ) ) ;
#18668 = CARTESIAN_POINT ( 'NONE',  ( -4.359361796094493258, -19.42695174060331809, 11.49999999999999645 ) ) ;
#18669 = CARTESIAN_POINT ( 'NONE',  ( -104.5173987185542899, -23.96119346886880663, -0.6495511937832033622 ) ) ;
#18670 = CARTESIAN_POINT ( 'NONE',  ( -48.62287095715004881, -29.50250243563736774, 8.947779886222146928 ) ) ;
#18671 = CARTESIAN_POINT ( 'NONE',  ( -48.63355419739910701, -24.34968618360933590, 0.1864209137778884418 ) ) ;
#18672 = ORIENTED_EDGE ( 'NONE', *, *, #99154, .F. ) ;
#18673 = CARTESIAN_POINT ( 'NONE',  ( 15.58962545129235799, 6.475225279485573360, -26.91365498785467025 ) ) ;
#18674 = CARTESIAN_POINT ( 'NONE',  ( -31.81565132553424746, -25.16370864782812689, 7.203858152271859439 ) ) ;
#18675 = CARTESIAN_POINT ( 'NONE',  ( 19.26462925850498920, -9.998780574493274287, 11.49999999999998934 ) ) ;
#18676 = DIRECTION ( 'NONE',  ( -0.000000000000000000, 2.173523156925979552E-06, -0.9999999999976378895 ) ) ;
#18677 = CARTESIAN_POINT ( 'NONE',  ( 14.28107258077893604, -13.35224110012613963, -1.500000000000002220 ) ) ;
#18678 = DIRECTION ( 'NONE',  ( 0.000000000000000000, 0.000000000000000000, -1.000000000000000000 ) ) ;
#18679 = VERTEX_POINT ( 'NONE', #16797 ) ;
#18680 = VECTOR ( 'NONE', #29532, 1000.000000000000000 ) ;
#18681 = CARTESIAN_POINT ( 'NONE',  ( 25.61870917940689196, -5.965225279485572685, 29.49402280011862487 ) ) ;
#18682 = CARTESIAN_POINT ( 'NONE',  ( -8.751980504941329286, -18.49744413911281882, 11.49999999999999645 ) ) ;
#18683 = CARTESIAN_POINT ( 'NONE',  ( -49.62287095715004170, -23.47596703998600631, 11.44779298504227505 ) ) ;
#18684 = CARTESIAN_POINT ( 'NONE',  ( -9.278253834636473130, -5.876774720514426953, 21.78128695274316229 ) ) ;
#18685 = ORIENTED_EDGE ( 'NONE', *, *, #3861, .T. ) ;
#18686 = CARTESIAN_POINT ( 'NONE',  ( -62.62287095715003460, -24.51283580621364067, 0.6167428607019811437 ) ) ;
#18687 = DIRECTION ( 'NONE',  ( -0.3133898629642186684, -4.164321980682960499E-15, 0.9496245541219267006 ) ) ;
#18688 = CARTESIAN_POINT ( 'NONE',  ( 9.402885806365684829, -5.965225279485572685, 29.04108526060719342 ) ) ;
#18689 = B_SPLINE_CURVE_WITH_KNOTS ( 'NONE', 3,
 ( #27198, #42930, #57164, #3870 ),
 .UNSPECIFIED., .F., .F.,
 ( 4, 4 ),
 ( 2.775557561562891351E-17, 0.0001000000000000167286 ),
 .UNSPECIFIED. ) ;
#18690 = CARTESIAN_POINT ( 'NONE',  ( -63.55620429048340725, -23.47596703998600276, 11.44779298504227505 ) ) ;
#18691 = ORIENTED_EDGE ( 'NONE', *, *, #83801, .F. ) ;
#18692 = DIRECTION ( 'NONE',  ( 1.000000000000000000, 0.000000000000000000, 0.000000000000000000 ) ) ;
#18693 = CARTESIAN_POINT ( 'NONE',  ( -22.88579126497628025, -1.409509213828211927, 11.49999999999999645 ) ) ;
#18694 = CARTESIAN_POINT ( 'NONE',  ( 21.15473741701296362, -8.388382055385795510, 11.49999999999998934 ) ) ;
#18695 = CARTESIAN_POINT ( 'NONE',  ( 3.797776442307698286, -6.376774720514427841, 21.83974358974358410 ) ) ;
#18696 = DIRECTION ( 'NONE',  ( 0.000000000000000000, 0.000000000000000000, -1.000000000000000000 ) ) ;
#18697 = CARTESIAN_POINT ( 'NONE',  ( -90.62932173586635543, -24.63355581998384380, 0.9682620441943978751 ) ) ;
#18698 = CARTESIAN_POINT ( 'NONE',  ( -25.92875734969025814, 6.376774720514426953, 30.51402280011862089 ) ) ;
#18699 = CARTESIAN_POINT ( 'NONE',  ( -70.19980647797044071, -25.13395880908142388, 7.096976381558549818 ) ) ;
#18700 = AXIS2_PLACEMENT_3D ( 'NONE', #30440, #76597, #998 ) ;
#18701 = CARTESIAN_POINT ( 'NONE',  ( -12.54888962926113827, 17.92887824059606672, 11.49999999999998934 ) ) ;
#18702 = CARTESIAN_POINT ( 'NONE',  ( -70.58953762381672448, -24.99132157543083821, 2.256160258750496084 ) ) ;
#18703 = VECTOR ( 'NONE', #69886, 1000.000000000000000 ) ;
#18704 = EDGE_CURVE ( 'NONE', #4364, #16838, #55885, .T. ) ;
#18705 = CARTESIAN_POINT ( 'NONE',  ( -26.31489179039940041, -24.86888853887588979, 3.386445682341310270 ) ) ;
#18706 = DIRECTION ( 'NONE',  ( -1.000000000000000000, -3.773278334444165844E-23, -8.201307836089272790E-29 ) ) ;
#18707 = CARTESIAN_POINT ( 'NONE',  ( -58.58294017270318221, -24.51314013834315020, 0.6176544820404091807 ) ) ;
#18708 = ORIENTED_EDGE ( 'NONE', *, *, #2634, .F. ) ;
#18709 = ADVANCED_FACE ( 'NONE', ( #10696 ), #92624, .T. ) ;
#18710 = CARTESIAN_POINT ( 'NONE',  ( -19.37329759448073574, 6.469241145865432863, -1.500000000000002220 ) ) ;
#18711 = ORIENTED_EDGE ( 'NONE', *, *, #63550, .T. ) ;
#18712 = AXIS2_PLACEMENT_3D ( 'NONE', #21011, #59103, #43867 ) ;
#18713 = ORIENTED_EDGE ( 'NONE', *, *, #61732, .F. ) ;
#18714 = B_SPLINE_CURVE_WITH_KNOTS ( 'NONE', 3,
 ( #53429, #85355, #84357, #14841, #38177, #69137, #15839, #100059, #62535, #39183, #70139, #30574, #77229, #31067, #93463 ),
 .UNSPECIFIED., .F., .F.,
 ( 4, 1, 1, 1, 1, 1, 1, 1, 1, 1, 1, 1, 4 ),
 ( 0.000000000000000000, 0.07176606415833990116, 0.1412255357663689537, 0.2091158524974625343, 0.2748396534685271231, 0.3394829303752209260, 0.4024762667353996570, 0.4649418891713271162, 0.5268326406463837985, 0.6474148160608227398, 0.7655615117859490004, 0.8816150870393316685, 1.000000000000000000 ),
 .UNSPECIFIED. ) ;
#18715 = CARTESIAN_POINT ( 'NONE',  ( 22.99805582222048272, -0.5679727363130141482, 11.49999999999998934 ) ) ;
#18716 = CARTESIAN_POINT ( 'NONE',  ( 14.83405752585509596, -4.881907540129173384, -27.54622755360215791 ) ) ;
#18717 = CIRCLE ( 'NONE', #70517, 1.000000000000000000 ) ;
#18718 = ADVANCED_FACE ( 'NONE', ( #25914 ), #94422, .T. ) ;
#18719 = VERTEX_POINT ( 'NONE', #1081 ) ;
#18720 = CARTESIAN_POINT ( 'NONE',  ( -97.62287095715004170, -24.65952944569304606, 1.056160979905701236 ) ) ;
#18721 = EDGE_CURVE ( 'NONE', #12730, #80701, #18306, .T. ) ;
#18722 = CARTESIAN_POINT ( 'NONE',  ( 6.482918536709166624, 0.6683258531633530231, 18.35000000000000142 ) ) ;
#18723 = AXIS2_PLACEMENT_3D ( 'NONE', #58923, #12725, #83246 ) ;
#18724 = EDGE_CURVE ( 'NONE', #45794, #82268, #13994, .T. ) ;
#18725 = CARTESIAN_POINT ( 'NONE',  ( -98.62287095715012697, -24.35013146730204525, 9.818937971375108376 ) ) ;
#18726 = CARTESIAN_POINT ( 'NONE',  ( -99.62727544345402464, -24.35071581493543391, 9.817618358456025263 ) ) ;
#18728 = VERTEX_POINT ( 'NONE', #2592 ) ;
#18727 = CARTESIAN_POINT ( 'NONE',  ( -9.778911232092227124, -18.99720643767551209, 11.49999999999999645 ) ) ;
#18729 = EDGE_CURVE ( 'NONE', #51651, #65785, #26557, .T. ) ;
#18730 = ORIENTED_EDGE ( 'NONE', *, *, #20439, .F. ) ;
#18731 = CARTESIAN_POINT ( 'NONE',  ( 19.02167141253037030, -11.55642654327076535, -1.500000000000002220 ) ) ;
#18732 = CARTESIAN_POINT ( 'NONE',  ( 18.97174343470660318, 8.267356841975738391, -1.500000000000002220 ) ) ;
#18733 = ORIENTED_EDGE ( 'NONE', *, *, #45364, .T. ) ;
#18734 = DIRECTION ( 'NONE',  ( 0.000000000000000000, 1.000000000000000000, 0.000000000000000000 ) ) ;
#18735 = CARTESIAN_POINT ( 'NONE',  ( 3.450324536843889067, -5.876774720514404748, 18.60429515659643229 ) ) ;
#18736 = VERTEX_POINT ( 'NONE', #71601 ) ;
#18737 = CARTESIAN_POINT ( 'NONE',  ( -56.52287095715007581, -24.50216790748205398, 0.6166512839542495072 ) ) ;
#18738 = VERTEX_POINT ( 'NONE', #33032 ) ;
#18739 = CARTESIAN_POINT ( 'NONE',  ( 7.805843057017202824, 6.475225279485576024, -27.15467198446602026 ) ) ;
#18740 = CARTESIAN_POINT ( 'NONE',  ( 7.117523389609132778, 19.69228268689324324, -1.500000000000002220 ) ) ;
#18741 = EDGE_CURVE ( 'NONE', #14881, #60701, #63502, .T. ) ;
#18742 = CARTESIAN_POINT ( 'NONE',  ( -18.33957545910867282, 11.93505917737106259, 11.49999999999999645 ) ) ;
#18743 = DIRECTION ( 'NONE',  ( 3.773278334444166432E-23, -1.000000000000000000, 0.000000000000000000 ) ) ;
#18744 = CARTESIAN_POINT ( 'NONE',  ( 12.95044643391442030, 18.39415735498938176, -1.500000000000002220 ) ) ;
#18745 = CARTESIAN_POINT ( 'NONE',  ( 17.09260067683297635, -12.12037977771017871, 11.49999999999998934 ) ) ;
#18746 = CARTESIAN_POINT ( 'NONE',  ( -38.50505405450132201, -23.96119346886880663, -0.6495511937831989213 ) ) ;
#18747 = CARTESIAN_POINT ( 'NONE',  ( -0.02075734969026423599, 0.3587747205144213303, -0.08597719988137648983 ) ) ;
#18748 = CARTESIAN_POINT ( 'NONE',  ( -89.52287095715006160, -23.47593901973090169, -1.443836447538996426 ) ) ;
#18750 = VERTEX_POINT ( 'NONE', #78677 ) ;
#18749 = EDGE_CURVE ( 'NONE', #37181, #45653, #36752, .T. ) ;
#18751 = VECTOR ( 'NONE', #60529, 1000.000000000000000 ) ;
#18752 = ORIENTED_EDGE ( 'NONE', *, *, #45221, .T. ) ;
#18753 = ORIENTED_EDGE ( 'NONE', *, *, #96329, .F. ) ;
#18754 = LINE ( 'NONE', #63971, #85524 ) ;
#18755 = ORIENTED_EDGE ( 'NONE', *, *, #38478, .T. ) ;
#18756 = EDGE_CURVE ( 'NONE', #91151, #58098, #38337, .T. ) ;
#18757 = CARTESIAN_POINT ( 'NONE',  ( 8.370372042246325250, 19.68514866842044242, -1.500000000000002220 ) ) ;
#18758 = ORIENTED_EDGE ( 'NONE', *, *, #25024, .F. ) ;
#18759 = CARTESIAN_POINT ( 'NONE',  ( 0.3627416911114360598, -5.876774720514411854, 19.59793130852656873 ) ) ;
#18760 = CARTESIAN_POINT ( 'NONE',  ( 5.994809752082427501, 20.21905721239408393, -1.500000000000002220 ) ) ;
#18761 = CARTESIAN_POINT ( 'NONE',  ( -73.52287095715007581, -29.50247984919015209, -1.443849546365055359 ) ) ;
#18762 = DIRECTION ( 'NONE',  ( 0.000000000000000000, -2.173523156925980399E-06, 0.9999999999976378895 ) ) ;
#18763 = CARTESIAN_POINT ( 'NONE',  ( -50.65001634216351789, -24.15602025860895452, 10.28564288303536856 ) ) ;
#18764 = DIRECTION ( 'NONE',  ( -3.773278334453079618E-23, 0.9999999999976377785, 2.173523156925979975E-06 ) ) ;
#18765 = CARTESIAN_POINT ( 'NONE',  ( -19.80875734969026425, 5.965225279485572685, 31.02402280011862246 ) ) ;
#18766 = CARTESIAN_POINT ( 'NONE',  ( -21.99024891984110752, 1.279939690139831665, -1.500000000000002220 ) ) ;
#18767 = ORIENTED_EDGE ( 'NONE', *, *, #6082, .T. ) ;
#18768 = CARTESIAN_POINT ( 'NONE',  ( -65.60612770986470821, -23.85049219812685806, 10.88485053497527311 ) ) ;
#18769 = DIRECTION ( 'NONE',  ( -1.000000000000000000, -3.773278334444166432E-23, -8.201307841325785021E-29 ) ) ;
#18770 = CARTESIAN_POINT ( 'NONE',  ( -41.47025245262053517, -25.31624658460401278, 5.160615443078977016 ) ) ;
#18771 = EDGE_CURVE ( 'NONE', #14381, #85963, #2098, .T. ) ;
#18772 = CARTESIAN_POINT ( 'NONE',  ( -28.39339090630327789, -25.14676924958207849, 4.936952632524851836 ) ) ;
#18773 = CARTESIAN_POINT ( 'NONE',  ( -8.676776695296460673, 18.57322330470351091, 0.000000000000000000 ) ) ;
#18774 = DIRECTION ( 'NONE',  ( 0.000000000000000000, 0.000000000000000000, -1.000000000000000000 ) ) ;
#18775 = CARTESIAN_POINT ( 'NONE',  ( 20.90283063341239966, -4.354886778353011856, -1.500000000000002220 ) ) ;
#18776 = CARTESIAN_POINT ( 'NONE',  ( -81.52287095715006160, -24.64898659630367916, 1.056161002820826145 ) ) ;
#18777 = CARTESIAN_POINT ( 'NONE',  ( -48.85340342284951021, -25.32724633150700200, 4.398074151685130495 ) ) ;
#18778 = EDGE_CURVE ( 'NONE', #27354, #95501, #9183, .T. ) ;
#18779 = CARTESIAN_POINT ( 'NONE',  ( -64.59767640655398679, -23.96169478059713498, 10.65365249895718058 ) ) ;
#18780 = CARTESIAN_POINT ( 'NONE',  ( -126.5228709571500616, -23.48786465467241769, 11.44779295918253581 ) ) ;
#18781 = CARTESIAN_POINT ( 'NONE',  ( -8.190886813464794969, 21.05079722441571732, -1.500000000000002220 ) ) ;
#18782 = VECTOR ( 'NONE', #40561, 1000.000000000000114 ) ;
#18783 = CARTESIAN_POINT ( 'NONE',  ( -41.62287095715006302, -29.50250243563736774, 8.947779886222148704 ) ) ;
#18784 = ORIENTED_EDGE ( 'NONE', *, *, #72044, .T. ) ;
#18785 = VECTOR ( 'NONE', #83775, 1000.000000000000000 ) ;
#18786 = CARTESIAN_POINT ( 'NONE',  ( -89.52287095715006160, -29.50248528299804818, 1.056150453629040253 ) ) ;
#18787 = CARTESIAN_POINT ( 'NONE',  ( -79.55043832272009752, -24.15543982623907127, -0.2315651400026654261 ) ) ;
#18788 = CARTESIAN_POINT ( 'NONE',  ( -16.88869819569221065, 10.18974688345344148, 11.49999999999999645 ) ) ;
#18789 = CARTESIAN_POINT ( 'NONE',  ( -55.58953762381671737, -25.00182538069145011, 7.747789668545099317 ) ) ;
#18790 = VECTOR ( 'NONE', #87313, 1000.000000000000000 ) ;
#18791 = CARTESIAN_POINT ( 'NONE',  ( -96.55620429048340725, -23.47593901973091235, -1.443836447539001089 ) ) ;
#18792 = EDGE_CURVE ( 'NONE', #48449, #98958, #3559, .T. ) ;
#18793 = ORIENTED_EDGE ( 'NONE', *, *, #75754, .F. ) ;
#18794 = VECTOR ( 'NONE', #97333, 1000.000000000000000 ) ;
#18795 = DIRECTION ( 'NONE',  ( 1.252131230780251742E-15, -6.886721769291384876E-15, 1.000000000000000000 ) ) ;
#18796 = CARTESIAN_POINT ( 'NONE',  ( -70.52287095715007581, -24.92604778743017491, 8.074972756849348343 ) ) ;
#18797 = CARTESIAN_POINT ( 'NONE',  ( -124.5557933546448908, -23.96169478059714564, 10.65365249895717170 ) ) ;
#18798 = CARTESIAN_POINT ( 'NONE',  ( 0.9236959384754221958, 21.56878955078795812, 11.49999999999998934 ) ) ;
#18799 = DIRECTION ( 'NONE',  ( 3.773278334444166432E-23, -1.000000000000000000, 0.000000000000000000 ) ) ;
#18801 = CARTESIAN_POINT ( 'NONE',  ( -95.52287095715010423, -24.92604778743017846, 8.074972756849360778 ) ) ;
#18800 = AXIS2_PLACEMENT_3D ( 'NONE', #43921, #74852, #36309 ) ;
#18802 = CARTESIAN_POINT ( 'NONE',  ( -28.52287095715005805, -23.31185441368106126, 11.44779303854528685 ) ) ;
#18803 = CARTESIAN_POINT ( 'NONE',  ( 30.53060340732035982, -0.6647747205144264315, 20.86760796525322093 ) ) ;
#18804 = CARTESIAN_POINT ( 'NONE',  ( -19.19514693104756375, 4.742496307885142315, 11.49999999999998934 ) ) ;
#18805 = ORIENTED_EDGE ( 'NONE', *, *, #88074, .F. ) ;
#18806 = CARTESIAN_POINT ( 'NONE',  ( 18.81862293822770837, 7.596102252255398035, 11.49999999999999645 ) ) ;
#18807 = CARTESIAN_POINT ( 'NONE',  ( -7.640476926272304681, -5.876774720514415407, 20.25188360057253689 ) ) ;
#18808 = ORIENTED_EDGE ( 'NONE', *, *, #46692, .T. ) ;
#18809 = CARTESIAN_POINT ( 'NONE',  ( -110.6228709571500133, -24.15431212366391733, -0.2830839119429083839 ) ) ;
#18810 = PLANE ( 'NONE',  #78279 ) ;
#18811 = DIRECTION ( 'NONE',  ( 0.7071067811865515695, -0.7071067811865435759, 0.000000000000000000 ) ) ;
#18812 = CARTESIAN_POINT ( 'NONE',  ( -8.160000000000000142, 0.000000000000000000, 0.000000000000000000 ) ) ;
#18813 = DIRECTION ( 'NONE',  ( 0.000000000000000000, 0.000000000000000000, -1.000000000000000000 ) ) ;
#18814 = CARTESIAN_POINT ( 'NONE',  ( -71.62287095715004170, -23.72747288104470087, -1.053458166803226570 ) ) ;
#18815 = CARTESIAN_POINT ( 'NONE',  ( 4.692034869050136336, 19.47840706813412126, 11.49999999999998934 ) ) ;
#18816 = DIRECTION ( 'NONE',  ( -0.000000000000000000, -0.000000000000000000, -1.000000000000000000 ) ) ;
#18817 = ORIENTED_EDGE ( 'NONE', *, *, #70085, .T. ) ;
#18818 = AXIS2_PLACEMENT_3D ( 'NONE', #95041, #25533, #56503 ) ;
#18819 = B_SPLINE_CURVE_WITH_KNOTS ( 'NONE', 3,
 ( #45958, #54076, #30212, #76381, #13490, #14989 ),
 .UNSPECIFIED., .F., .F.,
 ( 4, 2, 4 ),
 ( 1.570887131795109485E-05, 0.001396322306279764976, 0.002776935741241578874 ),
 .UNSPECIFIED. ) ;
#18820 = PLANE ( 'NONE',  #87515 ) ;
#18821 = CARTESIAN_POINT ( 'NONE',  ( 8.749999999999769074, 18.74999999999999645, 2.100000000000000089 ) ) ;
#18822 = CARTESIAN_POINT ( 'NONE',  ( 13.91401389203221406, -6.475225279485573360, 158.0376437107427137 ) ) ;
#18823 = CARTESIAN_POINT ( 'NONE',  ( -113.5228709571500474, -24.50216790748205398, 0.6166512839542556135 ) ) ;
#18824 = DIRECTION ( 'NONE',  ( 1.000000000000000000, 0.000000000000000000, 0.000000000000000000 ) ) ;
#18825 = CARTESIAN_POINT ( 'NONE',  ( 15.48350366603705552, 4.450064631497443024, -28.28653584630381701 ) ) ;
#18826 = EDGE_CURVE ( 'NONE', #51471, #34388, #62615, .T. ) ;
#18827 = DIRECTION ( 'NONE',  ( 3.773278334444166432E-23, -1.000000000000000000, 0.000000000000000000 ) ) ;
#18828 = ORIENTED_EDGE ( 'NONE', *, *, #18638, .T. ) ;
#18829 = EDGE_CURVE ( 'NONE', #89496, #25882, #41123, .T. ) ;
#18830 = CARTESIAN_POINT ( 'NONE',  ( -3.780122020211411193, 19.97858748211865532, -1.500000000000002220 ) ) ;
#18832 = ADVANCED_FACE ( 'NONE', ( #28400 ), #35538, .T. ) ;
#18831 = VERTEX_POINT ( 'NONE', #3591 ) ;
#18833 = CARTESIAN_POINT ( 'NONE',  ( -21.95939045666098366, -6.591442671832903777, -1.500000000000002220 ) ) ;
#18834 = CARTESIAN_POINT ( 'NONE',  ( -32.61005697994687580, -23.73766607897670866, -1.055555164236442023 ) ) ;
#18835 = EDGE_CURVE ( 'NONE', #33008, #12032, #19355, .T. ) ;
#18836 = CARTESIAN_POINT ( 'NONE',  ( -122.5228709571500900, -24.34917612406837861, 0.1852690917426592365 ) ) ;
#18837 = EDGE_LOOP ( 'NONE', ( #84392, #78361, #12890, #86324 ) ) ;
#18838 = FACE_OUTER_BOUND ( 'NONE', #83190, .T. ) ;
#18839 = EDGE_CURVE ( 'NONE', #93507, #4166, #37517, .T. ) ;
#18840 = VECTOR ( 'NONE', #23280, 1000.000000000000227 ) ;
#18841 = CARTESIAN_POINT ( 'NONE',  ( 15.02167523160210294, 3.508919134408378770, -27.32290745209846250 ) ) ;
#18842 = CARTESIAN_POINT ( 'NONE',  ( -65.62287095715005592, -24.14406661707770496, 10.28769366152061160 ) ) ;
#18843 = CARTESIAN_POINT ( 'NONE',  ( -16.84575021678815432, -12.90291372800108505, 11.49999999999999645 ) ) ;
#18844 = CARTESIAN_POINT ( 'NONE',  ( -17.14978611337857473, 13.99085498846200437, -1.500000000000002220 ) ) ;
#18845 = CARTESIAN_POINT ( 'NONE',  ( 17.26003113218828489, 11.23261964116016642, -1.500000000000002220 ) ) ;
#18846 = AXIS2_PLACEMENT_3D ( 'NONE', #60493, #91410, #54372 ) ;
#18847 = ORIENTED_EDGE ( 'NONE', *, *, #86927, .F. ) ;
#18848 = CARTESIAN_POINT ( 'NONE',  ( -111.5895376238167245, -23.48783264082479505, -1.443836473390060604 ) ) ;
#18849 = EDGE_LOOP ( 'NONE', ( #27123, #60728, #96602, #56395, #68823 ) ) ;
#18850 = CARTESIAN_POINT ( 'NONE',  ( 6.996935307331598075, -6.376774720514424288, 21.22729008382901128 ) ) ;
#18851 = CARTESIAN_POINT ( 'NONE',  ( -7.749999999999996447, 25.69999999999999574, 0.000000000000000000 ) ) ;
#18852 = ORIENTED_EDGE ( 'NONE', *, *, #23672, .F. ) ;
#18853 = AXIS2_PLACEMENT_3D ( 'NONE', #53802, #62418, #60919 ) ;
#18854 = ORIENTED_EDGE ( 'NONE', *, *, #76878, .T. ) ;
#18855 = VECTOR ( 'NONE', #91482, 1000.000000000000000 ) ;
#18856 = VERTEX_POINT ( 'NONE', #5070 ) ;
#18857 = CARTESIAN_POINT ( 'NONE',  ( -83.62287095715007013, -24.65952944569304606, 1.056160979905700792 ) ) ;
#18858 = B_SPLINE_CURVE_WITH_KNOTS ( 'NONE', 3,
 ( #48054, #9982, #10986, #49562, #40936, #63292, #72396, #71898, #2383, #80492, #72896, #34328, #78984, #55678, #9483, #1878, #95223, #63802 ),
 .UNSPECIFIED., .F., .F.,
 ( 4, 2, 2, 2, 2, 2, 2, 2, 4 ),
 ( 4.336808689942017736E-18, 0.0005889077912318099479, 0.001177815582463615559, 0.001766723373695421170, 0.002355631164927226781, 0.002944538956159032175, 0.003533446747390838003, 0.004122354538622643831, 0.004711262329854449225 ),
 .UNSPECIFIED. ) ;
#18859 = CARTESIAN_POINT ( 'NONE',  ( -28.65224025812264586, -23.80901598000311026, 10.65365253163527015 ) ) ;
#18860 = CARTESIAN_POINT ( 'NONE',  ( 8.971512145086506962, -2.028487854913504584, -6.500000000000000000 ) ) ;
#18861 = CARTESIAN_POINT ( 'NONE',  ( -15.27568272636907665, 14.01247568063241999, -1.500000000000002220 ) ) ;
#18862 = CARTESIAN_POINT ( 'NONE',  ( -6.878457297428972161, 20.61903435171069532, 11.49999999999999645 ) ) ;
#18863 = ORIENTED_EDGE ( 'NONE', *, *, #9000, .F. ) ;
#18864 = DIRECTION ( 'NONE',  ( 0.000000000000000000, 0.000000000000000000, 1.000000000000000000 ) ) ;
#18865 = CARTESIAN_POINT ( 'NONE',  ( 2.677564053859940341, -5.876774720514407413, 19.16116138973293559 ) ) ;
#18866 = CARTESIAN_POINT ( 'NONE',  ( 18.93296920960566965, -11.98514031388154599, 11.49999999999998934 ) ) ;
#18867 = VECTOR ( 'NONE', #41042, 1000.000000000000000 ) ;
#18868 = FACE_OUTER_BOUND ( 'NONE', #54527, .T. ) ;
#18869 = LINE ( 'NONE', #33099, #77211 ) ;
#18870 = ORIENTED_EDGE ( 'NONE', *, *, #21584, .F. ) ;
#18871 = CARTESIAN_POINT ( 'NONE',  ( -84.62287095715005592, -24.64898659630367561, 1.056161002820826145 ) ) ;
#18872 = CARTESIAN_POINT ( 'NONE',  ( 8.160000000000000142, -6.754662360505033547, 7.925641719537454222 ) ) ;
#18873 = ORIENTED_EDGE ( 'NONE', *, *, #61831, .F. ) ;
#18874 = ORIENTED_EDGE ( 'NONE', *, *, #34686, .T. ) ;
#18875 = DIRECTION ( 'NONE',  ( 0.000000000000000000, 0.000000000000000000, 1.000000000000000000 ) ) ;
#18876 = ORIENTED_EDGE ( 'NONE', *, *, #51044, .T. ) ;
#18877 = CARTESIAN_POINT ( 'NONE',  ( 10.86157628581156764, 18.25448884030880592, -1.500000000000002220 ) ) ;
#18878 = ORIENTED_EDGE ( 'NONE', *, *, #13111, .F. ) ;
#18879 = CARTESIAN_POINT ( 'NONE',  ( -101.1944152955115044, -25.16311295231453826, 6.858246048749960799 ) ) ;
#18880 = CARTESIAN_POINT ( 'NONE',  ( 12.52028139621776326, 17.89958603277719718, -1.500000000000002220 ) ) ;
#18881 = CARTESIAN_POINT ( 'NONE',  ( -52.56018670930887993, -23.73791477778911840, 11.05961554403171476 ) ) ;
#18882 = CARTESIAN_POINT ( 'NONE',  ( -41.35158263814751933, -25.18430974066979999, 3.766621014227882203 ) ) ;
#18883 = CARTESIAN_POINT ( 'NONE',  ( -35.62287095715005592, -23.47593901973091235, -1.443836447539011525 ) ) ;
#18884 = CARTESIAN_POINT ( 'NONE',  ( 21.83686239284238084, -0.8075297431944471471, -1.500000000000002220 ) ) ;
#18885 = CARTESIAN_POINT ( 'NONE',  ( 6.763596848542221984, -5.876774720514425177, 21.40271460634751577 ) ) ;
#18886 = VERTEX_POINT ( 'NONE', #73102 ) ;
#18887 = DIRECTION ( 'NONE',  ( -0.000000000000000000, -1.000000000000000000, -0.000000000000000000 ) ) ;
#18888 = DIRECTION ( 'NONE',  ( -3.773278334453080206E-23, 0.9999999999976377785, 2.173523156925979975E-06 ) ) ;
#18889 = AXIS2_PLACEMENT_3D ( 'NONE', #58562, #18986, #49964 ) ;
#18890 = ORIENTED_EDGE ( 'NONE', *, *, #60333, .T. ) ;
#18891 = CARTESIAN_POINT ( 'NONE',  ( -32.52287095715006160, -23.47596703998600631, 11.44779298504229459 ) ) ;
#18892 = ORIENTED_EDGE ( 'NONE', *, *, #7932, .T. ) ;
#18893 = CARTESIAN_POINT ( 'NONE',  ( 11.84174468958795323, 6.475225279485574248, -27.06880646454217043 ) ) ;
#18894 = CARTESIAN_POINT ( 'NONE',  ( -10.24610470412292607, -22.99878645841938507, 0.8294870405985478312 ) ) ;
#18895 = CARTESIAN_POINT ( 'NONE',  ( -13.59518820711925358, -16.35513075224449864, -1.500000000000002220 ) ) ;
#18896 = FACE_OUTER_BOUND ( 'NONE', #83103, .T. ) ;
#18897 = CARTESIAN_POINT ( 'NONE',  ( 30.93860345374796594, 6.475225279485573360, 19.84760796525321780 ) ) ;
#18898 = EDGE_CURVE ( 'NONE', #34410, #4424, #11192, .T. ) ;
#18899 = DIRECTION ( 'NONE',  ( -3.773278334453079030E-23, 0.9999999999976377785, 2.173523156925979128E-06 ) ) ;
#18900 = DIRECTION ( 'NONE',  ( 0.000000000000000000, 0.9999999999976377785, 2.173523156925979128E-06 ) ) ;
#18901 = CARTESIAN_POINT ( 'NONE',  ( 7.440116899146960172, 17.95454168335740874, 11.49999999999998934 ) ) ;
#18902 = ADVANCED_FACE ( 'NONE', ( #81202 ), #25564, .T. ) ;
#18903 = LINE ( 'NONE', #3698, #26333 ) ;
#18904 = ORIENTED_EDGE ( 'NONE', *, *, #54831, .F. ) ;
#18905 = CARTESIAN_POINT ( 'NONE',  ( -18.23851433863309879, 7.102826447048048664, 11.49999999999999645 ) ) ;
#18906 = CARTESIAN_POINT ( 'NONE',  ( -5.576690828732316696, -5.876774720514415407, 20.34213149456667935 ) ) ;
#18907 = CARTESIAN_POINT ( 'NONE',  ( -42.62287095715004881, -23.48786465467240347, 11.44779295918255180 ) ) ;
#18908 = ORIENTED_EDGE ( 'NONE', *, *, #35129, .F. ) ;
#18909 = CARTESIAN_POINT ( 'NONE',  ( -39.56136241089613037, -25.29384247623274362, 5.536731341526268224 ) ) ;
#18910 = CARTESIAN_POINT ( 'NONE',  ( -89.63826309510754697, -23.73766607897671221, -1.055555164236434029 ) ) ;
#18911 = AXIS2_PLACEMENT_3D ( 'NONE', #9932, #93658, #31773 ) ;
#18912 = DIRECTION ( 'NONE',  ( -3.773278334453079618E-23, 0.9999999999976377785, 2.173523156925979975E-06 ) ) ;
#18913 = B_SPLINE_CURVE_WITH_KNOTS ( 'NONE', 3,
 ( #25561, #56531, #77332, #718 ),
 .UNSPECIFIED., .F., .F.,
 ( 4, 4 ),
 ( 0.000000000000000000, 9.999999999998897304E-05 ),
 .UNSPECIFIED. ) ;
#18914 = CARTESIAN_POINT ( 'NONE',  ( -81.23841534186585989, -25.24813948233231642, 7.364952454261663561 ) ) ;
#18915 = CARTESIAN_POINT ( 'NONE',  ( 9.442166470422634461, 17.27452087139410963, 11.49999999999998934 ) ) ;
#18916 = ORIENTED_EDGE ( 'NONE', *, *, #46341, .T. ) ;
#18917 = CARTESIAN_POINT ( 'NONE',  ( -33.52287095715006160, -29.50250786944525672, 11.44777988621624409 ) ) ;
#18918 = DIRECTION ( 'NONE',  ( -3.773278334444167608E-23, 1.000000000000000000, 0.000000000000000000 ) ) ;
#18919 = VECTOR ( 'NONE', #59907, 1000.000000000000000 ) ;
#18920 = APPLICATION_PROTOCOL_DEFINITION ( 'international standard', 'config_control_design', 1994, #59603 ) ;
#18921 = VERTEX_POINT ( 'NONE', #29548 ) ;
#18922 = CARTESIAN_POINT ( 'NONE',  ( 3.748501943728875574, -6.376774720514426065, 21.47917144995767558 ) ) ;
#18923 = CARTESIAN_POINT ( 'NONE',  ( -72.52287095715007581, -23.47593901973090169, -1.443836447538996870 ) ) ;
#18924 = CARTESIAN_POINT ( 'NONE',  ( -47.59972484022089390, -23.96119346886880663, -0.6495511937831951466 ) ) ;
#18925 = CARTESIAN_POINT ( 'NONE',  ( -105.6228709571500133, -24.83620972994591725, 8.398175272781362111 ) ) ;
#18926 = CARTESIAN_POINT ( 'NONE',  ( 30.77564450787169648, -1.682774720514426114, -9.689394075852828081 ) ) ;
#18927 = VECTOR ( 'NONE', #83374, 1000.000000000000000 ) ;
#18928 = CIRCLE ( 'NONE', #77213, 1.050000000000000488 ) ;
#18929 = FACE_OUTER_BOUND ( 'NONE', #96958, .T. ) ;
#18930 = DIRECTION ( 'NONE',  ( -1.000000000000000000, -3.773278334444167608E-23, -8.201307833595939069E-29 ) ) ;
#18931 = CARTESIAN_POINT ( 'NONE',  ( -2.986242917674419850, -19.73498743542299749, 11.49999999999998934 ) ) ;
#18932 = FACE_OUTER_BOUND ( 'NONE', #81779, .T. ) ;
#18933 = CARTESIAN_POINT ( 'NONE',  ( -14.63867168220055781, -13.42826565525684579, -1.500000000000002220 ) ) ;
#18934 = VERTEX_POINT ( 'NONE', #69107 ) ;
#18935 = AXIS2_PLACEMENT_3D ( 'NONE', #34633, #19884, #34134 ) ;
#18936 = FACE_OUTER_BOUND ( 'NONE', #34352, .T. ) ;
#18937 = EDGE_CURVE ( 'NONE', #38118, #37689, #29051, .T. ) ;
#18938 = FACE_OUTER_BOUND ( 'NONE', #40573, .T. ) ;
#18939 = DIRECTION ( 'NONE',  ( 1.000000000000000000, -0.000000000000000000, 0.000000000000000000 ) ) ;
#18940 = CARTESIAN_POINT ( 'NONE',  ( 13.64113475014448618, -3.316774720514425567, -28.24100986136700442 ) ) ;
#18941 = CARTESIAN_POINT ( 'NONE',  ( 10.19739565540945492, -18.13666118385682680, 11.49999999999999645 ) ) ;
#18942 = CARTESIAN_POINT ( 'NONE',  ( -7.536766146225033047, -6.376774720514411854, 19.63296556618507438 ) ) ;
#18943 = DIRECTION ( 'NONE',  ( -0.000000000000000000, 0.000000000000000000, 1.000000000000000000 ) ) ;
#18944 = CARTESIAN_POINT ( 'NONE',  ( 13.72848742581335912, -18.28091200367991576, 11.49999999999999645 ) ) ;
#18945 = ORIENTED_EDGE ( 'NONE', *, *, #96745, .F. ) ;
#18946 = CARTESIAN_POINT ( 'NONE',  ( -116.6228709571500559, -29.50247984919015209, -1.443849546365046699 ) ) ;
#18947 = B_SPLINE_CURVE_WITH_KNOTS ( 'NONE', 3,
 ( #33514, #47745, #70571, #18291, #1067, #41641 ),
 .UNSPECIFIED., .F., .F.,
 ( 4, 2, 4 ),
 ( 6.391158118972358895E-06, 0.001387004593080794169, 0.002767618028042615873 ),
 .UNSPECIFIED. ) ;
#18948 = CARTESIAN_POINT ( 'NONE',  ( -89.62287095715004170, -23.47596703998600631, 11.44779298504227860 ) ) ;
#18949 = VERTEX_POINT ( 'NONE', #36667 ) ;
#18950 = EDGE_CURVE ( 'NONE', #28719, #53939, #66483, .T. ) ;
#18951 = B_SPLINE_CURVE_WITH_KNOTS ( 'NONE', 3,
 ( #89010, #19986, #50952, #12367, #35723, #90003 ),
 .UNSPECIFIED., .F., .F.,
 ( 4, 2, 4 ),
 ( 1.570887131794333942E-05, 0.001396322306279758037, 0.002776935741241572803 ),
 .UNSPECIFIED. ) ;
#18952 = CARTESIAN_POINT ( 'NONE',  ( -5.512817753899047268, 19.46650688538001361, 11.49999999999998934 ) ) ;
#18953 = CARTESIAN_POINT ( 'NONE',  ( 6.830155907162054341, -6.376774720514427841, 21.76451523534627341 ) ) ;
#18954 = CARTESIAN_POINT ( 'NONE',  ( -123.6228709571500559, -23.47593901973091235, -1.443836447538997536 ) ) ;
#18955 = EDGE_CURVE ( 'NONE', #46348, #25493, #5718, .T. ) ;
#18956 = CARTESIAN_POINT ( 'NONE',  ( -111.6228709571500701, -23.48786465467241769, 11.44779295918254114 ) ) ;
#18957 = EDGE_CURVE ( 'NONE', #97111, #15522, #83336, .T. ) ;
#18958 = ORIENTED_EDGE ( 'NONE', *, *, #57500, .T. ) ;
#18959 = CARTESIAN_POINT ( 'NONE',  ( -79.62531161443044425, -25.31170139299580413, 4.690176232765736586 ) ) ;
#18960 = LINE ( 'NONE', #26587, #82653 ) ;
#18961 = CARTESIAN_POINT ( 'NONE',  ( 17.55240489776628721, -9.587225365216566431, -1.500000000000002220 ) ) ;
#18962 = EDGE_CURVE ( 'NONE', #6678, #10266, #13816, .T. ) ;
#18963 = CARTESIAN_POINT ( 'NONE',  ( 6.892386425805808514, -19.84609432511738447, 11.49999999999999645 ) ) ;
#18964 = VECTOR ( 'NONE', #66108, 1000.000000000000000 ) ;
#18965 = CARTESIAN_POINT ( 'NONE',  ( -29.81066036315064949, -25.25719168430799044, 5.128783157772433654 ) ) ;
#18966 = PLANE ( 'NONE',  #31901 ) ;
#18967 = CARTESIAN_POINT ( 'NONE',  ( 19.90762846840230083, -9.494064324355022677, -1.500000000000002220 ) ) ;
#18968 = EDGE_CURVE ( 'NONE', #45742, #72919, #56179, .T. ) ;
#18969 = CARTESIAN_POINT ( 'NONE',  ( -39.54917078480641379, -25.31589227305247647, 4.610327192741620728 ) ) ;
#18970 = CARTESIAN_POINT ( 'NONE',  ( -95.62287095715005592, -29.50247984919015209, -1.443849546365050029 ) ) ;
#18971 = CARTESIAN_POINT ( 'NONE',  ( -72.54160130282839702, -24.51314013834316796, 0.6176544820404143987 ) ) ;
#18972 = DIRECTION ( 'NONE',  ( 0.000000000000000000, -1.000000000000000000, 0.000000000000000000 ) ) ;
#18973 = ORIENTED_EDGE ( 'NONE', *, *, #71438, .T. ) ;
#18974 = ORIENTED_EDGE ( 'NONE', *, *, #44352, .T. ) ;
#18975 = CARTESIAN_POINT ( 'NONE',  ( 6.660000000000001030, -10.15233964170348457, 0.003711184059992174607 ) ) ;
#18976 = CARTESIAN_POINT ( 'NONE',  ( -84.62287095715005592, -23.47593901973091235, -1.443836447539004642 ) ) ;
#18978 = EDGE_CURVE ( 'NONE', #80003, #28802, #21922, .T. ) ;
#18977 = CARTESIAN_POINT ( 'NONE',  ( -4.854568188115255367, -5.876774720514410077, 19.46611907402017394 ) ) ;
#18979 = CARTESIAN_POINT ( 'NONE',  ( -1.317410511717131971, -20.46822056820986546, -1.500000000000002220 ) ) ;
#18980 = ORIENTED_EDGE ( 'NONE', *, *, #46029, .T. ) ;
#18981 = DIRECTION ( 'NONE',  ( -1.000000000000000000, 0.000000000000000000, -0.000000000000000000 ) ) ;
#18982 = CARTESIAN_POINT ( 'NONE',  ( 6.727829057902616761, -5.876774720514417183, 20.13865202822440281 ) ) ;
#18983 = CARTESIAN_POINT ( 'NONE',  ( -41.52287095715006870, -23.47596703998600631, 11.44779298504229281 ) ) ;
#18984 = CARTESIAN_POINT ( 'NONE',  ( -19.39139147909919458, -11.06001032434818576, 11.49999999999998934 ) ) ;
#18985 = AXIS2_PLACEMENT_3D ( 'NONE', #42141, #4061, #34011 ) ;
#18986 = DIRECTION ( 'NONE',  ( 0.7512896232465888779, 8.688531644690855961E-16, 0.6599726524652355097 ) ) ;
#18987 = DIRECTION ( 'NONE',  ( -0.000000000000000000, 1.000000000000000000, -0.000000000000000000 ) ) ;
#18988 = EDGE_LOOP ( 'NONE', ( #5181, #92852, #13658, #62670 ) ) ;
#18989 = CARTESIAN_POINT ( 'NONE',  ( -32.62287095715004881, -24.64965695001467694, 8.947790433994189385 ) ) ;
#18990 = CARTESIAN_POINT ( 'NONE',  ( 3.165726958143470160, -5.876774720514421624, 21.14296526391294506 ) ) ;
#18991 = B_SPLINE_CURVE_WITH_KNOTS ( 'NONE', 3,
 ( #69451, #100369, #92774, #23259, #56747, #35268, #43382, #50994, #41506, #97159, #35765, #2954, #59604, #87678, #36260, #66233, #66735, #4812, #87174, #5801, #95290, #90535, #67224, #98137, #82421, #44377, #20516, #97648, #27653, #74320, #58598, #82915, #72459, #18161, #5301, #25774, #17661, #28150, #21017, #41008, #28644, #59108, #74805, #90046, #51986, #20028, #12408, #13403, #51487, #89545, #43872, #81929, #12905, #75303, #67722, #36757, #25269, #49133, #80060, #56248, #48632, #64368, #79559, #10048, #10545, #71965, #2446, #33379, #92525, #68207, #37748, #98636, #83415, #60110, #69706, #99626, #68708, #14400, #77292, #76296, #61103, #92031, #53496, #30128, #93021, #44880, #31127, #22503, #7795, #85414, #15398, #53987, #22004, #99135, #84421, #45381, #77788, #84914, #52485, #6791, #14899, #29635, #60609, #29136, #52989, #13902, #23498, #91034, #45868, #54477, #15900, #75801, #91531, #83922, #21508, #76785, #6301, #46865, #37259, #7288, #8297, #38239, #69197, #30631, #100114, #61608, #39241, #22999, #46360, #38738, #185, #62101, #40254, #48876, #49381, #16908, #80313, #64115, #78295, #8802, #1194, #48373, #93519, #54981, #24014, #71204, #25015, #25526, #56498, #87420, #94030, #55994, #94531, #71708, #18413, #72211, #95035, #33643, #10300, #79803, #17918, #26023, #41258, #86919, #87929, #39741, #683, #17412, #70199, #62594, #79302, #10803, #16398, #64623, #32129, #2701, #85926, #9799, #95536, #2206, #56993, #31629, #47367, #70699, #63102, #40750, #55484, #24516, #86422, #47871, #78791, #33135, #9289, #1700, #32632, #63610, #34646, #80817, #98013, #20894, #65615, #96533, #50871, #4193, #27027, #27532, #5182, #51365, #49885, #35643, #73212, #73699, #96038, #57996, #20390, #88931, #82304, #35146, #97036, #66117, #36136, #74687, #11794, #12783, #28514, #58985, #97528, #19403, #42282, #58489, #50374, #51867, #28027, #26532, #81312, #89426, #18905, #59477, #42766, #43752, #19898, #67105, #81810, #90418, #82798, #89921, #41769, #12284, #3700, #43260, #74202, #72712, #3209, #57497, #4693, #66616, #34151, #65118, #88431, #11300, #99509, #38625, #13281, #52860, #69588, #23382, #52362, #37627, #68, #92905, #30007, #83798, #60488, #91907, #84293, #15280, #22382, #44255, #61979, #54366, #99011, #7171, #21385, #83296, #44752, #21882, #60979, #68584, #29508, #14278, #53367, #91405, #46243, #75676, #22877, #45251, #14779, #45744, #75183, #5677, #13776, #77173, #53865, #84797, #69076, #31012, #38120, #76666, #76176, #100001, #6674, #36629, #30511, #6176, #92405, #37129, #67597, #61480, #7679, #29013, #98515, #59983, #90917, #68088, #10187, #78670, #71092, #17802, #79189, #86305, #2091, #24403, #86803, #17293, #25909, #9178, #64508, #85809, #47251, #95421, #40139, #23898, #41148, #85297, #8689, #15785, #72100, #1076, #9685, #54868, #55371, #46750, #70081, #77673, #56383, #16790, #47756, #32017, #64003, #62991, #33027, #39124, #93912, #1584, #32521, #94917, #25408, #63496, #94417, #39628, #2585, #8184, #70583, #71595, #78176, #62477, #48258, #24900, #55878, #565, #40644, #87303, #48764, #79690, #33522, #31514, #93404, #16289, #42158, #43635, #73589, #34027, #5065, #12171, #35029, #80198, #41650, #10689, #57881, #11672, #43142, #18788, #66503, #65501, #96921, #66001, #18301, #36013, #26414, #3091, #49271, #26910, #12673, #19285, #74575, #50754, #4077, #66988, #95920, #87813, #81196, #49767, #35532, #57387, #72596, #27414, #20276, #65004, #97417, #4583, #11186, #42655, #88315, #27906, #74090, #97901, #56883, #80697, #58373, #73096, #58862, #89311, #3586, #50256, #34529, #96423, #88819, #19780, #81699, #89806, #51246, #82186, #38513, #77060, #52250, #37514, #91301, #13661, #14164, #92296, #38014, #90303, #99888, #29398, #67981, #44633, #7064, #6061, #21770, #5563, #46135, #37017, #30395, #45141, #7564, #75561, #22767, #83683, #28903, #51751, #76068, #59869, #6567, #98903, #68471, #69464, #60377, #53754, #99405, #90805, #82684, #29899, #20773, #52744, #28395, #61368, #45635, #59358, #60867, #84682, #13165, #76555, #68964, #91790, #22268, #83177, #44136, #75063, #53252, #14671, #21274, #36509, #84181, #15168, #67474, #98399, #47640, #69962, #93287, #94795, #41026, #79067, #79574, #47139, #10065, #94292, #8063, #39009, #31402, #8569, #16670, #24291, #16171, #70469, #9063, #78055, #32909, #62361, #9560, #39517, #40014, #1463, #48650, #1967, #24778, #63881, #40528, #71479, #55758, #17675, #86685, #78556, #954, #70973, #31904, #56263, #62879, #23782, #25284, #447, #61866, #87188, #54755, #100386, #92790, #32406, #48141, #63379, #30899, #93796, #86188, #23271, #17172, #55257, #54254, #85184, #15673, #46640, #77558, #85690, #51126, #97301, #27785, #25788, #64887, #10561, #58738, #82070, #95797, #12556, #89687, #88197, #65879, #41522, #11066, #71979, #56763, #33394, #43021, #72978, #42032, #26291, #50627, #18668, #12052, #65382, #26790, #3468, #66371, #42533, #73965, #50134, #2461, #20164, #64386, #57267, #95303, #88697, #49151, #87693, #27293, #19165, #96302, #49642, #34405, #81078, #80572, #4463, #33902, #81581, #57754, #11554, #73467, #18177, #80077, #72476, #2969, #3961, #34905, #96799, #58248, #89193, #19662, #35414, #91174, #83050, #99764, #59746, #5443, #22147, #44007, #4951, #21648, #6940, #59240, #53134, #91668, #98277, #29279, #66864, #84061, #60250, #76435, #37401, #44513, #60746, #13543, #45021, #75941, #84559, #36894, #22643, #74939, #36395, #53635, #67858, #14546, #52621, #75438, #43521, #92171, #68846, #90679, #68349, #13046, #5938, #74457, #28281, #35896, #45519, #98779, #83557, #21159, #37894, #52127, #14040, #20658, #61248, #6445, #30270, #99282, #97789, #29779, #90183, #51629, #82564, #67357, #28783, #15544, #828, #31273, #94674, #70849, #69340, #93162, #31780, #23652, #32277, #63246, #85559, #62751, #40399, #15043, #54625, #71352, #25158, #54132, #39391, #1841, #56135, #93668, #16042, #62242, #24160, #47010, #77930, #94170, #8442, #70345, #92666, #32779, #55130, #9436, #61747, #48016, #86064, #24654, #63759, #55634, #1341, #38885, #46506, #16538, #47514, #46015, #86565, #100259, #78439, #8940, #39889, #17049, #76934, #69847, #30777, #7432, #38387, #78941, #23144, #85057, #77434, #7936, #327, #66257, #3356, #57141, #33783, #65265, #57634, #89072, #96188, #17555, #97181, #64768, #27675, #80958, #95182, #25666, #18054, #95683, #34291, #10948, #2850, #88078, #26676, #26167, #19548, #49021, #96675, #18552, #88576, #19050, #35292, #50508, #11442, #81465, #27175, #58136, #42421, #4342, #73352, #50023, #49524, #3846, #80456, #42906, #41913, #79952, #65757, #87569, #48521, #34786, #2344, #11940, #73842, #41400, #72855, #9941, #87064, #79449, #40893, #71855, #33273, #64260, #72354, #56638, #10438, #6323, #36286, #13427, #37773, #83944, #68728, #52008, #37279, #75327, #28665, #99647, #6815, #82446, #67744, #21039, #43896, #44400, #22026, #68230, #66756, #52508, #90066, #74341, #99159, #29657, #60632, #60133, #14424, #82938, #5822, #91553, #83437, #59627, #75824, #98160, #91057, #21531, #58624, #36780, #89569, #59130, #20539, #20053, #98661, #53014, #45399, #51015, #12927, #81951, #76316, #74829, #13926, #28171, #90559, #12435, #43405, #4833, #35786, #29159, #44902, #5323, #97674, #67243, #51512, #7309, #86818, #63508, #25922, #76810, #64523, #1595, #41160, #18316, #48781, #87317, #55381, #30658, #17306, #47769, #10705, #17815, #84440, #9190, #48270, #40150, #93923, #61124, #86320, #14920, #56898, #30150, #71106, #87830, #41670, #69220, #55891, #49285, #72610, #79201, #32534, #78683, #9699, #2106, #33538, #40659, #10202, #92053, #94428, #22523, #25423, #38262, #100135, #63004, #24914, #71608, #33039, #64020, #94934, #56397, #79704, #95435, #24416, #72113, #2604, #80212, #53517, #45893, #16803, #27921, #67005, #43652, #12688, #58882, #20792, #97436, #81713, #42671, #50772, #73604, #59376, #19304, #65519, #82205, #3600, #65021, #97917, #34545, #51767, #26929, #12185, #66019, #88835, #89328, #28410, #74589, #11201, #89821, #96437, #35046, #57402, #57898, #5081, #50271, #3109, #82701, #96937, #90320, #49784, #36032, #4095, #13180, #44150, #20291, #51265, #81214, #11688, #19797, #27431, #34044, #95935, #88330, #58391, #43163, #74105, #26436, #18806, #4599, #80717, #42174, #73113, #35547, #66517, #85198, #13681, #99419, #30913, #54272, #91810, #45157, #21784, #53266, #45649, #77074, #84194, #5580, #15689, #52761, #75084, #68977, #83193, #44648, #6079, #83698, #22283, #29913, #91315, #76080, #14684, #14180, #7579, #37031, #84696, #6579, #76574, #7079, #23287, #38527, #99902, #69485, #15187, #46150, #30414, #92805, #61382, #38028, #37534, #92310, #68484, #61883, #60879, #67993, #53769, #75577, #36525, #22780, #98919, #100400, #67493, #98415, #28918, #59887, #90819, #21293, #52264, #29412, #60392, #47656, #63901, #86206, #48156, #79081, #87709, #40032, #25807, #47155, #2479, #462, #39533, #85707, #33410, #56777, #70486, #16185, #64402, #46655, #969, #77574, #71996, #62893, #40543, #78072, #16685, #8079, #31418, #39026, #78571, #9077, #93814, #70991, #95319, #69978, #62375, #93303, #24304, #48667, #63392, #23796, #55270, #10081, #1482, #8584, #54770, #32420, #31923, #94309, #24796, #55774, #1982, #86699, #17187, #9581, #71493, #94812, #25299, #32923, #56279, #87202, #17693, #79589, #41040, #4480, #80590, #95812, #50645, #42051, #34921, #88711, #65402, #96814, #89209, #20179, #27306, #49166, #66882, #59258, #3482, #4965, #65895, #26311, #97806, #73983, #58269, #41541, #2986, #72492, #19676, #96319, #51142, #11081, #27801, #26808, #81594, #12066, #80092, #28299, #88215, #64903, #10576, #19183, #74474, #81092, #35913, #43040, #35428, #18195, #57769, #33923, #34422, #72994, #97317, #18682, #57284, #66390, #82090, #49657, #58755, #89708, #50153, #3979, #11569, #12573, #43537, #42548, #73480, #38405, #6959, #29295, #91684, #22166, #30798, #83575, #69360, #90700, #52142, #100277, #14059, #51648, #90199, #59765, #36412, #82587, #60268, #46034, #52639, #76955, #68366, #91191, #37420, #21664, #7449, #5955, #83067, #68861, #21178, #13063, #99302, #53651, #5461, #99779, #37911, #44531, #75957, #44022, #30287, #76454, #22663, #84076, #45039, #61266, #6463, #53151, #14566, #20678, #29796, #74959, #13562, #75455, #67375, #60762, #92187, #45534, #84575, #98293, #28799, #36910, #67873, #15066, #98802, #846, #61763, #46524, #23162, #32795, #62769, #31801, #77947, #24176, #17570, #54154, #92682, #79468, #39409, #63776, #78454, #40910, #93687, #71371, #48542, #78957, #17065, #85576, #62258, #47532, #8460, #71870, #48032, #15563, #70361, #8957, #55150, #9458, #40415, #86079, #39905, #16058, #85077, #16556, #87080, #2358, #343, #70870, #9959, #77453, #1360, #32295, #63266, #94184, #24670, #94690, #55651, #7953, #38907, #69863, #47031, #31291, #93185, #23670, #54644, #86579, #1854, #25176, #56151, #3372, #42433, #10963, #66270, #95698, #42924, #41929, #73368, #11459, #72870, #33289, #97193, #50522, #87590, #34304, #50039, #65283, #81480, #11953, #96205, #19064, #88097, #51027, #95198, #18565, #19565, #26186, #10453, #65776, #57159, #26691, #43422, #80972, #3864, #34803, #35308, #96690, #64276, #81972, #74354, #49540, #20065, #27191, #41416, #12450, #89087, #58149, #56653, #18070, #49040, #57650, #88591, #73860, #80470, #4359, #27692, #58638, #89585, #25682, #79967, #2867, #72372, #33799, #64782, #61142, #67757, #92067, #99173, #21547, #22537, #43910, #35799, #29172, #97690, #83453, #84454, #51527, #68742, #36300, #37790, #28185, #44916, #53028, #6337, #30166, #98679, #91071, #99660, #29674, #5840, #22046, #44417, #37297, #83959, #82950, #60150, #14937, #53529, #45909, #59142, #98178, #74841, #4845, #66772, #28680, #90083, #20558, #21053, #60644, #5344, #75340, #82462, #12941, #91565, #67256, #36795, #59645, #90574, #52024, #68244, #13942, #75839, #52520, #14439, #13443, #45411, #76334, #6829, #86457, #63643, #94063, #32165, #221, #38277, #56026, #46398, #23032, #69234, #46900, #32668, #39276, #94567, #70739, #93554, #25051, #15437, #7322, #716, #76824, #100152, #55019, #86955, #54027, #40288, #92561, #55524, #24551, #31163, #62635, #30671, #16943, #63138, #17442, #61641, #84951, #85957, #62133, #78825, #77328, #47905, #54515, #31665, #7829, #38778, #69740, #70236, #9325, #24048, #77823, #93058, #23536, #85448, #16434, #47403, #15934, #78331, #71242, #1728, #8331, #1231, #8835, #39772, #71744, #57030, #27065, #79338, #48409, #19441, #95571, #65652, #72749, #81350, #33678, #96564, #10841, #48912, #2238, #41805, #33169, #26058, #9832, #58029, #42313, #64150, #87966, #3247, #18447, #73244, #3738, #49419, #34181, #2739, #50406, #95074, #64657, #11337, #41289, #56528, #57531, #72247, #80345, #40785, #18941, #49921, #34679, #25559, #80852, #17949, #87460, #79838, #65157, #10336, #96076, #88968, #26571, #88466, #16771, #61963, #23367, #92889, #39612, #93898, #94401, #550, #48239, #47233, #78654, #47738, #62460, #39106, #24386, #54852, #17786, #24883, #54351, #16274, #55355, #78156, #55860, #86786, #8671, #86288, #93389, #38612, #70563, #63987, #48749, #77660, #62973, #94898, #79671, #9161, #1060, #85792, #40120, #71076, #40626, #1567, #69572, #87285, #51, #23877, #25390, #46734, #8167, #70063, #32001, #32506, #63479, #17278, #79171, #9671, #71579, #2073, #31496, #33012, #56367, #30996, #85280, #15769, #37321, #93080, #54534, #85469, #77845, #84479, #8351, #15459, #38300, #39300, #60666, #52541, #45933, #21569, #13963, #100175, #739, #68268, #15955, #53049, #46921, #44939, #61663, #7345, #75861, #69760, #7852, #70256, #31692, #62660, #30691, #6857, #23565, #83476, #241, #99682, #76843, #6364, #99196, #29696, #91589, #14459, #22068, #92088, #83980, #45439, #76354, #92580, #14960, #37810, #69257, #68762, #31184, #30186, #46419, #61168, #53549, #22557, #23059, #54048, #84974, #77350, #38799, #62157, #87987, #39800, #26078, #63668, #2757, #80370, #10353, #48930, #56047, #3264, #40802, #63157, #86476, #18464, #34203, #94588, #72269, #72770, #40310, #10860, #9850, #70758, #41824, #79859, #71765, #16453, #78351, #47424, #25069, #48428, #41310, #33698, #64676, #16962, #79358, #17464, #95093, #93575, #8852, #86972, #32185, #57051, #49436, #2257, #24071, #87479, #33190, #55040, #94084, #85978, #64172, #1256, #24569, #25578, #55546, #47926, #78847, #9347, #71259, #95591, #1749, #56551, #32687, #17971, #51422, #20949, #44314, #13334, #43314, #50424, #67159, #65174, #12837, #42820, #19956, #75240, #90474, #51921, #18963, #43806, #81865, #35199, #5732, #96101, #88987, #74252, #27588, #81367, #50927, #28574, #74740, #73264, #59038, #96586, #97090, #49941, #19457, #42331, #97583, #26589, #82850, #73751, #98067, #12344, #57549, #11850, #59534, #4746, #65670, #88488, #35697, #80871, #4250, #11358, #3758, #82358, #34699, #28085, #27084, #66171, #5237, #36195, #58539, #66672, #89479, #58051, #89976, #20450, #22925, #99065, #13833, #69127, #60542, #52920, #6726, #45797, #14330, #69639, #29563, #91457, #91963, #61032, #38167, #85346, #52418, #7728, #117, #44808, #46292, #92453, #54411, #30564, #14829, #76228, #84346, #37679, #92954, #83852, #21935, #76718, #15832, #83349, #31056, #68141, #62028, #29067, #7218, #84850, #100050, #23428, #30059, #22435, #46801, #61536, #68639, #53916, #99556, #15328, #77221, #45307, #53418, #77722, #36687, #67652, #90968, #38674, #75726, #98571, #60040, #21438, #6229, #37185, #24453, #2143, #78227, #47801, #8235, #93455, #70130, #39675, #40188, #62526, #63039, #85860, #40690, #86848, #48306, #63547, #71141, #2637, #54915, #41196, #78720, #17853, #95472, #25456, #64054, #32065, #8738, #39175, #72149, #56432, #56931, #71642, #33577, #23948, #70631, #1127, #618, #93961, #16336, #64555, #31563, #9224, #25959, #18350, #47302, #32566, #87864, #1634, #49318, #55926, #55420, #86359, #16843, #94469, #24952, #87353, #17345, #79236, #9735, #33077, #94967, #48814, #79739, #10234, #96972, #4130, #28446, #57933, #27472, #88873, #97469, #27959, #50310, #66052, #34584, #97950, #41706, #65555, #66558, #42214, #57435, #12220, #3636, #42704, #90356, #58429, #49824, #50808, #82239, #89361, #10742, #59409, #20829, #96469, #67042, #19829, #88364, #80248, #35583, #81747, #3143, #65056, #34084, #81245, #35080, #58915, #89858, #26959, #43198, #74137, #4630, #72648, #95973, #51299, #12718, #18843, #20325, #43686, #26472, #74625, #5118, #19343, #36070, #11727, #80756, #73639, #73147, #11237, #30951, #98451, #15226, #83237, #84737, #44190, #91849, #99943, #53301, #77112, #45191, #37569, #46184, #45686, #52801, #69018, #91350, #84233, #14719, #29445, #6617, #61917, #7619, #38569, #5618, #44690, #90854, #69526, #92844, #75610, #51805, #8, #68031, #76609, #21325, #21825, #82736, #36560, #13218, #13720, #83735, #67531, #6115, #28953, #7114, #29952, #22323, #68521, #14215, #75125, #59925, #52301, #76116, #61420, #37066, #30456, #38062, #98957, #60425, #99452, #60920, #92346, #22819, #53803, #48705, #23325, #62931, #79627, #33454, #62419, #47692, #10119, #2524, #40076, #93851, #70522, #1519, #94351, #25343, #24344, #2025, #64444, #1012, #54310, #17230, #31453, #93342, #54807, #31958, #71030, #78611, #39571, #55311, #32458, #86244, #56321, #85745, #32967, #16725, #9117, #24840, #72038, #39065, #94853, #87241, #23834, #63944, #79127, #41083, #48195, #63434, #55814, #86742, #9621, #85236, #40582, #16228, #17737, #47193, #70015, #15725, #78110, #46694, #77614, #71533, #8125, #502, #8623, #88758, #81134, #27844, #89249, #96360, #12110, #34466, #96859, #27351, #35958, #19229, #74516, #20220, #51191, #49206, #88253, #33961, #82132, #5008, #18727, #95359, #12618, #11121, #19717, #64941, #65441, #25843, #80134, #56820, #66438, #26849, #10626, #49706, #72532, #58312, #73527, #34964, #50193, #57816, #89750, #41588, #58800, #11613, #4521, #43577, #43083, #50690, #80636, #95857, #42590, #42090, #74026, #87752, #81637, #18236, #3026, #26349, #57324, #73036, #3521, #35469, #97362, #4018, #65937, #21219, #84624, #28340, #52188, #53194, #28849, #44073, #22707, #46079, #83624, #36955, #13607, #45082, #37462, #68904, #76003, #97846, #15114, #7501, #83117, #53696, #14106, #75006, #76998, #22211, #6510, #90246, #44574, #67923, #68410, #75503, #99829, #59812, #76498, #6003, #99343, #29841, #59302, #66927, #84124, #29340, #5504, #30336, #20721, #60310, #51691, #60809, #98844, #91733, #91238, #82624, #21711, #90745, #45581, #67421, #13107, #14610, #61310, #36453, #7005, #37952, #52685, #92234, #98342, #86628, #24720, #94737, #32341, #39459, #55701, #77996, #39956, #70917, #79515, #31850, #17620, #38950, #390, #48592, #62818, #17113, #55199, #8508, #38453, #87128, #62306, #47582, #23721, #24227, #1905, #48081, #46574, #63317, #69905, #70409, #92727, #93231, #15609, #1407, #16605, #78501, #93732, #895, #32848, #85123, #71414, #86129, #9003, #31340, #61807, #94235, #30841, #79007, #69408, #63824, #9505, #100325, #40465, #25224, #56202, #23214, #54199, #77500, #8002, #54691, #85626, #16110, #47081, #33335, #97601, #2406, #50946, #10004, #44331, #28594, #60060, #43824, #5753, #64327, #81387, #73769, #40962, #66189, #95244, #36707, #71922, #81884, #98088, #4268, #89003, #74759, #35217, #74271, #21458, #59059, #11868, #97110, #67673, #52437, #12360, #90492, #90987, #58556, #25731, #5254, #19476, #50440, #67176, #89996, #58070, #42839, #27607, #43333, #66690, #59556, #20968, #51939, #89495, #28101, #35717, #12856, #19977, #4763, #82868, #75260, #20469, #13355, #51440, #98593, #36212, #82377, #29086, #21956, #13857, #7239, #83368, #75749, #61555, #62548, #29584, #46822, #14350, #15850, #6250, #22948, #31076, #84869, #62048, #69658, #39192, #93472, #31583, #92473, #68659, #85365, #44827, #92974, #61051, #38189, #23965, #8254, #70148, #37207, #76249, #52939, #635, #68159, #99085, #6745, #53938, #45816, #99576, #69147, #77738, #23449, #91479, #77239, #45328, #14851, #60561, #37699, #83870, #15350, #46314, #7746, #38692, #30082, #53440, #54432, #91983, #22454, #84370, #135, #76737, #100068, #30584, #63565, #71660, #79254, #71160, #24969, #64071, #32585, #87882, #16860, #64572, #94485, #9751, #56449, #3160, #70654, #25977, #18366, #63058, #95491, #10251, #72663, #48832, #33092, #55943, #2159, #86869, #10760, #1650, #47819, #33592, #55437, #1145, #49334, #86376, #80266, #47322, #94986, #2657, #87374, #41723, #48326, #40706, #34102, #79758, #17364, #72166, #25472, #17868, #41214, #95991, #56948, #65074, #54934, #85877, #8755, #78743, #93979, #16354, #78244, #9243, #39694, #32082, #24471, #40205, #96487, #66069, #26488, #11254, #88381, #97967, #27488, #80772, #81262, #3655, #58932, #4647, #66573, #81765, #58445, #20847, #73164, #59432, #96989, #36090, #13236, #43705, #82258, #50326, #26978, #12235, #42723, #74642, #75142, #89875, #51824, #42230, #57949, #88888, #57452, #11746, #34600, #82753, #18862, #89378, #44210, #36579, #65572, #50824, #5633, #67551, #43216, #74154, #19361, #35602, #19848, #73655, #97486, #27979, #28467, #20345, #49839, #4148, #35101, #51318, #12735, #5136, #67058, #90372, #53823, #76628, #21342, #52320, #99468, #53322, #84755, #15242, #46199, #21842, #84252, #22338, #99962, #46710, #13735, #69545, #30968, #6132, #7639, #77130, #15744, #92365, #7129, #77632, #37085, #28969, #14737, #98469, #90871, #38079, #8144, #44706, #61935, #29462, #92865, #83254, #69034, #38585, #30472, #23341, #91867, #45703, #54326, #39081, #61438, #83752, #25, #59943, #85251, #76135, #22836, #75631, #68048, #98972, #60445, #91366, #52817, #14232, #45208, #6632, #37586, #68538, #29967, #60936, #55830, #33470, #79641, #78127, #63959, #1026, #1535, #23852, #24361, #47208, #2043, #48214, #9639, #24856, #32475, #64461, #16247, #2538, #40091, #86757, #70539, #93360, #17246, #62434, #9133, #70035, #95375, #87258, #18251, #32984, #25863, #54826, #39587, #31977, #523, #55327, #85762, #56836, #31473, #86261, #56338, #62945, #8642, #94868, #93869, #79141, #16741, #47709, #40599, #78626, #71046, #63450, #87769, #17752, #49223, #25358, #80152, #94369, #71549, #48723, #10136, #41101, #72054, #10641, #3040, #26864, #27860, #3539, #18742, #74041, #65457, #4034, #51704, #89264, #11138, #34480, #35972, #82639, #11629, #90260, #41603, #57832, #28354, #58327, #49720, #20736, #97376, #19732, #64960, #26366, #95871, #42607, #96876, #58815, #89765, #20236, #96374, #27365, #65953, #33978, #72548, #51204, #34978, #80653, #74533, #97859, #50705, #59317, #35485, #81655, #57339, #42108, #88269, #12124, #73054, #88774, #43098, #19242, #50209, #5023, #81151, #82146, #12632, #73542, #4538, #66456, #43592, #66942, #69424, #92747, #61824, #91746, #98860, #15130, #13122, #61327, #91254, #68425, #23230, #75517, #54216, #6524, #92251, #29855, #83639, #44089, #75018, #36972, #22226, #76020, #29354, #99359, #77016, #22723, #21232, #7020, #44589, #45099, #67433, #37475, #100342, #5516, #36467, #30858, #21727, #46093, #60825, #98358, #60329, #7518, #28863, #14121, #53209, #68920, #99845, #30353, #67937, #84137, #14627, #59825, #90758, #53713, #45594, #52204, #38472, #83131, #76514, #13619, #37969, #84640, #6017, #52700, #15627, #9024, #85140, #77519, #63337, #64344, #31360, #48609, #408, #63842, #32868, #39476, #70936, #8019, #94755, #71434, #40983, #95262, #33355, #94254, #70429, #87148, #46595, #25244, #62836, #39972, #25752, #47098, #38969, #78517, #56218, #1424, #55218, #69922, #62324, #8526, #24739, #47600, #914, #32359, #79534, #17637, #93252, #79025, #16128, #16628, #23739, #54712, #17131, #55719, #86646, #48100, #9523, #10022, #85649, #71941, #86146, #2423, #78014, #1925, #40481, #31867, #93753, #24246, #72935, #35862, #12020, #89154, #51093, #10522, #26254, #18628, #87656, #11028, #41483, #82037, #56721, #96266, #12517, #66834, #95760, #81040, #43484, #97755, #73433, #26751, #3435, #49605, #74424, #18137, #57716, #35374, #49106, #34368, #80037, #50590, #64850, #57226, #88158, #65349, #3930, #11518, #88658, #42989, #19128, #80535, #89649, #73927, #4916, #81546, #34867, #50100, #65838, #42498, #72438, #96760, #41998, #66336, #27258, #2931, #58213, #20131, #33864, #97260, #4423, #19628, #27751, #58701, #21612, #14006, #61213, #22114, #29239, #45484, #67825, #29743, #60710, #69302, #52583, #7392, #28748, #90641, #38349, #83520, #6902, #44981, #98748, #52089, #28246, #53598, #44478, #53096, #98243, #60209, #59207, #13008, #90149, #99728, #91138, #75906, #75403, #6411, #84522, #20625, #51592, #45976, #5903, #22604, #74905, #92133, #37367, #37855, #15009, #76399, #84022, #83017, #59710, #68310, #36861, #82527, #14509, #43973, #99241, #91630, #68809, #30232, #76890, #13506, #5410, #36362, #67318, #21118, #25115, #9898, #38847, #24119, #56091, #79407, #16499, #70308, #46971, #78398, #70810, #1799, #8901, #30739, #48481, #77893, #40850, #94129, #7896, #69805, #31235, #8398, #47471, #55089, #16002, #788, #39847, #39349, #32735, #62203, #9396, #31740, #1299, #32232, #61705, #86023, #285, #23107, #63207, #92629, #62708, #100221, #63719, #17008, #54095, #24613, #94635, #85016, #93126, #23608, #15500, #54582, #46467, #87024, #77396, #85518, #86522, #93623, #55593, #47973, #78898, #40357, #71311, #17514, #41357, #64726, #66217, #12391, #41871, #50469, #50976, #18511, #81913, #65717, #79910, #20009, #27133, #49987, #95142, #56600, #25628, #72815, #26635, #58097, #89033, #19508, #95643, #57596, #96148, #73311, #71815, #87534, #42868, #4297, #10399, #27637, #34249, #2808, #80914, #10908, #19008, #3318, #58582, #88036, #33745, #81418, #72311, #33236, #11405, #35248, #18014, #11899, #73799, #26128, #88532, #97137, #65224, #42379, #89525, #96631, #3806, #2305, #34744, #64216, #48977, #57099, #49484, #80414, #43856, #5283, #53472, #36736, #21986, #60090, #13382, #67205, #85780, #68688, #59588, #37237, #12884, #82897, #43364, #28132, #4792, #14380, #44362, #75286, #90518, #5781, #99606, #35747, #74301, #61082, #20996, #91015, #22482, #51969, #6772, #67704, #37727, #90026, #76278, #98621, #52967, #30109, #60591, #99115, #98118, #74785, #29115, #21487, #66718, #29612, #97628, #92011, #59089, #36244, #28624, #20498, #52466, #51470, #82404, #83398, #13883, #44857, #75780, #6279, #68188, #91507, #83902, #45356, #63465, #40106, #9657, #33489, #49240, #94387, #79657, #18268, #71063, #16262, #25375, #24374, #55343, #16755, #24869, #40612, #17263, #1552, #55845, #71567, #32493, #2553, #47725, #78641, #48227, #79157, #63974, #47220, #31989, #64477, #95391, #86275, #1045, #9147, #39599, #86773, #2060, #32999, #94884, #56353, #56852, #87272, #17772, #48737, #78142, #93886, #25881, #10157, #87785, #70551, #41116, #72073, #8657, #62958, #100297, #92700, #39431, #363, #7467, #23690, #46054, #7973, #38925, #84599, #61780, #86100, #31822, #62791, #59396, #98438, #44176, #93706, #16579, #30307, #47554, #24197, #22682, #31311, #75109, #76973, #5105, #90343, #67030, #36549, #38427, #20816, #61285, #82724, #69879, #85096, #46544, #23188, #36055, #69378, #85595, #97938, #53668, #28433, #62280, #13200, #5605, #67517, #15087, #51789, #92208, #30815, #54174, #15580, #93205, #54665, #16082, #77474, #47052, #77966, #8481, #55173, #70380, #870, #10982, #86600, #32315, #78980, #70891, #9477, #95219, #96225, #17087, #8976, #2378, #78475, #1382, #56676, #57668, #24692, #41947, #40438, #72890, #63288, #18093, #26206, #79987, #3388, #71893, #34323, #88611, #26708, #87610, #63797, #80487, #39928, #57180, #56172, #33309, #19083, #65301, #94205, #55674, #71390, #48050, #1873, #32820, #94712, #25196, #49059, #40932, #87100, #64296, #17592, #88114, #48564, #72392, #79490, #9977, #25700, #10475, #41435, #2887, #33817, #64802, #95718, #18581, #49558, #96709, #66288, #13465, #4871, #50543, #73390, #35819, #42450, #89605, #50055, #82974, #67279, #98703, #82482, #44437, #3884, #19583, #11977, #80994, #4379, #34823, #67786, #11476, #35327, #36320, #42945, #27212, #12963, #73881, #12475, #60170, #97711, #81498, #97215, #75361, #65794, #29201, #91092, #27710, #36818, #66792, #89110, #58656, #20084, #28204, #74374, #51052, #81991, #59161, #43444, #5861, #90105, #59668, #20579, #51552, #43931, #58167, #74862, #98197, #5366, #28707, #90598, #21077, #52044, #33293, #1857, #2871, #24179, #16062, #9461, #85579, #77951, #63780, #64786, #31805, #49043, #16561, #18074, #8464, #25179, #64279, #10459, #78961, #71375, #79971, #79472, #86583, #2362, #24674, #87084, #17573, #26189, #40419, #95701, #86082, #47536, #47035, #32801, #95202, #94696, #55656, #8960, #39414, #41419, #1364, #9963, #55155, #17069, #70364, #849, #62774, #56656, #48035, #56155, #32298, #48545, #72376, #93690, #78459, #33803, #63271, #39908, #70874, #94188, #40913, #25685, #71876, #87594, #12455, #80975, #57653, #42927, #73370, #36304, #43426, #10967, #34806, #73863, #65779, #74358, #4851, #11462, #41932, #82467, #57162, #96693, #12945, #67263, #96209, #81482, #43915, #98183, #4363, #27196, #3868, #35311, #27695, #59146, #66273, #89091, #72874, #19568, #74845, #18568, #88100, #5349, #58151, #90086, #97196, #49543, #50526, #20562, #11956, #88596, #80472, #58640, #3375, #89588, #34306, #51532, #35803, #65285, #20069, #51032, #81975, #66776, #97693, #28189, #26694, #42435, #19068, #50042, #13946, #14940, #91075, #5845, #61148, #52524, #91570, #38783, #76337, #6834, #99664, #30675, #37793, #59650, #77333, #69744, #44922, #15441, #45415, #36800, #7833, #84457, #68746, #52028, #13447, #82956, #29679, #83963, #45913, #21552, #38282, #37302, #30169, #92071, #90580, #28685, #76827, #22051, #67762, #61646, #21058, #6342, #44422, #7327, #22542, #46401, #98684, #75344, #53033, #83458, #69238, #29178, #60154, #53533, #92564, #75845, #100156, #23036, #68249, #14443, #99177, #54030, #84955, #60650, #79842, #48915, #78828, #85962, #2241, #32673, #41292, #94068, #10340, #719, #62639, #225, #24554, #79342, #16948, #70742, #31166, #62136, #24052, #9329, #63142, #16438, #86460, #64153, #9836, #93061, #71748, #1237, #23541, #47406, #54519, #94571, #8335, #39281, #31669, #8838, #47908, #55528, #78335, #32169, #40292, #39776, #33173, #93558, #40789, #71245, #1734, #63646, #85451, #15938, #95078, #25562, #70240, #56532, #25054, #46904, #55023, #56030, #86958, #17445, #48412, #87463, #17954, #77828, #52278, #52781, #18451, #37047, #3250, #6094, #64662, #13193, #21307, #75101, #98938, #65655, #58033, #68007, #67509, #73247, #90834, #11342, #5598, #36542, #14195, #27070, #83717, #29425, #60407, #26063, #65160, #10845, #91328, #72251, #96081, #2742, #21804, #88470, #98430, #41808, #42317, #33682, #57034, #95574, #44672, #3741, #87969, #26574, #49423, #28934, #51781, #44168, #90333, #34683, #80348, #72754, #34185, #96568, #83214, #57536, #13697, #59903, #18944, #49925, #20809, #80856, #75591, #82716, #22797, #61897, #53783, #62392, #93323, #15204, #30929, #99920, #62908, #6596, #30431, #31433, #7094, #22303, #77592, #68996, #7593, #46164, #92324, #23304, #15705, #47170, #54289, #76095, #68500, #77094, #100418, #479, #23813, #54786, #61401, #92822, #69501, #46669, #93831, #60900, #16203, #84209, #78089, #37549, #84713, #91826, #85721, #85217, #24317, #14700, #99434, #8096, #45173, #29929, #39045, #55290, #53281, #8601, #76590, #39548, #45665, #38545, #69993, #38043, #70500, #989, #31938, #86220, #65415, #95333, #1994, #18693, #16703, #64915, #94828, #72012, #96330, #42063, #73008, #71007, #9597, #33431, #87216, #26818, #57783, #40557, #25821, #79604, #32940, #2493, #80602, #26323, #24811, #10592, #48170, #48680, #1497, #71509, #94326, #49181, #56793, #34436, #25318, #49675, #64416, #47671, #63914, #11094, #87727, #17205, #40049, #18209, #9095, #56294, #78585, #3495, #33936, #32434, #80105, #63408, #55792, #95828, #57297, #17710, #41559, #10094, #86715, #79098, #41053, #3000, #72507, #88229, #20690, #12079, #51156, #98814, #35926, #58282, #81608, #83083, #29308, #19196, #36922, #88727, #73999, #75468, #4979, #65910, #67891, #44041, #66897, #11585, #73494, #43052, #89221, #74486, #4492, #50167, #74972, #42562, #66408, #3989, #19689, #50660, #81104, #35439, #34932, #13574, #96825, #27816, #44543, #27321, #97328, #12586, #5972, #58769, #97819, #89721, #20191, #28312, #59268, #82105, #43549, #67387, #90216, #51661, #82598, #13074, #5475, #36423, #98311, #28814, #59780, #90713, #21188, #52154, #69372, #37923, #93199, #22180, #69874, #15081, #84592, #61775, #8475, #75970, #31305, #23685, #68380, #54659, #38421, #91204, #99313, #100292, #99795, #7462, #30302, #16076, #76469, #53163, #38920, #39425, #6478, #85589, #91696, #47046, #52651, #30810, #7967, #92694, #77961, #53663, #46048, #70375, #54168, #61279, #77467, #92202, #23181, #85090, #864, #76967, #60281, #21679, #83587, #14074, #84092, #29806, #45051, #37430, #14578, #60777, #45548, #6974, #15575, #68871, #22677, #46539, #357, #62274, #2882, #63791, #86095, #86595, #8970, #64291, #9972, #71888, #87095, #94707, #26201, #78470, #64796, #1868, #41428, #18577, #49053, #87605 ),
 .UNSPECIFIED., .F., .F.,
 ( 4, 2, 2, 2, 2, 2, 2, 2, 2, 2, 2, 2, 2, 2, 2, 2, 2, 2, 2, 2, 2, 2, 2, 2, 2, 2, 2, 2, 2, 2, 2, 2, 2, 2, 2, 2, 2, 2, 2, 2, 2, 2, 2, 2, 2, 2, 2, 2, 2, 2, 2, 2, 2, 2, 2, 2, 2, 2, 2, 2, 2, 2, 2, 2, 2, 2, 2, 2, 2, 2, 2, 2, 2, 2, 2, 2, 2, 2, 2, 2, 2, 2, 2, 2, 2, 2, 2, 2, 2, 2, 2, 2, 2, 2, 2, 2, 2, 2, 2, 2, 2, 2, 2, 2, 2, 2, 2, 2, 2, 2, 2, 2, 2, 2, 2, 2, 2, 2, 2, 2, 2, 2, 2, 2, 2, 2, 2, 2, 2, 2, 2, 2, 2, 2, 2, 2, 2, 2, 2, 2, 2, 2, 2, 2, 2, 2, 2, 2, 2, 2, 2, 2, 2, 2, 2, 2, 2, 2, 2, 2, 2, 2, 2, 2, 2, 2, 2, 2, 2, 2, 2, 2, 2, 2, 2, 2, 2, 2, 2, 2, 2, 2, 2, 2, 2, 2, 2, 2, 2, 2, 2, 2, 2, 2, 2, 2, 2, 2, 2, 2, 2, 2, 2, 2, 2, 2, 2, 2, 2, 2, 2, 2, 2, 2, 2, 2, 2, 2, 2, 2, 2, 2, 2, 2, 2, 2, 2, 2, 2, 2, 2, 2, 2, 2, 2, 2, 2, 2, 2, 2, 2, 2, 2, 2, 2, 2, 2, 2, 2, 2, 2, 2, 2, 2, 2, 2, 2, 2, 2, 2, 2, 2, 2, 2, 2, 2, 2, 2, 2, 2, 2, 2, 2, 2, 2, 2, 2, 2, 2, 2, 2, 2, 2, 2, 2, 2, 2, 2, 2, 2, 2, 2, 2, 2, 2, 2, 2, 2, 2, 2, 2, 2, 2, 2, 2, 2, 2, 2, 2, 2, 2, 2, 2, 2, 2, 2, 2, 2, 2, 2, 2, 2, 2, 2, 2, 2, 2, 2, 2, 2, 2, 2, 2, 2, 2, 2, 2, 2, 2, 2, 2, 2, 2, 2, 2, 2, 2, 2, 2, 2, 2, 2, 2, 2, 2, 2, 2, 2, 2, 2, 2, 2, 2, 2, 2, 2, 2, 2, 2, 2, 2, 2, 2, 2, 2, 2, 2, 2, 2, 2, 2, 2, 2, 2, 2, 2, 2, 2, 2, 2, 2, 2, 2, 2, 2, 2, 2, 2, 2, 2, 2, 2, 2, 2, 2, 2, 2, 2, 2, 2, 2, 2, 2, 2, 2, 2, 2, 2, 2, 2, 2, 2, 2, 2, 2, 2, 2, 2, 2, 2, 2, 2, 2, 2, 2, 2, 2, 2, 2, 2, 2, 2, 2, 2, 2, 2, 2, 2, 2, 2, 2, 2, 2, 2, 2, 2, 2, 2, 2, 2, 2, 2, 2, 2, 2, 2, 2, 2, 2, 2, 2, 2, 2, 2, 2, 2, 2, 2, 2, 2, 2, 2, 2, 2, 2, 2, 2, 2, 2, 2, 2, 2, 2, 2, 2, 2, 2, 2, 2, 2, 2, 2, 2, 2, 2, 2, 2, 2, 2, 2, 2, 2, 2, 2, 2, 2, 2, 2, 2, 2, 2, 2, 2, 2, 2, 2, 2, 2, 2, 2, 2, 2, 2, 2, 2, 2, 2, 2, 2, 2, 2, 2, 2, 2, 2, 2, 2, 2, 2, 2, 2, 2, 2, 2, 2, 2, 2, 2, 2, 2, 2, 2, 2, 2, 2, 2, 2, 2, 2, 2, 2, 2, 2, 2, 2, 2, 2, 2, 2, 2, 2, 2, 2, 2, 2, 2, 2, 2, 2, 2, 2, 2, 2, 2, 2, 2, 2, 2, 2, 2, 2, 2, 2, 2, 2, 2, 2, 2, 2, 2, 2, 2, 2, 2, 2, 2, 2, 2, 2, 2, 2, 2, 2, 2, 2, 2, 2, 2, 2, 2, 2, 2, 2, 2, 2, 2, 2, 2, 2, 2, 2, 2, 2, 2, 2, 2, 2, 2, 2, 2, 2, 2, 2, 2, 2, 2, 2, 2, 2, 2, 2, 2, 2, 2, 2, 2, 2, 2, 2, 2, 2, 2, 2, 2, 2, 2, 2, 2, 2, 2, 2, 2, 2, 2, 2, 2, 2, 2, 2, 2, 2, 2, 2, 2, 2, 2, 2, 2, 2, 2, 2, 2, 2, 2, 2, 2, 2, 2, 2, 2, 2, 2, 2, 2, 2, 2, 2, 2, 2, 2, 2, 2, 2, 2, 2, 2, 2, 2, 2, 2, 2, 2, 2, 2, 2, 2, 2, 2, 2, 2, 2, 2, 2, 2, 2, 2, 2, 2, 2, 2, 2, 2, 2, 2, 2, 2, 2, 2, 2, 2, 2, 2, 2, 2, 2, 2, 2, 2, 2, 2, 2, 2, 2, 2, 2, 2, 2, 2, 2, 2, 2, 2, 2, 2, 2, 2, 2, 2, 2, 2, 2, 2, 2, 2, 2, 2, 2, 2, 2, 2, 2, 2, 2, 2, 2, 2, 2, 2, 2, 2, 2, 2, 2, 2, 2, 2, 2, 2, 2, 2, 2, 2, 2, 2, 2, 2, 2, 2, 2, 2, 2, 2, 2, 2, 2, 2, 2, 2, 2, 2, 2, 2, 2, 2, 2, 2, 2, 2, 2, 2, 2, 2, 2, 2, 2, 2, 2, 2, 2, 2, 2, 2, 2, 2, 2, 2, 2, 2, 2, 2, 2, 2, 2, 2, 2, 2, 2, 2, 2, 2, 2, 2, 2, 2, 2, 2, 2, 2, 2, 2, 2, 2, 2, 2, 2, 2, 2, 2, 2, 2, 2, 2, 2, 2, 2, 2, 2, 2, 2, 2, 2, 2, 2, 2, 2, 2, 2, 2, 2, 2, 2, 2, 2, 2, 2, 2, 2, 2, 2, 2, 2, 2, 2, 2, 2, 2, 2, 2, 2, 2, 2, 2, 2, 2, 2, 2, 2, 2, 2, 2, 2, 2, 2, 2, 2, 2, 2, 2, 2, 2, 2, 2, 2, 2, 2, 2, 2, 2, 2, 2, 2, 2, 2, 2, 2, 2, 2, 2, 2, 2, 2, 2, 2, 2, 2, 2, 2, 2, 2, 2, 2, 2, 2, 2, 2, 2, 2, 2, 2, 2, 2, 2, 2, 2, 2, 2, 2, 2, 2, 2, 2, 2, 2, 2, 2, 2, 2, 2, 2, 2, 2, 2, 2, 2, 2, 2, 2, 2, 2, 2, 2, 2, 2, 2, 2, 2, 2, 2, 2, 2, 2, 2, 2, 2, 2, 2, 2, 2, 2, 2, 2, 2, 2, 2, 2, 2, 2, 2, 2, 2, 2, 2, 2, 2, 2, 2, 2, 2, 2, 2, 2, 2, 2, 2, 2, 2, 2, 2, 2, 2, 2, 2, 2, 2, 2, 2, 2, 2, 2, 2, 2, 2, 2, 2, 2, 2, 2, 2, 2, 2, 2, 2, 2, 2, 2, 2, 2, 2, 2, 2, 2, 2, 2, 2, 2, 2, 2, 2, 2, 2, 2, 2, 2, 2, 2, 2, 2, 2, 2, 2, 2, 2, 2, 2, 2, 2, 2, 2, 2, 2, 2, 2, 2, 2, 2, 2, 2, 2, 2, 2, 2, 2, 2, 2, 2, 2, 2, 2, 2, 2, 2, 2, 2, 2, 2, 2, 2, 2, 2, 2, 2, 2, 2, 2, 2, 2, 2, 2, 2, 2, 2, 2, 2, 2, 2, 2, 2, 2, 2, 2, 2, 2, 2, 2, 2, 2, 2, 2, 2, 2, 2, 2, 2, 2, 2, 2, 2, 2, 2, 2, 2, 2, 2, 2, 2, 2, 2, 2, 2, 2, 2, 2, 2, 2, 2, 2, 2, 2, 2, 2, 2, 2, 2, 2, 2, 2, 2, 2, 2, 2, 2, 2, 2, 2, 2, 2, 2, 2, 2, 2, 2, 2, 2, 2, 2, 2, 2, 2, 2, 2, 2, 2, 2, 2, 2, 2, 2, 2, 2, 2, 2, 2, 2, 2, 2, 2, 2, 2, 2, 2, 2, 2, 2, 2, 2, 2, 2, 2, 2, 2, 2, 2, 2, 2, 2, 2, 2, 2, 2, 2, 2, 2, 2, 2, 2, 2, 2, 2, 2, 2, 2, 2, 2, 2, 2, 2, 2, 2, 2, 2, 2, 2, 2, 2, 2, 2, 2, 2, 2, 2, 2, 2, 2, 2, 2, 2, 2, 2, 2, 2, 2, 2, 2, 2, 2, 2, 2, 2, 2, 2, 2, 2, 2, 2, 2, 2, 2, 2, 2, 2, 2, 2, 2, 2, 2, 2, 2, 2, 2, 2, 2, 2, 2, 2, 2, 2, 2, 2, 2, 2, 2, 2, 2, 2, 2, 2, 2, 2, 2, 2, 2, 2, 2, 2, 2, 2, 2, 2, 2, 2, 2, 2, 2, 2, 2, 2, 2, 2, 2, 2, 2, 2, 2, 2, 2, 2, 2, 2, 2, 2, 2, 2, 2, 2, 2, 2, 2, 2, 2, 2, 2, 2, 2, 2, 2, 2, 2, 2, 2, 2, 2, 2, 2, 2, 2, 2, 2, 2, 2, 2, 2, 2, 2, 2, 2, 2, 2, 2, 2, 2, 2, 2, 2, 2, 2, 2, 2, 2, 2, 2, 2, 2, 2, 2, 2, 2, 2, 2, 2, 2, 2, 2, 2, 2, 2, 2, 2, 2, 2, 2, 2, 2, 2, 2, 2, 2, 2, 2, 2, 2, 2, 2, 2, 2, 2, 2, 2, 2, 2, 2, 2, 2, 2, 2, 2, 2, 2, 2, 2, 2, 2, 2, 2, 2, 2, 2, 2, 2, 2, 2, 2, 2, 2, 2, 2, 2, 2, 2, 2, 2, 2, 2, 2, 2, 2, 2, 2, 2, 2, 2, 2, 2, 2, 2, 2, 2, 2, 2, 2, 2, 2, 2, 2, 2, 2, 2, 2, 2, 2, 2, 2, 2, 2, 2, 2, 2, 2, 2, 2, 2, 2, 2, 2, 2, 2, 2, 2, 2, 2, 2, 2, 2, 2, 2, 2, 2, 2, 2, 2, 2, 2, 2, 2, 2, 2, 2, 2, 2, 2, 2, 2, 2, 2, 2, 2, 2, 2, 2, 2, 2, 2, 2, 2, 2, 2, 2, 2, 2, 2, 2, 2, 2, 2, 2, 2, 2, 2, 2, 2, 2, 2, 2, 2, 2, 2, 2, 2, 2, 2, 2, 2, 2, 2, 2, 2, 2, 2, 2, 2, 2, 2, 2, 2, 2, 2, 2, 2, 2, 2, 2, 2, 2, 2, 2, 2, 2, 2, 2, 2, 2, 2, 2, 2, 2, 2, 2, 2, 2, 2, 2, 2, 2, 2, 2, 2, 2, 2, 2, 2, 2, 2, 2, 2, 2, 2, 2, 2, 2, 2, 2, 2, 2, 2, 2, 2, 2, 2, 2, 2, 2, 2, 2, 2, 2, 2, 2, 2, 2, 2, 2, 2, 2, 2, 2, 2, 2, 2, 2, 2, 2, 2, 2, 2, 2, 2, 2, 2, 2, 2, 2, 2, 2, 2, 2, 2, 2, 2, 2, 2, 2, 2, 2, 2, 2, 2, 2, 2, 2, 2, 2, 2, 2, 2, 2, 2, 2, 2, 2, 2, 2, 2, 2, 2, 2, 2, 2, 2, 2, 2, 2, 2, 2, 2, 2, 2, 2, 2, 2, 2, 2, 2, 2, 2, 2, 2, 2, 2, 2, 2, 2, 2, 2, 2, 2, 2, 2, 2, 2, 2, 2, 2, 2, 2, 2, 2, 2, 2, 2, 2, 2, 2, 2, 2, 2, 2, 2, 2, 2, 2, 2, 2, 2, 2, 2, 2, 2, 2, 2, 2, 2, 2, 2, 2, 2, 2, 2, 2, 2, 2, 2, 2, 2, 2, 2, 2, 2, 2, 2, 2, 2, 2, 2, 2, 2, 2, 2, 2, 2, 2, 2, 2, 2, 2, 2, 2, 2, 2, 2, 2, 2, 2, 2, 2, 2, 2, 2, 2, 2, 2, 2, 2, 2, 2, 2, 2, 2, 2, 2, 2, 2, 2, 2, 2, 2, 2, 2, 2, 2, 2, 2, 2, 2, 2, 2, 2, 2, 2, 2, 2, 2, 2, 2, 2, 2, 2, 2, 2, 2, 2, 2, 2, 2, 2, 2, 2, 2, 2, 2, 2, 2, 2, 2, 2, 2, 2, 2, 2, 2, 2, 2, 2, 2, 2, 2, 2, 2, 2, 2, 2, 2, 2, 2, 2, 2, 2, 2, 2, 2, 2, 2, 2, 2, 2, 2, 2, 2, 2, 2, 2, 2, 2, 2, 2, 2, 2, 2, 2, 2, 2, 2, 2, 2, 2, 2, 2, 2, 2, 2, 2, 2, 2, 2, 2, 2, 2, 2, 2, 2, 2, 2, 2, 2, 2, 2, 2, 2, 2, 2, 2, 2, 2, 2, 2, 2, 2, 2, 2, 2, 2, 2, 2, 2, 2, 2, 2, 2, 2, 2, 4 ),
 ( 0.000000000000000000, 0.0004882812500000001084, 0.0009765625000000002168, 0.001464843750000000434, 0.001953125000000000000, 0.002441406250000000000, 0.002929687499999999566, 0.003417968749999999566, 0.003906249999999999133, 0.004394531249999998265, 0.004882812499999997398, 0.005371093749999997398, 0.005859374999999997398, 0.006347656249999998265, 0.006835937499999998265, 0.007324218749999998265, 0.007812499999999998265, 0.008300781249999998265, 0.008789062499999998265, 0.009277343749999998265, 0.009765624999999998265, 0.01025390624999999827, 0.01074218749999999827, 0.01123046874999999827, 0.01171874999999999827, 0.01220703125000000000, 0.01269531250000000000, 0.01318359375000000000, 0.01367187500000000000, 0.01416015625000000000, 0.01464843750000000000, 0.01513671875000000000, 0.01562500000000000000, 0.01611328125000000000, 0.01660156250000000000, 0.01708984375000000000, 0.01757812500000000000, 0.01806640625000000000, 0.01855468750000000000, 0.01904296875000000000, 0.01953125000000000000, 0.02001953125000000000, 0.02050781250000000000, 0.02099609375000000000, 0.02148437500000000000, 0.02197265625000000000, 0.02246093750000000000, 0.02294921875000000000, 0.02343750000000000000, 0.02392578125000000347, 0.02441406250000000347, 0.02490234375000000347, 0.02539062500000000347, 0.02587890625000000347, 0.02636718750000000347, 0.02685546875000000347, 0.02734375000000000347, 0.02783203125000000347, 0.02832031250000000347, 0.02880859375000000347, 0.02929687500000000347, 0.02978515625000000347, 0.03027343750000000347, 0.03076171875000000347, 0.03125000000000000000, 0.03173828125000000000, 0.03222656250000000000, 0.03271484375000000000, 0.03320312500000000000, 0.03369140625000000000, 0.03417968750000000000, 0.03466796875000000000, 0.03515625000000000000, 0.03564453125000000000, 0.03613281250000000000, 0.03662109375000000000, 0.03710937500000000000, 0.03759765625000000000, 0.03808593750000000000, 0.03857421875000000000, 0.03906250000000000000, 0.03955078125000000000, 0.04003906250000000000, 0.04052734375000000000, 0.04101562500000000000, 0.04150390625000000000, 0.04199218750000000000, 0.04248046875000000000, 0.04296875000000000000, 0.04345703125000000000, 0.04394531250000000000, 0.04443359375000000000, 0.04492187500000000000, 0.04541015625000000000, 0.04589843750000000000, 0.04638671875000000000, 0.04687500000000000000, 0.04736328125000000694, 0.04785156250000000694, 0.04833984375000000694, 0.04882812500000000694, 0.04931640625000000694, 0.04980468750000000694, 0.05029296875000000694, 0.05078125000000000694, 0.05126953125000000694, 0.05175781250000000694, 0.05224609375000000694, 0.05273437500000000694, 0.05322265625000000694, 0.05371093750000000694, 0.05419921875000000694, 0.05468750000000000694, 0.05517578125000000694, 0.05566406250000000694, 0.05615234375000000694, 0.05664062500000000694, 0.05712890625000000694, 0.05761718750000000694, 0.05810546875000000694, 0.05859375000000000694, 0.05908203125000000694, 0.05957031250000000694, 0.06005859375000000694, 0.06054687500000000694, 0.06103515625000000694, 0.06152343750000000694, 0.06201171875000000694, 0.06250000000000000000, 0.06298828125000000000, 0.06347656250000000000, 0.06396484375000000000, 0.06445312500000000000, 0.06494140625000000000, 0.06542968750000000000, 0.06591796875000000000, 0.06640625000000000000, 0.06689453125000000000, 0.06738281250000000000, 0.06787109375000000000, 0.06835937500000000000, 0.06884765625000000000, 0.06933593750000000000, 0.06982421875000000000, 0.07031250000000000000, 0.07080078125000000000, 0.07128906250000000000, 0.07177734375000000000, 0.07226562500000000000, 0.07275390625000000000, 0.07324218750000000000, 0.07373046875000000000, 0.07421875000000000000, 0.07470703125000000000, 0.07519531250000000000, 0.07568359375000000000, 0.07617187500000000000, 0.07666015625000000000, 0.07714843750000000000, 0.07763671875000000000, 0.07812500000000000000, 0.07861328125000000000, 0.07910156250000000000, 0.07958984375000000000, 0.08007812500000000000, 0.08056640625000000000, 0.08105468750000000000, 0.08154296875000000000, 0.08203125000000000000, 0.08251953125000000000, 0.08300781250000000000, 0.08349609375000000000, 0.08398437500000000000, 0.08447265625000000000, 0.08496093750000000000, 0.08544921875000000000, 0.08593750000000000000, 0.08642578125000000000, 0.08691406250000000000, 0.08740234375000000000, 0.08789062500000000000, 0.08837890625000000000, 0.08886718750000000000, 0.08935546875000000000, 0.08984375000000000000, 0.09033203125000000000, 0.09082031250000000000, 0.09130859375000000000, 0.09179687500000000000, 0.09228515625000000000, 0.09277343750000000000, 0.09326171875000000000, 0.09375000000000000000, 0.09423828125000001388, 0.09472656250000001388, 0.09521484375000001388, 0.09570312500000001388, 0.09619140625000001388, 0.09667968750000001388, 0.09716796875000001388, 0.09765625000000001388, 0.09814453125000001388, 0.09863281250000001388, 0.09912109375000001388, 0.09960937500000001388, 0.1000976562500000139, 0.1005859375000000139, 0.1010742187500000139, 0.1015625000000000139, 0.1020507812500000139, 0.1025390625000000139, 0.1030273437500000139, 0.1035156250000000139, 0.1040039062500000139, 0.1044921875000000139, 0.1049804687500000139, 0.1054687500000000139, 0.1059570312500000139, 0.1064453125000000139, 0.1069335937500000139, 0.1074218750000000139, 0.1079101562500000139, 0.1083984375000000139, 0.1088867187500000139, 0.1093750000000000139, 0.1098632812500000139, 0.1103515625000000139, 0.1108398437500000139, 0.1113281250000000139, 0.1118164062500000139, 0.1123046875000000139, 0.1127929687500000139, 0.1132812500000000139, 0.1137695312500000139, 0.1142578125000000139, 0.1147460937500000139, 0.1152343750000000139, 0.1157226562500000139, 0.1162109375000000139, 0.1166992187500000139, 0.1171875000000000139, 0.1176757812500000139, 0.1181640625000000139, 0.1186523437500000139, 0.1191406250000000139, 0.1196289062500000139, 0.1201171875000000139, 0.1206054687500000139, 0.1210937500000000139, 0.1215820312500000139, 0.1220703125000000139, 0.1225585937500000139, 0.1230468750000000139, 0.1235351562500000139, 0.1240234375000000139, 0.1245117187500000139, 0.1250000000000000000, 0.1254882812500000000, 0.1259765625000000000, 0.1264648437500000000, 0.1269531250000000000, 0.1274414062500000000, 0.1279296875000000000, 0.1284179687500000000, 0.1289062500000000000, 0.1293945312500000000, 0.1298828125000000000, 0.1303710937500000000, 0.1308593750000000000, 0.1313476562500000000, 0.1318359375000000000, 0.1323242187500000000, 0.1328125000000000000, 0.1333007812500000000, 0.1337890625000000000, 0.1342773437500000000, 0.1347656250000000000, 0.1352539062500000000, 0.1357421875000000000, 0.1362304687500000000, 0.1367187500000000000, 0.1372070312500000000, 0.1376953125000000000, 0.1381835937500000000, 0.1386718750000000000, 0.1391601562500000000, 0.1396484375000000000, 0.1401367187500000000, 0.1406250000000000000, 0.1411132812500000000, 0.1416015625000000000, 0.1420898437500000000, 0.1425781250000000000, 0.1430664062500000000, 0.1435546875000000000, 0.1440429687500000000, 0.1445312500000000000, 0.1450195312500000000, 0.1455078125000000000, 0.1459960937500000000, 0.1464843750000000000, 0.1469726562500000000, 0.1474609375000000000, 0.1479492187500000000, 0.1484375000000000000, 0.1489257812500000000, 0.1494140625000000000, 0.1499023437500000000, 0.1503906250000000000, 0.1508789062500000000, 0.1513671875000000000, 0.1518554687500000000, 0.1523437500000000000, 0.1528320312500000000, 0.1533203125000000000, 0.1538085937500000000, 0.1542968750000000000, 0.1547851562500000000, 0.1552734375000000000, 0.1557617187500000000, 0.1562500000000000000, 0.1567382812500000000, 0.1572265625000000000, 0.1577148437500000000, 0.1582031250000000000, 0.1586914062500000000, 0.1591796875000000000, 0.1596679687500000000, 0.1601562500000000000, 0.1606445312500000000, 0.1611328125000000000, 0.1616210937500000000, 0.1621093750000000000, 0.1625976562500000000, 0.1630859375000000000, 0.1635742187500000000, 0.1640625000000000000, 0.1645507812500000000, 0.1650390625000000000, 0.1655273437500000000, 0.1660156250000000000, 0.1665039062500000000, 0.1669921875000000000, 0.1674804687500000000, 0.1679687500000000000, 0.1684570312500000000, 0.1689453125000000000, 0.1694335937500000000, 0.1699218750000000000, 0.1704101562500000000, 0.1708984375000000000, 0.1713867187500000000, 0.1718750000000000000, 0.1723632812500000000, 0.1728515625000000000, 0.1733398437500000000, 0.1738281250000000000, 0.1743164062500000000, 0.1748046875000000000, 0.1752929687500000000, 0.1757812500000000000, 0.1762695312500000000, 0.1767578125000000000, 0.1772460937500000000, 0.1777343750000000000, 0.1782226562500000000, 0.1787109375000000000, 0.1791992187500000000, 0.1796875000000000000, 0.1801757812500000000, 0.1806640625000000000, 0.1811523437500000000, 0.1816406250000000000, 0.1821289062500000000, 0.1826171875000000000, 0.1831054687500000000, 0.1835937500000000000, 0.1840820312500000000, 0.1845703125000000000, 0.1850585937500000000, 0.1855468750000000000, 0.1860351562500000000, 0.1865234375000000000, 0.1870117187500000000, 0.1875000000000000000, 0.1879882812500000278, 0.1884765625000000278, 0.1889648437500000278, 0.1894531250000000278, 0.1899414062500000278, 0.1904296875000000278, 0.1909179687500000278, 0.1914062500000000278, 0.1918945312500000278, 0.1923828125000000278, 0.1928710937500000278, 0.1933593750000000278, 0.1938476562500000278, 0.1943359375000000278, 0.1948242187500000278, 0.1953125000000000278, 0.1958007812500000278, 0.1962890625000000278, 0.1967773437500000278, 0.1972656250000000278, 0.1977539062500000278, 0.1982421875000000278, 0.1987304687500000278, 0.1992187500000000278, 0.1997070312500000278, 0.2001953125000000278, 0.2006835937500000278, 0.2011718750000000278, 0.2016601562500000278, 0.2021484375000000278, 0.2026367187500000278, 0.2031250000000000278, 0.2036132812500000278, 0.2041015625000000278, 0.2045898437500000278, 0.2050781250000000278, 0.2055664062500000278, 0.2060546875000000278, 0.2065429687500000278, 0.2070312500000000278, 0.2075195312500000278, 0.2080078125000000278, 0.2084960937500000278, 0.2089843750000000278, 0.2094726562500000278, 0.2099609375000000278, 0.2104492187500000278, 0.2109375000000000278, 0.2114257812500000278, 0.2119140625000000278, 0.2124023437500000278, 0.2128906250000000278, 0.2133789062500000278, 0.2138671875000000278, 0.2143554687500000278, 0.2148437500000000278, 0.2153320312500000278, 0.2158203125000000278, 0.2163085937500000278, 0.2167968750000000278, 0.2172851562500000278, 0.2177734375000000278, 0.2182617187500000278, 0.2187500000000000278, 0.2192382812500000278, 0.2197265625000000278, 0.2202148437500000278, 0.2207031250000000278, 0.2211914062500000278, 0.2216796875000000278, 0.2221679687500000278, 0.2226562500000000278, 0.2231445312500000278, 0.2236328125000000278, 0.2241210937500000278, 0.2246093750000000278, 0.2250976562500000278, 0.2255859375000000278, 0.2260742187500000278, 0.2265625000000000278, 0.2270507812500000278, 0.2275390625000000278, 0.2280273437500000278, 0.2285156250000000278, 0.2290039062500000278, 0.2294921875000000278, 0.2299804687500000278, 0.2304687500000000278, 0.2309570312500000278, 0.2314453125000000278, 0.2319335937500000278, 0.2324218750000000278, 0.2329101562500000278, 0.2333984375000000278, 0.2338867187500000278, 0.2343750000000000278, 0.2348632812500000278, 0.2353515625000000278, 0.2358398437500000278, 0.2363281250000000278, 0.2368164062500000278, 0.2373046875000000278, 0.2377929687500000278, 0.2382812500000000278, 0.2387695312500000278, 0.2392578125000000278, 0.2397460937500000278, 0.2402343750000000278, 0.2407226562500000278, 0.2412109375000000278, 0.2416992187500000278, 0.2421875000000000278, 0.2426757812500000278, 0.2431640625000000278, 0.2436523437500000278, 0.2441406250000000278, 0.2446289062500000278, 0.2451171875000000278, 0.2456054687500000278, 0.2460937500000000278, 0.2465820312500000278, 0.2470703125000000278, 0.2475585937500000278, 0.2480468750000000278, 0.2485351562500000278, 0.2490234375000000278, 0.2495117187500000278, 0.2500000000000000000, 0.2504882812500000000, 0.2509765625000000000, 0.2514648437500000000, 0.2519531250000000000, 0.2524414062500000000, 0.2529296875000000000, 0.2534179687500000000, 0.2539062500000000000, 0.2543945312500000000, 0.2548828125000000000, 0.2553710937500000000, 0.2558593750000000000, 0.2563476562500000000, 0.2568359375000000000, 0.2573242187500000000, 0.2578125000000000000, 0.2583007812500000000, 0.2587890625000000000, 0.2592773437500000000, 0.2597656250000000000, 0.2602539062500000000, 0.2607421875000000000, 0.2612304687500000000, 0.2617187500000000000, 0.2622070312500000000, 0.2626953125000000000, 0.2631835937500000000, 0.2636718750000000000, 0.2641601562500000000, 0.2646484375000000000, 0.2651367187500000000, 0.2656250000000000000, 0.2661132812500000000, 0.2666015625000000000, 0.2670898437500000000, 0.2675781250000000000, 0.2680664062500000000, 0.2685546875000000000, 0.2690429687500000000, 0.2695312500000000000, 0.2700195312500000000, 0.2705078125000000000, 0.2709960937500000000, 0.2714843750000000000, 0.2719726562500000000, 0.2724609375000000000, 0.2729492187500000000, 0.2734375000000000000, 0.2739257812500000000, 0.2744140625000000000, 0.2749023437500000000, 0.2753906250000000000, 0.2758789062500000000, 0.2763671875000000000, 0.2768554687500000000, 0.2773437500000000000, 0.2778320312500000000, 0.2783203125000000000, 0.2788085937500000000, 0.2792968750000000000, 0.2797851562500000000, 0.2802734375000000000, 0.2807617187500000000, 0.2812500000000000000, 0.2817382812500000000, 0.2822265625000000000, 0.2827148437500000000, 0.2832031250000000000, 0.2836914062500000000, 0.2841796875000000000, 0.2846679687500000000, 0.2851562500000000000, 0.2856445312500000000, 0.2861328125000000000, 0.2866210937500000000, 0.2871093750000000000, 0.2875976562500000000, 0.2880859375000000000, 0.2885742187500000000, 0.2890625000000000000, 0.2895507812500000000, 0.2900390625000000000, 0.2905273437500000000, 0.2910156250000000000, 0.2915039062500000000, 0.2919921875000000000, 0.2924804687500000000, 0.2929687500000000000, 0.2934570312500000000, 0.2939453125000000000, 0.2944335937500000000, 0.2949218750000000000, 0.2954101562500000000, 0.2958984375000000000, 0.2963867187500000000, 0.2968750000000000000, 0.2973632812500000000, 0.2978515625000000000, 0.2983398437500000000, 0.2988281250000000000, 0.2993164062500000000, 0.2998046875000000000, 0.3002929687500000000, 0.3007812500000000000, 0.3012695312500000000, 0.3017578125000000000, 0.3022460937500000000, 0.3027343750000000000, 0.3032226562500000000, 0.3037109375000000000, 0.3041992187500000000, 0.3046875000000000000, 0.3051757812500000000, 0.3056640625000000000, 0.3061523437500000000, 0.3066406250000000000, 0.3071289062500000000, 0.3076171875000000000, 0.3081054687500000000, 0.3085937500000000000, 0.3090820312500000000, 0.3095703125000000000, 0.3100585937500000000, 0.3105468750000000000, 0.3110351562500000000, 0.3115234375000000000, 0.3120117187500000000, 0.3125000000000000000, 0.3129882812500000000, 0.3134765625000000000, 0.3139648437500000000, 0.3144531250000000000, 0.3149414062500000000, 0.3154296875000000000, 0.3159179687500000000, 0.3164062500000000000, 0.3168945312500000000, 0.3173828125000000000, 0.3178710937500000000, 0.3183593750000000000, 0.3188476562500000000, 0.3193359375000000000, 0.3198242187500000000, 0.3203125000000000000, 0.3208007812500000000, 0.3212890625000000000, 0.3217773437500000000, 0.3222656250000000000, 0.3227539062500000000, 0.3232421875000000000, 0.3237304687500000000, 0.3242187500000000000, 0.3247070312500000000, 0.3251953125000000000, 0.3256835937500000000, 0.3261718750000000000, 0.3266601562500000000, 0.3271484375000000000, 0.3276367187500000000, 0.3281250000000000000, 0.3286132812500000000, 0.3291015625000000000, 0.3295898437500000000, 0.3300781250000000000, 0.3305664062500000000, 0.3310546875000000000, 0.3315429687500000000, 0.3320312500000000000, 0.3325195312500000000, 0.3330078125000000000, 0.3334960937500000000, 0.3339843750000000000, 0.3344726562500000000, 0.3349609375000000000, 0.3354492187500000000, 0.3359375000000000000, 0.3364257812500000000, 0.3369140625000000000, 0.3374023437500000000, 0.3378906250000000000, 0.3383789062500000000, 0.3388671875000000000, 0.3393554687500000000, 0.3398437500000000000, 0.3403320312500000000, 0.3408203125000000000, 0.3413085937500000000, 0.3417968750000000000, 0.3422851562500000000, 0.3427734375000000000, 0.3432617187500000000, 0.3437500000000000000, 0.3442382812500000000, 0.3447265625000000000, 0.3452148437500000000, 0.3457031250000000000, 0.3461914062500000000, 0.3466796875000000000, 0.3471679687500000000, 0.3476562500000000000, 0.3481445312500000000, 0.3486328125000000000, 0.3491210937500000000, 0.3496093750000000000, 0.3500976562500000000, 0.3505859375000000000, 0.3510742187500000000, 0.3515625000000000000, 0.3520507812500000000, 0.3525390625000000000, 0.3530273437500000000, 0.3535156250000000000, 0.3540039062500000000, 0.3544921875000000000, 0.3549804687500000000, 0.3554687500000000000, 0.3559570312500000000, 0.3564453125000000000, 0.3569335937500000000, 0.3574218750000000000, 0.3579101562500000000, 0.3583984375000000000, 0.3588867187500000000, 0.3593750000000000000, 0.3598632812500000000, 0.3603515625000000000, 0.3608398437500000000, 0.3613281250000000000, 0.3618164062500000000, 0.3623046875000000000, 0.3627929687500000000, 0.3632812500000000000, 0.3637695312500000000, 0.3642578125000000000, 0.3647460937500000000, 0.3652343750000000000, 0.3657226562500000000, 0.3662109375000000000, 0.3666992187500000000, 0.3671875000000000000, 0.3676757812500000000, 0.3681640625000000000, 0.3686523437500000000, 0.3691406250000000000, 0.3696289062500000000, 0.3701171875000000000, 0.3706054687500000000, 0.3710937500000000000, 0.3715820312500000000, 0.3720703125000000000, 0.3725585937500000000, 0.3730468750000000000, 0.3735351562500000000, 0.3740234375000000000, 0.3745117187500000000, 0.3750000000000000000, 0.3754882812500000555, 0.3759765625000000555, 0.3764648437500000555, 0.3769531250000000555, 0.3774414062500000555, 0.3779296875000000555, 0.3784179687500000555, 0.3789062500000000555, 0.3793945312500000555, 0.3798828125000000555, 0.3803710937500000555, 0.3808593750000000555, 0.3813476562500000555, 0.3818359375000000555, 0.3823242187500000555, 0.3828125000000000555, 0.3833007812500000555, 0.3837890625000000555, 0.3842773437500000555, 0.3847656250000000555, 0.3852539062500000555, 0.3857421875000000555, 0.3862304687500000555, 0.3867187500000000555, 0.3872070312500000555, 0.3876953125000000555, 0.3881835937500000555, 0.3886718750000000555, 0.3891601562500000555, 0.3896484375000000555, 0.3901367187500000555, 0.3906250000000000555, 0.3911132812500000555, 0.3916015625000000555, 0.3920898437500000555, 0.3925781250000000555, 0.3930664062500000555, 0.3935546875000000555, 0.3940429687500000555, 0.3945312500000000555, 0.3950195312500000555, 0.3955078125000000555, 0.3959960937500000555, 0.3964843750000000555, 0.3969726562500000555, 0.3974609375000000555, 0.3979492187500000555, 0.3984375000000000555, 0.3989257812500000555, 0.3994140625000000555, 0.3999023437500000555, 0.4003906250000000555, 0.4008789062500000555, 0.4013671875000000555, 0.4018554687500000555, 0.4023437500000000555, 0.4028320312500000555, 0.4033203125000000555, 0.4038085937500000555, 0.4042968750000000555, 0.4047851562500000555, 0.4052734375000000555, 0.4057617187500000555, 0.4062500000000000555, 0.4067382812500000555, 0.4072265625000000555, 0.4077148437500000555, 0.4082031250000000555, 0.4086914062500000555, 0.4091796875000000555, 0.4096679687500000555, 0.4101562500000000555, 0.4106445312500000555, 0.4111328125000000555, 0.4116210937500000555, 0.4121093750000000555, 0.4125976562500000555, 0.4130859375000000555, 0.4135742187500000555, 0.4140625000000000555, 0.4145507812500000555, 0.4150390625000000555, 0.4155273437500000555, 0.4160156250000000555, 0.4165039062500000555, 0.4169921875000000555, 0.4174804687500000555, 0.4179687500000000555, 0.4184570312500000555, 0.4189453125000000555, 0.4194335937500000555, 0.4199218750000000555, 0.4204101562500000555, 0.4208984375000000555, 0.4213867187500000555, 0.4218750000000000555, 0.4223632812500000555, 0.4228515625000000555, 0.4233398437500000555, 0.4238281250000000555, 0.4243164062500000555, 0.4248046875000000555, 0.4252929687500000555, 0.4257812500000000555, 0.4262695312500000555, 0.4267578125000000555, 0.4272460937500000555, 0.4277343750000000555, 0.4282226562500000555, 0.4287109375000000555, 0.4291992187500000555, 0.4296875000000000555, 0.4301757812500000555, 0.4306640625000000555, 0.4311523437500000555, 0.4316406250000000555, 0.4321289062500000555, 0.4326171875000000555, 0.4331054687500000555, 0.4335937500000000555, 0.4340820312500000555, 0.4345703125000000555, 0.4350585937500000555, 0.4355468750000000555, 0.4360351562500000555, 0.4365234375000000555, 0.4370117187500000555, 0.4375000000000000555, 0.4379882812500000555, 0.4384765625000000555, 0.4389648437500000555, 0.4394531250000000555, 0.4399414062500000555, 0.4404296875000000555, 0.4409179687500000555, 0.4414062500000000555, 0.4418945312500000555, 0.4423828125000000555, 0.4428710937500000555, 0.4433593750000000555, 0.4438476562500000555, 0.4443359375000000555, 0.4448242187500000555, 0.4453125000000000555, 0.4458007812500000555, 0.4462890625000000555, 0.4467773437500000555, 0.4472656250000000555, 0.4477539062500000555, 0.4482421875000000555, 0.4487304687500000555, 0.4492187500000000555, 0.4497070312500000555, 0.4501953125000000555, 0.4506835937500000555, 0.4511718750000000555, 0.4516601562500000555, 0.4521484375000000555, 0.4526367187500000555, 0.4531250000000000555, 0.4536132812500000555, 0.4541015625000000555, 0.4545898437500000555, 0.4550781250000000555, 0.4555664062500000555, 0.4560546875000000555, 0.4565429687500000555, 0.4570312500000000555, 0.4575195312500000555, 0.4580078125000000555, 0.4584960937500000555, 0.4589843750000000555, 0.4594726562500000555, 0.4599609375000000555, 0.4604492187500000555, 0.4609375000000000555, 0.4614257812500000555, 0.4619140625000000555, 0.4624023437500000555, 0.4628906250000000555, 0.4633789062500000555, 0.4638671875000000555, 0.4643554687500000555, 0.4648437500000000555, 0.4653320312500000555, 0.4658203125000000555, 0.4663085937500000555, 0.4667968750000000555, 0.4672851562500000555, 0.4677734375000000555, 0.4682617187500000555, 0.4687500000000000555, 0.4692382812500000555, 0.4697265625000000555, 0.4702148437500000555, 0.4707031250000000555, 0.4711914062500000555, 0.4716796875000000555, 0.4721679687500000555, 0.4726562500000000555, 0.4731445312500000555, 0.4736328125000000555, 0.4741210937500000555, 0.4746093750000000555, 0.4750976562500000555, 0.4755859375000000555, 0.4760742187500000555, 0.4765625000000000555, 0.4770507812500000555, 0.4775390625000000555, 0.4780273437500000555, 0.4785156250000000555, 0.4790039062500000555, 0.4794921875000000555, 0.4799804687500000555, 0.4804687500000000555, 0.4809570312500000555, 0.4814453125000000555, 0.4819335937500000555, 0.4824218750000000555, 0.4829101562500000555, 0.4833984375000000555, 0.4838867187500000555, 0.4843750000000000555, 0.4848632812500000555, 0.4853515625000000555, 0.4858398437500000555, 0.4863281250000000555, 0.4868164062500000555, 0.4873046875000000555, 0.4877929687500000555, 0.4882812500000000555, 0.4887695312500000555, 0.4892578125000000555, 0.4897460937500000555, 0.4902343750000000555, 0.4907226562500000555, 0.4912109375000000555, 0.4916992187500000555, 0.4921875000000000555, 0.4926757812500000555, 0.4931640625000000555, 0.4936523437500000555, 0.4941406250000000555, 0.4946289062500000555, 0.4951171875000000555, 0.4956054687500000555, 0.4960937500000000555, 0.4965820312500000555, 0.4970703125000000555, 0.4975585937500000555, 0.4980468750000000555, 0.4985351562500000555, 0.4990234375000000555, 0.4995117187500000555, 0.5000000000000000000, 0.5004882812500000000, 0.5009765625000000000, 0.5014648437500000000, 0.5019531250000000000, 0.5024414062500000000, 0.5029296875000000000, 0.5034179687500000000, 0.5039062500000000000, 0.5043945312500000000, 0.5048828125000000000, 0.5053710937500000000, 0.5058593750000000000, 0.5063476562500000000, 0.5068359375000000000, 0.5073242187500000000, 0.5078125000000000000, 0.5083007812500000000, 0.5087890625000000000, 0.5092773437500000000, 0.5097656250000000000, 0.5102539062500000000, 0.5107421875000000000, 0.5112304687500000000, 0.5117187500000000000, 0.5122070312500000000, 0.5126953125000000000, 0.5131835937500000000, 0.5136718750000000000, 0.5141601562500000000, 0.5146484375000000000, 0.5151367187500000000, 0.5156250000000000000, 0.5161132812500000000, 0.5166015625000000000, 0.5170898437500000000, 0.5175781250000000000, 0.5180664062500000000, 0.5185546875000000000, 0.5190429687500000000, 0.5195312500000000000, 0.5200195312500000000, 0.5205078125000000000, 0.5209960937500000000, 0.5214843750000000000, 0.5219726562500000000, 0.5224609375000000000, 0.5229492187500000000, 0.5234375000000000000, 0.5239257812500000000, 0.5244140625000000000, 0.5249023437500000000, 0.5253906250000000000, 0.5258789062500000000, 0.5263671875000000000, 0.5268554687500000000, 0.5273437500000000000, 0.5278320312500000000, 0.5283203125000000000, 0.5288085937500000000, 0.5292968750000000000, 0.5297851562500000000, 0.5302734375000000000, 0.5307617187500000000, 0.5312500000000000000, 0.5317382812500000000, 0.5322265625000000000, 0.5327148437500000000, 0.5332031250000000000, 0.5336914062500000000, 0.5341796875000000000, 0.5346679687500000000, 0.5351562500000000000, 0.5356445312500000000, 0.5361328125000000000, 0.5366210937500000000, 0.5371093750000000000, 0.5375976562500000000, 0.5380859375000000000, 0.5385742187500000000, 0.5390625000000000000, 0.5395507812500000000, 0.5400390625000000000, 0.5405273437500000000, 0.5410156250000000000, 0.5415039062500000000, 0.5419921875000000000, 0.5424804687500000000, 0.5429687500000000000, 0.5434570312500000000, 0.5439453125000000000, 0.5444335937500000000, 0.5449218750000000000, 0.5454101562500000000, 0.5458984375000000000, 0.5463867187500000000, 0.5468750000000000000, 0.5473632812500000000, 0.5478515625000000000, 0.5483398437500000000, 0.5488281250000000000, 0.5493164062500000000, 0.5498046875000000000, 0.5502929687500000000, 0.5507812500000000000, 0.5512695312500000000, 0.5517578125000000000, 0.5522460937500000000, 0.5527343750000000000, 0.5532226562500000000, 0.5537109375000000000, 0.5541992187500000000, 0.5546875000000000000, 0.5551757812500000000, 0.5556640625000000000, 0.5561523437500000000, 0.5566406250000000000, 0.5571289062500000000, 0.5576171875000000000, 0.5581054687500000000, 0.5585937500000000000, 0.5590820312500000000, 0.5595703125000000000, 0.5600585937500000000, 0.5605468750000000000, 0.5610351562500000000, 0.5615234375000000000, 0.5620117187500000000, 0.5625000000000000000, 0.5629882812500000000, 0.5634765625000000000, 0.5639648437500000000, 0.5644531250000000000, 0.5649414062500000000, 0.5654296875000000000, 0.5659179687500000000, 0.5664062500000000000, 0.5668945312500000000, 0.5673828125000000000, 0.5678710937500000000, 0.5683593750000000000, 0.5688476562500000000, 0.5693359375000000000, 0.5698242187500000000, 0.5703125000000000000, 0.5708007812500000000, 0.5712890625000000000, 0.5717773437500000000, 0.5722656250000000000, 0.5727539062500000000, 0.5732421875000000000, 0.5737304687500000000, 0.5742187500000000000, 0.5747070312500000000, 0.5751953125000000000, 0.5756835937500000000, 0.5761718750000000000, 0.5766601562500000000, 0.5771484375000000000, 0.5776367187500000000, 0.5781250000000000000, 0.5786132812500000000, 0.5791015625000000000, 0.5795898437500000000, 0.5800781250000000000, 0.5805664062500000000, 0.5810546875000000000, 0.5815429687500000000, 0.5820312500000000000, 0.5825195312500000000, 0.5830078125000000000, 0.5834960937500000000, 0.5839843750000000000, 0.5844726562500000000, 0.5849609375000000000, 0.5854492187500000000, 0.5859375000000000000, 0.5864257812500000000, 0.5869140625000000000, 0.5874023437500000000, 0.5878906250000000000, 0.5883789062500000000, 0.5888671875000000000, 0.5893554687500000000, 0.5898437500000000000, 0.5903320312500000000, 0.5908203125000000000, 0.5913085937500000000, 0.5917968750000000000, 0.5922851562500000000, 0.5927734375000000000, 0.5932617187500000000, 0.5937500000000000000, 0.5942382812500000000, 0.5947265625000000000, 0.5952148437500000000, 0.5957031250000000000, 0.5961914062500000000, 0.5966796875000000000, 0.5971679687500000000, 0.5976562500000000000, 0.5981445312500000000, 0.5986328125000000000, 0.5991210937500000000, 0.5996093750000000000, 0.6000976562500000000, 0.6005859375000000000, 0.6010742187500000000, 0.6015625000000000000, 0.6020507812500000000, 0.6025390625000000000, 0.6030273437500000000, 0.6035156250000000000, 0.6040039062500000000, 0.6044921875000000000, 0.6049804687500000000, 0.6054687500000000000, 0.6059570312500000000, 0.6064453125000000000, 0.6069335937500000000, 0.6074218750000000000, 0.6079101562500000000, 0.6083984375000000000, 0.6088867187500000000, 0.6093750000000000000, 0.6098632812500000000, 0.6103515625000000000, 0.6108398437500000000, 0.6113281250000000000, 0.6118164062500000000, 0.6123046875000000000, 0.6127929687500000000, 0.6132812500000000000, 0.6137695312500000000, 0.6142578125000000000, 0.6147460937500000000, 0.6152343750000000000, 0.6157226562500000000, 0.6162109375000000000, 0.6166992187500000000, 0.6171875000000000000, 0.6176757812500000000, 0.6181640625000000000, 0.6186523437500000000, 0.6191406250000000000, 0.6196289062500000000, 0.6201171875000000000, 0.6206054687500000000, 0.6210937500000000000, 0.6215820312500000000, 0.6220703125000000000, 0.6225585937500000000, 0.6230468750000000000, 0.6235351562500000000, 0.6240234375000000000, 0.6245117187500000000, 0.6250000000000000000, 0.6254882812500000000, 0.6259765625000000000, 0.6264648437500000000, 0.6269531250000000000, 0.6274414062500000000, 0.6279296875000000000, 0.6284179687500000000, 0.6289062500000000000, 0.6293945312500000000, 0.6298828125000000000, 0.6303710937500000000, 0.6308593750000000000, 0.6313476562500000000, 0.6318359375000000000, 0.6323242187500000000, 0.6328125000000000000, 0.6333007812500000000, 0.6337890625000000000, 0.6342773437500000000, 0.6347656250000000000, 0.6352539062500000000, 0.6357421875000000000, 0.6362304687500000000, 0.6367187500000000000, 0.6372070312500000000, 0.6376953125000000000, 0.6381835937500000000, 0.6386718750000000000, 0.6391601562500000000, 0.6396484375000000000, 0.6401367187500000000, 0.6406250000000000000, 0.6411132812500000000, 0.6416015625000000000, 0.6420898437500000000, 0.6425781250000000000, 0.6430664062500000000, 0.6435546875000000000, 0.6440429687500000000, 0.6445312500000000000, 0.6450195312500000000, 0.6455078125000000000, 0.6459960937500000000, 0.6464843750000000000, 0.6469726562500000000, 0.6474609375000000000, 0.6479492187500000000, 0.6484375000000000000, 0.6489257812500000000, 0.6494140625000000000, 0.6499023437500000000, 0.6503906250000000000, 0.6508789062500000000, 0.6513671875000000000, 0.6518554687500000000, 0.6523437500000000000, 0.6528320312500000000, 0.6533203125000000000, 0.6538085937500000000, 0.6542968750000000000, 0.6547851562500000000, 0.6552734375000000000, 0.6557617187500000000, 0.6562500000000000000, 0.6567382812500000000, 0.6572265625000000000, 0.6577148437500000000, 0.6582031250000000000, 0.6586914062500000000, 0.6591796875000000000, 0.6596679687500000000, 0.6601562500000000000, 0.6606445312500000000, 0.6611328125000000000, 0.6616210937500000000, 0.6621093750000000000, 0.6625976562500000000, 0.6630859375000000000, 0.6635742187500000000, 0.6640625000000000000, 0.6645507812500000000, 0.6650390625000000000, 0.6655273437500000000, 0.6660156250000000000, 0.6665039062500000000, 0.6669921875000000000, 0.6674804687500000000, 0.6679687500000000000, 0.6684570312500000000, 0.6689453125000000000, 0.6694335937500000000, 0.6699218750000000000, 0.6704101562500000000, 0.6708984375000000000, 0.6713867187500000000, 0.6718750000000000000, 0.6723632812500000000, 0.6728515625000000000, 0.6733398437500000000, 0.6738281250000000000, 0.6743164062500000000, 0.6748046875000000000, 0.6752929687500000000, 0.6757812500000000000, 0.6762695312500000000, 0.6767578125000000000, 0.6772460937500000000, 0.6777343750000000000, 0.6782226562500000000, 0.6787109375000000000, 0.6791992187500000000, 0.6796875000000000000, 0.6801757812500000000, 0.6806640625000000000, 0.6811523437500000000, 0.6816406250000000000, 0.6821289062500000000, 0.6826171875000000000, 0.6831054687500000000, 0.6835937500000000000, 0.6840820312500000000, 0.6845703125000000000, 0.6850585937500000000, 0.6855468750000000000, 0.6860351562500000000, 0.6865234375000000000, 0.6870117187500000000, 0.6875000000000000000, 0.6879882812500000000, 0.6884765625000000000, 0.6889648437500000000, 0.6894531250000000000, 0.6899414062500000000, 0.6904296875000000000, 0.6909179687500000000, 0.6914062500000000000, 0.6918945312500000000, 0.6923828125000000000, 0.6928710937500000000, 0.6933593750000000000, 0.6938476562500000000, 0.6943359375000000000, 0.6948242187500000000, 0.6953125000000000000, 0.6958007812500000000, 0.6962890625000000000, 0.6967773437500000000, 0.6972656250000000000, 0.6977539062500000000, 0.6982421875000000000, 0.6987304687500000000, 0.6992187500000000000, 0.6997070312500000000, 0.7001953125000000000, 0.7006835937500000000, 0.7011718750000000000, 0.7016601562500000000, 0.7021484375000000000, 0.7026367187500000000, 0.7031250000000000000, 0.7036132812500000000, 0.7041015625000000000, 0.7045898437500000000, 0.7050781250000000000, 0.7055664062500000000, 0.7060546875000000000, 0.7065429687500000000, 0.7070312500000000000, 0.7075195312500000000, 0.7080078125000000000, 0.7084960937500000000, 0.7089843750000000000, 0.7094726562500000000, 0.7099609375000000000, 0.7104492187500000000, 0.7109375000000000000, 0.7114257812500000000, 0.7119140625000000000, 0.7124023437500000000, 0.7128906250000000000, 0.7133789062500000000, 0.7138671875000000000, 0.7143554687500000000, 0.7148437500000000000, 0.7153320312500000000, 0.7158203125000000000, 0.7163085937500000000, 0.7167968750000000000, 0.7172851562500000000, 0.7177734375000000000, 0.7182617187500000000, 0.7187500000000000000, 0.7192382812500000000, 0.7197265625000000000, 0.7202148437500000000, 0.7207031250000000000, 0.7211914062500000000, 0.7216796875000000000, 0.7221679687500000000, 0.7226562500000000000, 0.7231445312500000000, 0.7236328125000000000, 0.7241210937500000000, 0.7246093750000000000, 0.7250976562500000000, 0.7255859375000000000, 0.7260742187500000000, 0.7265625000000000000, 0.7270507812500000000, 0.7275390625000000000, 0.7280273437500000000, 0.7285156250000000000, 0.7290039062500000000, 0.7294921875000000000, 0.7299804687500000000, 0.7304687500000000000, 0.7309570312500000000, 0.7314453125000000000, 0.7319335937500000000, 0.7324218750000000000, 0.7329101562500000000, 0.7333984375000000000, 0.7338867187500000000, 0.7343750000000000000, 0.7348632812500000000, 0.7353515625000000000, 0.7358398437500000000, 0.7363281250000000000, 0.7368164062500000000, 0.7373046875000000000, 0.7377929687500000000, 0.7382812500000000000, 0.7387695312500000000, 0.7392578125000000000, 0.7397460937500000000, 0.7402343750000000000, 0.7407226562500000000, 0.7412109375000000000, 0.7416992187500000000, 0.7421875000000000000, 0.7426757812500000000, 0.7431640625000000000, 0.7436523437500000000, 0.7441406250000000000, 0.7446289062500000000, 0.7451171875000000000, 0.7456054687500000000, 0.7460937500000000000, 0.7465820312500000000, 0.7470703125000000000, 0.7475585937500000000, 0.7480468750000000000, 0.7485351562500000000, 0.7490234375000000000, 0.7495117187500000000, 0.7500000000000000000, 0.7504882812500001110, 0.7509765625000001110, 0.7514648437500001110, 0.7519531250000001110, 0.7524414062500001110, 0.7529296875000001110, 0.7534179687500001110, 0.7539062500000001110, 0.7543945312500001110, 0.7548828125000001110, 0.7553710937500001110, 0.7558593750000001110, 0.7563476562500001110, 0.7568359375000001110, 0.7573242187500001110, 0.7578125000000001110, 0.7583007812500001110, 0.7587890625000001110, 0.7592773437500001110, 0.7597656250000001110, 0.7602539062500001110, 0.7607421875000001110, 0.7612304687500001110, 0.7617187500000001110, 0.7622070312500001110, 0.7626953125000001110, 0.7631835937500001110, 0.7636718750000001110, 0.7641601562500001110, 0.7646484375000001110, 0.7651367187500001110, 0.7656250000000001110, 0.7661132812500001110, 0.7666015625000001110, 0.7670898437500001110, 0.7675781250000001110, 0.7680664062500001110, 0.7685546875000001110, 0.7690429687500001110, 0.7695312500000001110, 0.7700195312500001110, 0.7705078125000001110, 0.7709960937500001110, 0.7714843750000001110, 0.7719726562500001110, 0.7724609375000001110, 0.7729492187500001110, 0.7734375000000001110, 0.7739257812500001110, 0.7744140625000001110, 0.7749023437500001110, 0.7753906250000001110, 0.7758789062500001110, 0.7763671875000001110, 0.7768554687500001110, 0.7773437500000001110, 0.7778320312500001110, 0.7783203125000001110, 0.7788085937500001110, 0.7792968750000001110, 0.7797851562500001110, 0.7802734375000001110, 0.7807617187500001110, 0.7812500000000001110, 0.7817382812500001110, 0.7822265625000001110, 0.7827148437500001110, 0.7832031250000001110, 0.7836914062500001110, 0.7841796875000001110, 0.7846679687500001110, 0.7851562500000001110, 0.7856445312500001110, 0.7861328125000001110, 0.7866210937500001110, 0.7871093750000001110, 0.7875976562500001110, 0.7880859375000001110, 0.7885742187500001110, 0.7890625000000001110, 0.7895507812500001110, 0.7900390625000001110, 0.7905273437500001110, 0.7910156250000001110, 0.7915039062500001110, 0.7919921875000001110, 0.7924804687500001110, 0.7929687500000001110, 0.7934570312500001110, 0.7939453125000001110, 0.7944335937500001110, 0.7949218750000001110, 0.7954101562500001110, 0.7958984375000001110, 0.7963867187500001110, 0.7968750000000001110, 0.7973632812500001110, 0.7978515625000001110, 0.7983398437500001110, 0.7988281250000001110, 0.7993164062500001110, 0.7998046875000001110, 0.8002929687500001110, 0.8007812500000001110, 0.8012695312500001110, 0.8017578125000001110, 0.8022460937500001110, 0.8027343750000001110, 0.8032226562500001110, 0.8037109375000001110, 0.8041992187500001110, 0.8046875000000001110, 0.8051757812500001110, 0.8056640625000001110, 0.8061523437500001110, 0.8066406250000001110, 0.8071289062500001110, 0.8076171875000001110, 0.8081054687500001110, 0.8085937500000001110, 0.8090820312500001110, 0.8095703125000001110, 0.8100585937500001110, 0.8105468750000001110, 0.8110351562500001110, 0.8115234375000001110, 0.8120117187500001110, 0.8125000000000001110, 0.8129882812500001110, 0.8134765625000001110, 0.8139648437500001110, 0.8144531250000001110, 0.8149414062500001110, 0.8154296875000001110, 0.8159179687500001110, 0.8164062500000001110, 0.8168945312500001110, 0.8173828125000001110, 0.8178710937500001110, 0.8183593750000001110, 0.8188476562500001110, 0.8193359375000001110, 0.8198242187500001110, 0.8203125000000001110, 0.8208007812500001110, 0.8212890625000001110, 0.8217773437500001110, 0.8222656250000001110, 0.8227539062500001110, 0.8232421875000001110, 0.8237304687500001110, 0.8242187500000001110, 0.8247070312500001110, 0.8251953125000001110, 0.8256835937500001110, 0.8261718750000001110, 0.8266601562500001110, 0.8271484375000001110, 0.8276367187500001110, 0.8281250000000001110, 0.8286132812500001110, 0.8291015625000001110, 0.8295898437500001110, 0.8300781250000001110, 0.8305664062500001110, 0.8310546875000001110, 0.8315429687500001110, 0.8320312500000001110, 0.8325195312500001110, 0.8330078125000001110, 0.8334960937500001110, 0.8339843750000001110, 0.8344726562500001110, 0.8349609375000001110, 0.8354492187500001110, 0.8359375000000001110, 0.8364257812500001110, 0.8369140625000001110, 0.8374023437500001110, 0.8378906250000001110, 0.8383789062500001110, 0.8388671875000001110, 0.8393554687500001110, 0.8398437500000001110, 0.8403320312500001110, 0.8408203125000001110, 0.8413085937500001110, 0.8417968750000001110, 0.8422851562500001110, 0.8427734375000001110, 0.8432617187500001110, 0.8437500000000001110, 0.8442382812500001110, 0.8447265625000001110, 0.8452148437500001110, 0.8457031250000001110, 0.8461914062500001110, 0.8466796875000001110, 0.8471679687500001110, 0.8476562500000001110, 0.8481445312500001110, 0.8486328125000001110, 0.8491210937500001110, 0.8496093750000001110, 0.8500976562500001110, 0.8505859375000001110, 0.8510742187500001110, 0.8515625000000001110, 0.8520507812500001110, 0.8525390625000001110, 0.8530273437500001110, 0.8535156250000001110, 0.8540039062500001110, 0.8544921875000001110, 0.8549804687500001110, 0.8554687500000001110, 0.8559570312500001110, 0.8564453125000001110, 0.8569335937500001110, 0.8574218750000001110, 0.8579101562500001110, 0.8583984375000001110, 0.8588867187500001110, 0.8593750000000001110, 0.8598632812500001110, 0.8603515625000001110, 0.8608398437500001110, 0.8613281250000001110, 0.8618164062500001110, 0.8623046875000001110, 0.8627929687500001110, 0.8632812500000001110, 0.8637695312500001110, 0.8642578125000001110, 0.8647460937500001110, 0.8652343750000001110, 0.8657226562500001110, 0.8662109375000001110, 0.8666992187500001110, 0.8671875000000001110, 0.8676757812500001110, 0.8681640625000001110, 0.8686523437500001110, 0.8691406250000001110, 0.8696289062500001110, 0.8701171875000001110, 0.8706054687500001110, 0.8710937500000001110, 0.8715820312500001110, 0.8720703125000001110, 0.8725585937500001110, 0.8730468750000001110, 0.8735351562500001110, 0.8740234375000001110, 0.8745117187500001110, 0.8750000000000001110, 0.8754882812500001110, 0.8759765625000001110, 0.8764648437500001110, 0.8769531250000001110, 0.8774414062500001110, 0.8779296875000001110, 0.8784179687500001110, 0.8789062500000001110, 0.8793945312500001110, 0.8798828125000001110, 0.8803710937500001110, 0.8808593750000001110, 0.8813476562500001110, 0.8818359375000001110, 0.8823242187500001110, 0.8828125000000001110, 0.8833007812500001110, 0.8837890625000001110, 0.8842773437500001110, 0.8847656250000001110, 0.8852539062500001110, 0.8857421875000001110, 0.8862304687500001110, 0.8867187500000001110, 0.8872070312500001110, 0.8876953125000001110, 0.8881835937500001110, 0.8886718750000001110, 0.8891601562500001110, 0.8896484375000001110, 0.8901367187500001110, 0.8906250000000001110, 0.8911132812500001110, 0.8916015625000001110, 0.8920898437500001110, 0.8925781250000001110, 0.8930664062500001110, 0.8935546875000001110, 0.8940429687500001110, 0.8945312500000001110, 0.8950195312500001110, 0.8955078125000001110, 0.8959960937500001110, 0.8964843750000001110, 0.8969726562500001110, 0.8974609375000001110, 0.8979492187500001110, 0.8984375000000001110, 0.8989257812500001110, 0.8994140625000001110, 0.8999023437500001110, 0.9003906250000001110, 0.9008789062500001110, 0.9013671875000001110, 0.9018554687500001110, 0.9023437500000001110, 0.9028320312500001110, 0.9033203125000001110, 0.9038085937500001110, 0.9042968750000001110, 0.9047851562500001110, 0.9052734375000001110, 0.9057617187500001110, 0.9062500000000001110, 0.9067382812500001110, 0.9072265625000001110, 0.9077148437500001110, 0.9082031250000001110, 0.9086914062500001110, 0.9091796875000001110, 0.9096679687500001110, 0.9101562500000001110, 0.9106445312500001110, 0.9111328125000001110, 0.9116210937500001110, 0.9121093750000001110, 0.9125976562500001110, 0.9130859375000001110, 0.9135742187500001110, 0.9140625000000001110, 0.9145507812500001110, 0.9150390625000001110, 0.9155273437500001110, 0.9160156250000001110, 0.9165039062500001110, 0.9169921875000001110, 0.9174804687500001110, 0.9179687500000001110, 0.9184570312500001110, 0.9189453125000001110, 0.9194335937500001110, 0.9199218750000001110, 0.9204101562500001110, 0.9208984375000001110, 0.9213867187500001110, 0.9218750000000001110, 0.9223632812500001110, 0.9228515625000001110, 0.9233398437500001110, 0.9238281250000001110, 0.9243164062500001110, 0.9248046875000001110, 0.9252929687500001110, 0.9257812500000001110, 0.9262695312500001110, 0.9267578125000001110, 0.9272460937500001110, 0.9277343750000001110, 0.9282226562500001110, 0.9287109375000001110, 0.9291992187500001110, 0.9296875000000001110, 0.9301757812500001110, 0.9306640625000001110, 0.9311523437500001110, 0.9316406250000001110, 0.9321289062500001110, 0.9326171875000001110, 0.9331054687500001110, 0.9335937500000001110, 0.9340820312500001110, 0.9345703125000001110, 0.9350585937500001110, 0.9355468750000001110, 0.9360351562500001110, 0.9365234375000001110, 0.9370117187500001110, 0.9375000000000001110, 0.9379882812500001110, 0.9384765625000001110, 0.9389648437500001110, 0.9394531250000001110, 0.9399414062500001110, 0.9404296875000001110, 0.9409179687500001110, 0.9414062500000001110, 0.9418945312500001110, 0.9423828125000001110, 0.9428710937500001110, 0.9433593750000001110, 0.9438476562500001110, 0.9443359375000001110, 0.9448242187500001110, 0.9453125000000001110, 0.9458007812500001110, 0.9462890625000001110, 0.9467773437500001110, 0.9472656250000001110, 0.9477539062500001110, 0.9482421875000001110, 0.9487304687500001110, 0.9492187500000001110, 0.9497070312500001110, 0.9501953125000001110, 0.9506835937500001110, 0.9511718750000001110, 0.9516601562500001110, 0.9521484375000001110, 0.9526367187500001110, 0.9531250000000001110, 0.9536132812500001110, 0.9541015625000001110, 0.9545898437500001110, 0.9550781250000001110, 0.9555664062500001110, 0.9560546875000001110, 0.9565429687500001110, 0.9570312500000001110, 0.9575195312500001110, 0.9580078125000001110, 0.9584960937500001110, 0.9589843750000001110, 0.9594726562500001110, 0.9599609375000001110, 0.9604492187500001110, 0.9609375000000001110, 0.9614257812500001110, 0.9619140625000001110, 0.9624023437500001110, 0.9628906250000001110, 0.9633789062500001110, 0.9638671875000001110, 0.9643554687500001110, 0.9648437500000001110, 0.9653320312500001110, 0.9658203125000001110, 0.9663085937500001110, 0.9667968750000001110, 0.9672851562500001110, 0.9677734375000001110, 0.9682617187500001110, 0.9687500000000001110, 0.9692382812500001110, 0.9697265625000001110, 0.9702148437500001110, 0.9707031250000001110, 0.9711914062500001110, 0.9716796875000001110, 0.9721679687500001110, 0.9726562500000001110, 0.9731445312500001110, 0.9736328125000001110, 0.9741210937500001110, 0.9746093750000001110, 0.9750976562500001110, 0.9755859375000001110, 0.9760742187500001110, 0.9765625000000001110, 0.9770507812500001110, 0.9775390625000001110, 0.9780273437500001110, 0.9785156250000001110, 0.9790039062500001110, 0.9794921875000001110, 0.9799804687500001110, 0.9804687500000001110, 0.9809570312500001110, 0.9814453125000001110, 0.9819335937500001110, 0.9824218750000001110, 0.9829101562500001110, 0.9833984375000001110, 0.9838867187500001110, 0.9843750000000001110, 0.9848632812500001110, 0.9853515625000001110, 0.9858398437500001110, 0.9863281250000001110, 0.9868164062500001110, 0.9873046875000001110, 0.9877929687500001110, 0.9882812500000001110, 0.9887695312500001110, 0.9892578125000001110, 0.9897460937500001110, 0.9902343750000001110, 0.9907226562500001110, 0.9912109375000001110, 0.9916992187500001110, 0.9921875000000001110, 0.9926757812500001110, 0.9931640625000001110, 0.9936523437500001110, 0.9941406250000001110, 0.9946289062500001110, 0.9951171875000001110, 0.9956054687500001110, 0.9960937500000001110, 0.9965820312500001110, 0.9970703125000001110, 0.9975585937500001110, 0.9980468750000001110, 0.9985351562500001110, 0.9990234375000001110, 0.9995117187500001110, 1.000000000000000000 ),
 .UNSPECIFIED. ) ;
#18992 = CARTESIAN_POINT ( 'NONE',  ( 12.78316523911058944, -16.47895720935621711, 11.49999999999998934 ) ) ;
#18993 = VERTEX_POINT ( 'NONE', #15315 ) ;
#18995 = VERTEX_POINT ( 'NONE', #30547 ) ;
#18994 = CARTESIAN_POINT ( 'NONE',  ( -40.34598903906039169, -25.11096149773888797, 2.835861264366675183 ) ) ;
#18996 = ORIENTED_EDGE ( 'NONE', *, *, #64377, .F. ) ;
#18997 = CARTESIAN_POINT ( 'NONE',  ( -42.62287095715006302, -23.47596703998600276, 11.44779298504227505 ) ) ;
#18998 = CARTESIAN_POINT ( 'NONE',  ( -11.11193726737652199, 17.91617163517716804, -1.500000000000002220 ) ) ;
#18999 = VERTEX_POINT ( 'NONE', #38153 ) ;
#19000 = LINE ( 'NONE', #3798, #67339 ) ;
#19001 = DIRECTION ( 'NONE',  ( 1.251281512149627050E-16, 0.000000000000000000, -1.000000000000000000 ) ) ;
#19002 = CARTESIAN_POINT ( 'NONE',  ( -120.5523422370003885, -24.92592662359561473, 8.075495903018000021 ) ) ;
#19003 = VECTOR ( 'NONE', #11648, 1000.000000000000000 ) ;
#19004 = CARTESIAN_POINT ( 'NONE',  ( -96.62287095715005592, -23.48783264082478794, -1.443836473390061936 ) ) ;
#19005 = LINE ( 'NONE', #72812, #9246 ) ;
#19006 = CARTESIAN_POINT ( 'NONE',  ( -9.282276271697774916, -19.63344595494797673, -1.500000000000002220 ) ) ;
#19007 = CARTESIAN_POINT ( 'NONE',  ( -79.80079360954597689, -25.07329833162646082, 7.418818858774966607 ) ) ;
#19009 = ORIENTED_EDGE ( 'NONE', *, *, #25512, .T. ) ;
#19008 = CARTESIAN_POINT ( 'NONE',  ( 5.670930919660429836, -21.52877996283707418, 11.49999999999999645 ) ) ;
#19010 = CARTESIAN_POINT ( 'NONE',  ( -50.37830952628071657, -25.24728723542768805, 5.197789135022055085 ) ) ;
#19011 = DIRECTION ( 'NONE',  ( 0.000000000000000000, 0.000000000000000000, 1.000000000000000000 ) ) ;
#19012 = EDGE_CURVE ( 'NONE', #56601, #63059, #92440, .T. ) ;
#19013 = DIRECTION ( 'NONE',  ( -1.000000000000000000, -0.000000000000000000, -0.000000000000000000 ) ) ;
#19014 = EDGE_LOOP ( 'NONE', ( #52625, #94894, #11886, #90636 ) ) ;
#19016 = EDGE_LOOP ( 'NONE', ( #82754, #17350, #47335, #86015 ) ) ;
#19015 = CARTESIAN_POINT ( 'NONE',  ( -40.62287095715004170, -24.15431212366387825, -0.2830839119429072182 ) ) ;
#19017 = EDGE_CURVE ( 'NONE', #34994, #12406, #30130, .T. ) ;
#19018 = EDGE_LOOP ( 'NONE', ( #56713, #90135, #26852, #5761 ) ) ;
#19019 = CARTESIAN_POINT ( 'NONE',  ( -47.55620429048338593, -24.64965694238575011, 8.947790433994200043 ) ) ;
#19020 = ADVANCED_FACE ( 'NONE', ( #53900 ), #46278, .F. ) ;
#19021 = CARTESIAN_POINT ( 'NONE',  ( -121.5543303801803177, -24.34968618360933945, 0.1864209137778886083 ) ) ;
#19022 = DIRECTION ( 'NONE',  ( -1.000000000000000000, -3.773278334444166432E-23, -8.201307841325785021E-29 ) ) ;
#19023 = ADVANCED_FACE ( 'NONE', ( #38659 ), #31044, .T. ) ;
#19024 = CARTESIAN_POINT ( 'NONE',  ( -105.5228709571500758, -24.92579138211019085, 1.929029949965658464 ) ) ;
#19025 = ORIENTED_EDGE ( 'NONE', *, *, #78208, .F. ) ;
#19026 = CARTESIAN_POINT ( 'NONE',  ( -130.5728709571500588, -25.36495145570554399, 3.850034294483935859 ) ) ;
#19027 = CARTESIAN_POINT ( 'NONE',  ( 19.77452139984142221, -10.64395493966388706, -1.500000000000002220 ) ) ;
#19028 = VERTEX_POINT ( 'NONE', #45289 ) ;
#19029 = CARTESIAN_POINT ( 'NONE',  ( -112.5204644665129479, -23.73791477778912551, 11.05961554403169878 ) ) ;
#19030 = CARTESIAN_POINT ( 'NONE',  ( -101.5869878991651234, -24.51419770103158413, 9.386484678747175181 ) ) ;
#19031 = CARTESIAN_POINT ( 'NONE',  ( 1.175186991919848989, -5.965225279485572685, 28.89597625626659649 ) ) ;
#19032 = AXIS2_PLACEMENT_3D ( 'NONE', #97622, #34738, #65710 ) ;
#19033 = LINE ( 'NONE', #64751, #61143 ) ;
#19034 = CARTESIAN_POINT ( 'NONE',  ( -130.5728709571501156, -24.75152770810920444, 1.363349870542269526 ) ) ;
#19035 = CARTESIAN_POINT ( 'NONE',  ( 19.52168601723349894, 1.684101417132040979, 11.49999999999998934 ) ) ;
#19036 = B_SPLINE_SURFACE_WITH_KNOTS ( 'NONE', 3, 3, ( 
 ( #13876, #99106, #60582, #76759 ),
 ( #7259, #99598, #100089, #37228 ),
 ( #30603, #83890, #44847, #98614 ),
 ( #29106, #61575, #22969, #36729 ),
 ( #82397, #60082, #52457, #37719 ),
 ( #68678, #12875, #75771, #68180 ),
 ( #43849, #74778, #9263, #1166 ) ),
 .UNSPECIFIED., .F., .F., .F.,
 ( 4, 3, 4 ),
 ( 4, 4 ),
 ( 0.0004766839783827998963, 0.1029713700210901639, 0.2054660560637975308 ),
 ( 0.1295269466903908040, 0.1305994347416321311 ),
 .UNSPECIFIED. ) ;
#19037 = PLANE ( 'NONE',  #96082 ) ;
#19038 = VERTEX_POINT ( 'NONE', #61015 ) ;
#19039 = CARTESIAN_POINT ( 'NONE',  ( -21.45671390985790694, -1.711987587955616119, -1.500000000000002220 ) ) ;
#19040 = CIRCLE ( 'NONE', #1157, 3.349999999999998757 ) ;
#19041 = FACE_OUTER_BOUND ( 'NONE', #27552, .T. ) ;
#19042 = CARTESIAN_POINT ( 'NONE',  ( -80.76567584835706270, -25.31572652954127278, 4.998963527312024979 ) ) ;
#19043 = CARTESIAN_POINT ( 'NONE',  ( -100.5190840336241820, -25.12077108248912438, 2.833913962057982960 ) ) ;
#19044 = FACE_OUTER_BOUND ( 'NONE', #71948, .T. ) ;
#19045 = CARTESIAN_POINT ( 'NONE',  ( -18.50152239663938403, 13.63810111590111163, -1.500000000000002220 ) ) ;
#19046 = PRODUCT_DEFINITION ( 'UNKNOWN', '', #63621, #19561 ) ;
#19047 = PERSON_AND_ORGANIZATION ( #70597, #27821 ) ;
#19048 = DIRECTION ( 'NONE',  ( -0.5473879298857849962, 5.908253122965993883E-15, -0.8368789961609472972 ) ) ;
#19049 = CARTESIAN_POINT ( 'NONE',  ( -101.5228709571500758, -29.50248528299804818, 1.056150453629042030 ) ) ;
#19050 = CARTESIAN_POINT ( 'NONE',  ( 15.17442925503088169, 13.16703847180013831, 11.49999999999999645 ) ) ;
#19051 = DIRECTION ( 'NONE',  ( -3.773278334453079030E-23, 0.9999999999976377785, 2.173523156925979128E-06 ) ) ;
#19052 = LINE ( 'NONE', #25668, #29009 ) ;
#19053 = CARTESIAN_POINT ( 'NONE',  ( -99.52287095715000476, -23.73907113217737574, -1.053371485780073558 ) ) ;
#19054 = CARTESIAN_POINT ( 'NONE',  ( 12.88745205064171273, 3.316774720517230435, -28.14312002837575477 ) ) ;
#19055 = CARTESIAN_POINT ( 'NONE',  ( 0.5964549592197745387, 8.529703308962702124, 1.700000000000008837 ) ) ;
#19056 = CARTESIAN_POINT ( 'NONE',  ( -15.96263503330635380, 11.84234753045382682, 11.49999999999998934 ) ) ;
#19057 = CARTESIAN_POINT ( 'NONE',  ( -94.52287095715006160, -24.64965694238575011, 8.947790433994196491 ) ) ;
#19058 = CARTESIAN_POINT ( 'NONE',  ( 3.912202881759007767, 19.34271161525698091, -1.500000000000002220 ) ) ;
#19059 = AXIS2_PLACEMENT_3D ( 'NONE', #24635, #55614, #56621 ) ;
#19060 = DIRECTION ( 'NONE',  ( -0.000000000000000000, -1.000000000000000000, -0.000000000000000000 ) ) ;
#19061 = DATE_AND_TIME ( #56148, #53825 ) ;
#19062 = CARTESIAN_POINT ( 'NONE',  ( -98.62287095715005592, -29.50248528299804818, 1.056150453629042030 ) ) ;
#19063 = CARTESIAN_POINT ( 'NONE',  ( 2.949406532984364393, -6.376774720514410077, 19.42899254576129664 ) ) ;
#19064 = CARTESIAN_POINT ( 'NONE',  ( -4.704028875484805639, -20.06825252194306941, 11.49999999999999645 ) ) ;
#19065 = VECTOR ( 'NONE', #50328, 1000.000000000000114 ) ;
#19066 = DIRECTION ( 'NONE',  ( 0.000000000000000000, 0.000000000000000000, 1.000000000000000000 ) ) ;
#19067 = B_SPLINE_CURVE_WITH_KNOTS ( 'NONE', 3,
 ( #78376, #9374, #71286, #1774, #87001, #71790, #32712, #56575, #63696, #17490, #48456, #41850, #72791, #65695, #42846, #34227, #3293, #26106 ),
 .UNSPECIFIED., .F., .F.,
 ( 4, 2, 2, 2, 2, 2, 2, 2, 4 ),
 ( 0.000000000000000000, 0.1249999999999993894, 0.1874999999999992506, 0.2499999999999991118, 0.4999999999999995559, 0.7500000000000001110, 0.8125000000000001110, 0.8750000000000001110, 1.000000000000000000 ),
 .UNSPECIFIED. ) ;
#19068 = CARTESIAN_POINT ( 'NONE',  ( -6.316168294299441932, 21.79233575779346310, 11.49999999999999645 ) ) ;
#19069 = ORIENTED_EDGE ( 'NONE', *, *, #82072, .T. ) ;
#19070 = CARTESIAN_POINT ( 'NONE',  ( -115.6228709571500417, -25.00182538069145721, 7.747789668545097541 ) ) ;
#19071 = CARTESIAN_POINT ( 'NONE',  ( -97.58474497804847658, -24.65952944569304961, 1.056160979905703456 ) ) ;
#19072 = AXIS2_PLACEMENT_3D ( 'NONE', #39002, #93280, #10054 ) ;
#19073 = ADVANCED_FACE ( 'NONE', ( #91948 ), #93948, .T. ) ;
#19074 = CYLINDRICAL_SURFACE ( 'NONE', #19211, 252.4458649670781085 ) ;
#19075 = FACE_OUTER_BOUND ( 'NONE', #66737, .T. ) ;
#19076 = ORIENTED_EDGE ( 'NONE', *, *, #61268, .F. ) ;
#19077 = CARTESIAN_POINT ( 'NONE',  ( -100.1661903510885452, -25.12553550024694360, 7.087413643504399730 ) ) ;
#19078 = CARTESIAN_POINT ( 'NONE',  ( -1.055347110731411187, -22.84297022578905612, -1.500000000000002220 ) ) ;
#19079 = DIRECTION ( 'NONE',  ( 0.000000000000000000, 0.000000000000000000, -1.000000000000000000 ) ) ;
#19080 = CARTESIAN_POINT ( 'NONE',  ( -113.6295968303889481, -23.73791477778912196, 11.05961554403170233 ) ) ;
#19081 = CARTESIAN_POINT ( 'NONE',  ( -63.49149983805614283, -24.66019654487200086, 8.947790411086119278 ) ) ;
#19082 = ADVANCED_FACE ( 'NONE', ( #47288 ), #78703, .T. ) ;
#19083 = CARTESIAN_POINT ( 'NONE',  ( -6.794891441663577503, 21.43730618243864683, 11.49999999999999645 ) ) ;
#19084 = ORIENTED_EDGE ( 'NONE', *, *, #93827, .T. ) ;
#19085 = CYLINDRICAL_SURFACE ( 'NONE', #82159, 3.060000000000000053 ) ;
#19086 = CARTESIAN_POINT ( 'NONE',  ( -11.46427080702723522, -18.74017919159951973, 11.49999999999998934 ) ) ;
#19087 = EDGE_CURVE ( 'NONE', #89410, #97387, #55687, .T. ) ;
#19088 = CARTESIAN_POINT ( 'NONE',  ( -111.5539232054254484, -24.15543982623907482, -0.2315651400026575712 ) ) ;
#19089 = CARTESIAN_POINT ( 'NONE',  ( -29.23483314410334444, -24.79699843522629976, 5.425067535242146022 ) ) ;
#19090 = ORIENTED_EDGE ( 'NONE', *, *, #70339, .T. ) ;
#19091 = CARTESIAN_POINT ( 'NONE',  ( -63.62287095715004881, -23.72773821059535493, 11.05748984161097503 ) ) ;
#19092 = CARTESIAN_POINT ( 'NONE',  ( -111.6228709571500559, -23.94994826722515668, -0.6494450866351696439 ) ) ;
#19093 = ORIENTED_EDGE ( 'NONE', *, *, #26231, .T. ) ;
#19094 = CARTESIAN_POINT ( 'NONE',  ( -77.62287095715005592, -23.94994826722515668, -0.6494450866351729745 ) ) ;
#19095 = CARTESIAN_POINT ( 'NONE',  ( -10.27258457790969892, -17.75692283049141196, 11.49999999999998934 ) ) ;
#19096 = EDGE_LOOP ( 'NONE', ( #17727, #35, #21318, #53269 ) ) ;
#19097 = ORIENTED_EDGE ( 'NONE', *, *, #49282, .F. ) ;
#19098 = EDGE_LOOP ( 'NONE', ( #26874, #39778, #73918 ) ) ;
#19099 = CARTESIAN_POINT ( 'NONE',  ( 2.935461252226840401, -6.376774720514420736, 20.47627681611744777 ) ) ;
#19100 = CARTESIAN_POINT ( 'NONE',  ( -0.07435467474217070938, 23.09247799282200475, -1.500000000000002220 ) ) ;
#19102 = ADVANCED_FACE ( 'NONE', ( #55913 ), #9209, .T. ) ;
#19101 = CARTESIAN_POINT ( 'NONE',  ( -104.5173939172612734, -23.96169478059714208, 10.65365249895717525 ) ) ;
#19103 = CARTESIAN_POINT ( 'NONE',  ( -13.67433444753018534, -15.09191755960682890, -1.500000000000002220 ) ) ;
#19104 = ORIENTED_EDGE ( 'NONE', *, *, #28845, .T. ) ;
#19105 = CIRCLE ( 'NONE', #80679, 1.836000000000000743 ) ;
#19106 = CARTESIAN_POINT ( 'NONE',  ( -1.041963229364719634, -5.876774720514417183, 20.24089781925592746 ) ) ;
#19107 = CARTESIAN_POINT ( 'NONE',  ( -29.51207664681304976, -23.65098756497642540, 11.05961561336856391 ) ) ;
#19108 = B_SPLINE_CURVE_WITH_KNOTS ( 'NONE', 3,
 ( #47896, #40773, #210, #33156, #17939, #3726 ),
 .UNSPECIFIED., .F., .F.,
 ( 4, 2, 4 ),
 ( 6.391158118961562613E-06, 0.001387004593080782460, 0.002767618028042603297 ),
 .UNSPECIFIED. ) ;
#19109 = CARTESIAN_POINT ( 'NONE',  ( -105.6261443220027445, -24.73486907724918282, 1.287355809206962576 ) ) ;
#19110 = CARTESIAN_POINT ( 'NONE',  ( -63.52287095715009002, -23.72773821059535848, 11.05748984161097503 ) ) ;
#19111 = VERTEX_POINT ( 'NONE', #79221 ) ;
#19112 = CARTESIAN_POINT ( 'NONE',  ( -29.23473450784903704, -24.76881327774048458, 4.453843528195366552 ) ) ;
#19113 = CARTESIAN_POINT ( 'NONE',  ( -90.22287095715005023, -23.47593901973090524, -1.443836447538996870 ) ) ;
#19114 = ORIENTED_EDGE ( 'NONE', *, *, #31662, .F. ) ;
#19115 = CARTESIAN_POINT ( 'NONE',  ( -18.78340662496949776, 8.880393494302802893, -1.500000000000002220 ) ) ;
#19116 = ORIENTED_EDGE ( 'NONE', *, *, #49854, .T. ) ;
#19118 = VERTEX_POINT ( 'NONE', #25441 ) ;
#19117 = CARTESIAN_POINT ( 'NONE',  ( -96.62287095715005592, -29.50250243563736774, 8.947779886222138046 ) ) ;
#19119 = B_SPLINE_SURFACE_WITH_KNOTS ( 'NONE', 3, 1, ( 
 ( #25309, #64409 ),
 ( #72500, #81099 ),
 ( #2994, #11580 ),
 ( #33931, #32428 ),
 ( #9591, #40550 ),
 ( #71502, #1989 ),
 ( #25816, #56287 ),
 ( #79597, #56786 ),
 ( #90578, #14441 ),
 ( #6832, #29678 ),
 ( #54029, #15440 ),
 ( #100155, #23035 ),
 ( #37792, #21057 ),
 ( #69237, #30168 ),
 ( #46400, #67761 ),
 ( #36799, #52027 ),
 ( #76826, #91569 ),
 ( #30673, #60649 ),
 ( #28684, #14939 ) ),
 .UNSPECIFIED., .F., .F., .F.,
 ( 4, 1, 1, 1, 1, 1, 1, 1, 1, 1, 1, 1, 1, 1, 1, 1, 4 ),
 ( 2, 2 ),
 ( 0.000000000000000000, 0.05733942592015824763, 0.1130633316232408925, 0.1691814487493780716, 0.2257745596549409484, 0.2838263038920837977, 0.3434542790864910655, 0.4059069615102774420, 0.4713922597696830752, 0.5380028337126923077, 0.6030635561963488822, 0.6676018307634233873, 0.7322254428169042706, 0.7970048098289836958, 0.8630479900344357747, 0.9303569870570429501, 1.000000000000000000 ),
 ( 0.000000000000000000, 1.000000000000000000 ),
 .UNSPECIFIED. ) ;
#19120 = FACE_OUTER_BOUND ( 'NONE', #73882, .T. ) ;
#19121 = CARTESIAN_POINT ( 'NONE',  ( -107.6228709571501412, -23.94994826722516379, -0.6494450866351700880 ) ) ;
#19122 = ORIENTED_EDGE ( 'NONE', *, *, #91704, .F. ) ;
#19123 = EDGE_LOOP ( 'NONE', ( #4288, #10005, #48926, #23859 ) ) ;
#19124 = LINE ( 'NONE', #50585, #28423 ) ;
#19125 = CARTESIAN_POINT ( 'NONE',  ( -116.6228709571500417, -24.51387760970724017, 9.387446482453407626 ) ) ;
#19127 = EDGE_CURVE ( 'NONE', #1891, #21831, #79723, .T. ) ;
#19126 = CARTESIAN_POINT ( 'NONE',  ( -74.62287095715004170, -23.94994826722566117, -0.6494450866342730277 ) ) ;
#19129 = ORIENTED_EDGE ( 'NONE', *, *, #21906, .F. ) ;
#19128 = CARTESIAN_POINT ( 'NONE',  ( 2.303347834742990763, 21.97011321758780866, 11.49999999999999645 ) ) ;
#19130 = CARTESIAN_POINT ( 'NONE',  ( -103.5574459519354065, -23.73766607897670156, -1.055555164236454901 ) ) ;
#19131 = CARTESIAN_POINT ( 'NONE',  ( 6.494847429386178206, -21.66115869805930672, 11.49999999999998934 ) ) ;
#19132 = AXIS2_PLACEMENT_3D ( 'NONE', #22641, #1339, #7934 ) ;
#19134 = ORIENTED_EDGE ( 'NONE', *, *, #86227, .T. ) ;
#19133 = CARTESIAN_POINT ( 'NONE',  ( -115.5872429041571650, -24.92592662359561473, 8.075495903017996469 ) ) ;
#19135 = EDGE_CURVE ( 'NONE', #59566, #89278, #48296, .T. ) ;
#19136 = EDGE_LOOP ( 'NONE', ( #28232, #27197, #61106, #64820 ) ) ;
#19137 = CARTESIAN_POINT ( 'NONE',  ( -7.160000000000000142, -6.754662360505033547, 8.925641719537455998 ) ) ;
#19138 = EDGE_CURVE ( 'NONE', #12730, #24728, #1219, .T. ) ;
#19139 = AXIS2_PLACEMENT_3D ( 'NONE', #19363, #55945, #80268 ) ;
#19140 = EDGE_CURVE ( 'NONE', #40087, #91590, #71125, .T. ) ;
#19141 = B_SPLINE_CURVE_WITH_KNOTS ( 'NONE', 3,
 ( #81673, #27880, #4559, #74064, #65977, #11157, #73073, #64979, #96896, #95893, #12146, #42133, #66481, #11649, #26388, #18274, #34003, #58838, #49743, #49245, #26885, #20255, #57359, #88291, #42626, #73564, #51223 ),
 .UNSPECIFIED., .F., .F.,
 ( 4, 1, 1, 1, 1, 1, 1, 1, 1, 1, 1, 1, 1, 1, 1, 1, 1, 1, 1, 1, 1, 1, 1, 1, 4 ),
 ( 0.000000000000000000, 0.06506328961727787796, 0.1267731664665228408, 0.1855157632260783507, 0.2407646791677146292, 0.2929797960235977494, 0.3422503727797667206, 0.3889192861856601846, 0.4327756640583091396, 0.4746284326311175361, 0.5147746906379525589, 0.5536058934984424695, 0.5914264064311723912, 0.6280281199460664432, 0.6638036341103201732, 0.6989843361316636638, 0.7335914893067054798, 0.7676284691511399139, 0.8012083477865917791, 0.8342638397266231021, 0.8669806947287760357, 0.8997197415181603652, 0.9327019124985379550, 0.9661758834327495160, 1.000000000000000000 ),
 .UNSPECIFIED. ) ;
#19142 = DIRECTION ( 'NONE',  ( 0.000000000000000000, 0.000000000000000000, 1.000000000000000000 ) ) ;
#19143 = ORIENTED_EDGE ( 'NONE', *, *, #94033, .T. ) ;
#19144 = CARTESIAN_POINT ( 'NONE',  ( 12.09327641706010326, 17.40255341615222306, 11.49999999999998934 ) ) ;
#19145 = VECTOR ( 'NONE', #31207, 1000.000000000000114 ) ;
#19146 = CARTESIAN_POINT ( 'NONE',  ( -6.815415664272417295, -6.376774720514410077, 19.46427715384223234 ) ) ;
#19147 = CARTESIAN_POINT ( 'NONE',  ( -80.62287095715008434, -24.83620972994592080, 8.398175272781369216 ) ) ;
#19148 = CARTESIAN_POINT ( 'NONE',  ( -2.790049085472659396, -22.09070898310802633, -1.500000000000002220 ) ) ;
#19149 = CARTESIAN_POINT ( 'NONE',  ( -49.87826110250815503, -25.03220892416941723, 7.497148264617506719 ) ) ;
#19150 = ORIENTED_EDGE ( 'NONE', *, *, #12338, .F. ) ;
#19151 = CARTESIAN_POINT ( 'NONE',  ( 8.462785143989153269, -3.316774720514427344, -28.02084008811334215 ) ) ;
#19152 = CARTESIAN_POINT ( 'NONE',  ( -48.58953762381671737, -24.65952944569304250, 1.056160979905691466 ) ) ;
#19153 = DIRECTION ( 'NONE',  ( -3.773278334453079618E-23, 0.9999999999976377785, 2.173523156925979975E-06 ) ) ;
#19154 = CARTESIAN_POINT ( 'NONE',  ( -1.358974358974357921, -6.376774720514420736, 20.75510817307693046 ) ) ;
#19155 = CARTESIAN_POINT ( 'NONE',  ( 6.966380261627926451, -18.21767524041069564, -1.500000000000002220 ) ) ;
#19156 = CARTESIAN_POINT ( 'NONE',  ( 19.99082695160776169, -7.785253749782737209, 11.49999999999998934 ) ) ;
#19157 = CARTESIAN_POINT ( 'NONE',  ( -26.15505896238250472, -24.57999669887485794, 2.424162796277344434 ) ) ;
#19158 = DIRECTION ( 'NONE',  ( 0.000000000000000000, 2.173523156925980399E-06, -0.9999999999976378895 ) ) ;
#19159 = CARTESIAN_POINT ( 'NONE',  ( -77.63799161339106547, -23.96119346886880663, -0.6495511937832126881 ) ) ;
#19160 = CARTESIAN_POINT ( 'NONE',  ( 18.68554041145753786, -12.99315341008173519, -1.500000000000002220 ) ) ;
#19161 = ADVANCED_FACE ( 'NONE', ( #8222 ), #1618, .T. ) ;
#19162 = DIRECTION ( 'NONE',  ( -3.498155634913392171E-15, 0.0002585596332610844150, -0.9999999665734575771 ) ) ;
#19163 = FACE_OUTER_BOUND ( 'NONE', #45316, .T. ) ;
#19164 = CARTESIAN_POINT ( 'NONE',  ( -65.05438548721848235, -3.316774720514426456, 29.49402280011861777 ) ) ;
#19165 = CARTESIAN_POINT ( 'NONE',  ( -14.97016004668225264, 13.15154794113874637, 11.49999999999999645 ) ) ;
#19166 = CARTESIAN_POINT ( 'NONE',  ( -104.5599225995679404, -23.48783264082477373, -1.443836473390085695 ) ) ;
#19167 = EDGE_CURVE ( 'NONE', #50221, #55102, #93439, .T. ) ;
#19168 = DIRECTION ( 'NONE',  ( 0.000000000000000000, -1.478457507934778393E-16, -1.000000000000000000 ) ) ;
#19169 = FACE_OUTER_BOUND ( 'NONE', #3533, .T. ) ;
#19170 = VERTEX_POINT ( 'NONE', #86344 ) ;
#19171 = DIRECTION ( 'NONE',  ( 0.000000000000000000, -1.000000000000000000, 0.000000000000000000 ) ) ;
#19172 = CARTESIAN_POINT ( 'NONE',  ( -32.42034289422212368, -24.87219037988794312, 1.747789950295619787 ) ) ;
#19173 = CARTESIAN_POINT ( 'NONE',  ( 14.13103794885040898, -16.47871000921984219, -1.500000000000002220 ) ) ;
#19174 = EDGE_CURVE ( 'NONE', #32707, #93325, #2621, .T. ) ;
#19175 = CARTESIAN_POINT ( 'NONE',  ( -56.50279899131798089, -24.15620529776628445, 10.23563542870660648 ) ) ;
#19176 = CARTESIAN_POINT ( 'NONE',  ( -15.27948257512286645, 12.15582775940324822, -1.500000000000002220 ) ) ;
#19177 = EDGE_CURVE ( 'NONE', #51486, #52686, #9145, .T. ) ;
#19178 = CARTESIAN_POINT ( 'NONE',  ( -55.49531503891194717, -24.40133493613049964, 9.663955038902800609 ) ) ;
#19179 = B_SPLINE_CURVE_WITH_KNOTS ( 'NONE', 3,
 ( #97928, #81225, #26939, #88850 ),
 .UNSPECIFIED., .F., .F.,
 ( 4, 4 ),
 ( 0.2089094642748469122, 0.2099102113156124105 ),
 .UNSPECIFIED. ) ;
#19180 = VERTEX_POINT ( 'NONE', #16324 ) ;
#19181 = APPROVAL_DATE_TIME ( #95810, #28897 ) ;
#19182 = CARTESIAN_POINT ( 'NONE',  ( -25.92875734969025814, -3.316774720514426456, 0.7300228001186309656 ) ) ;
#19183 = CARTESIAN_POINT ( 'NONE',  ( 16.50020720150075348, -12.08490501797973238, 11.49999999999999645 ) ) ;
#19184 = DIRECTION ( 'NONE',  ( 3.773278334444167608E-23, -1.000000000000000000, 0.000000000000000000 ) ) ;
#19185 = DIRECTION ( 'NONE',  ( 3.773278334444167608E-23, -1.000000000000000000, 0.000000000000000000 ) ) ;
#19186 = ORIENTED_EDGE ( 'NONE', *, *, #99289, .F. ) ;
#19187 = CARTESIAN_POINT ( 'NONE',  ( -55.55620429048339304, -23.48786465467241058, 11.44779295918254469 ) ) ;
#19188 = CARTESIAN_POINT ( 'NONE',  ( -39.48699591144466581, -25.28892559316353683, 3.925286840877467487 ) ) ;
#19189 = FACE_OUTER_BOUND ( 'NONE', #9148, .T. ) ;
#19190 = FACE_OUTER_BOUND ( 'NONE', #36760, .T. ) ;
#19191 = EDGE_CURVE ( 'NONE', #44968, #60374, #27810, .T. ) ;
#19192 = CARTESIAN_POINT ( 'NONE',  ( 282.9764569301858046, -1.682774720514426114, 20.79159422840526616 ) ) ;
#19193 = ORIENTED_EDGE ( 'NONE', *, *, #81113, .T. ) ;
#19194 = CARTESIAN_POINT ( 'NONE',  ( 6.127395130496778641, -6.376774720514417183, 20.13872869980892943 ) ) ;
#19195 = VECTOR ( 'NONE', #28047, 1000.000000000000114 ) ;
#19196 = CARTESIAN_POINT ( 'NONE',  ( 3.160899137004691717, 22.77513019406404382, 11.49999999999999645 ) ) ;
#19197 = CARTESIAN_POINT ( 'NONE',  ( 22.69831151501224298, -1.600861625767590724, 11.49999999999998934 ) ) ;
#19198 = CARTESIAN_POINT ( 'NONE',  ( 4.967622410992271753, -6.376774720514415407, 20.05703257908297843 ) ) ;
#19199 = LINE ( 'NONE', #20694, #67470 ) ;
#19200 = CARTESIAN_POINT ( 'NONE',  ( -81.52287095715009002, -23.72773821059537269, 11.05748984161097503 ) ) ;
#19201 = CARTESIAN_POINT ( 'NONE',  ( -78.55620429048339304, -23.48786465467241058, 11.44779295918254469 ) ) ;
#19202 = CARTESIAN_POINT ( 'NONE',  ( 0.000000000000000000, 1.477225279485574028, 19.84760796525321425 ) ) ;
#19203 = CARTESIAN_POINT ( 'NONE',  ( -15.17958814119055155, -15.74432251006154715, -1.500000000000002220 ) ) ;
#19204 = ADVANCED_FACE ( 'NONE', ( #3621 ), #41688, .T. ) ;
#19205 = CARTESIAN_POINT ( 'NONE',  ( -74.52287095715007581, -23.72747288104470087, -1.053458166803227014 ) ) ;
#19206 = EDGE_CURVE ( 'NONE', #49156, #98244, #74121, .T. ) ;
#19207 = CARTESIAN_POINT ( 'NONE',  ( -55.52287095715005449, -24.99132157543083821, 2.256160258750667502 ) ) ;
#19208 = LINE ( 'NONE', #66419, #9590 ) ;
#19209 = LINE ( 'NONE', #66910, #63118 ) ;
#19210 = ORIENTED_EDGE ( 'NONE', *, *, #61754, .T. ) ;
#19211 = AXIS2_PLACEMENT_3D ( 'NONE', #56664, #19573, #41937 ) ;
#19212 = CARTESIAN_POINT ( 'NONE',  ( -20.42006937447004233, 0.3101567295262241952, -1.500000000000002220 ) ) ;
#19213 = ORIENTED_EDGE ( 'NONE', *, *, #75882, .F. ) ;
#19214 = ORIENTED_EDGE ( 'NONE', *, *, #98707, .F. ) ;
#19215 = ORIENTED_EDGE ( 'NONE', *, *, #63310, .F. ) ;
#19216 = ORIENTED_EDGE ( 'NONE', *, *, #44188, .T. ) ;
#19217 = CARTESIAN_POINT ( 'NONE',  ( 22.97298546869389568, 1.202750762487129199, -1.500000000000002220 ) ) ;
#19219 = ADVANCED_FACE ( 'NONE', ( #34065 ), #26455, .F. ) ;
#19218 = CARTESIAN_POINT ( 'NONE',  ( -6.752792875861700850, -5.876774720514411854, 19.46247113826586528 ) ) ;
#19220 = CARTESIAN_POINT ( 'NONE',  ( 9.409760114191467295, 17.86087837679851020, -1.500000000000002220 ) ) ;
#19221 = EDGE_LOOP ( 'NONE', ( #88281, #98190, #46964, #96349 ) ) ;
#19222 = PLANE ( 'NONE',  #88206 ) ;
#19223 = CARTESIAN_POINT ( 'NONE',  ( 29.80070917940689412, -6.475225279485573360, 27.39560796525321607 ) ) ;
#19224 = EDGE_CURVE ( 'NONE', #47870, #53939, #43182, .T. ) ;
#19225 = ADVANCED_FACE ( 'NONE', ( #27455 ), #57913, .F. ) ;
#19226 = FACE_OUTER_BOUND ( 'NONE', #93246, .T. ) ;
#19227 = CARTESIAN_POINT ( 'NONE',  ( -53.50201011555726893, -24.15620529776627734, 10.23563542870660825 ) ) ;
#19228 = AXIS2_PLACEMENT_3D ( 'NONE', #29546, #6210, #28066 ) ;
#19230 = ORIENTED_EDGE ( 'NONE', *, *, #36492, .F. ) ;
#19229 = CARTESIAN_POINT ( 'NONE',  ( 12.02608574658498597, -17.65016651952024063, 11.49999999999999645 ) ) ;
#19231 = CARTESIAN_POINT ( 'NONE',  ( -78.62287095715005592, -23.47596703998600631, 11.44779298504227860 ) ) ;
#19232 = ORIENTED_EDGE ( 'NONE', *, *, #9909, .T. ) ;
#19233 = CARTESIAN_POINT ( 'NONE',  ( 21.27325221474336914, 6.521069146585026566, -1.500000000000002220 ) ) ;
#19234 = CARTESIAN_POINT ( 'NONE',  ( -20.55277978778089576, -2.218614319624547360, 11.49999999999998934 ) ) ;
#19235 = ORIENTED_EDGE ( 'NONE', *, *, #19438, .F. ) ;
#19236 = CARTESIAN_POINT ( 'NONE',  ( 3.085011456917871264, -5.876774720514409189, 19.00082519311127172 ) ) ;
#19237 = ORIENTED_EDGE ( 'NONE', *, *, #44663, .T. ) ;
#19238 = DIRECTION ( 'NONE',  ( -0.000000000000000000, -1.000000000000000000, -0.000000000000000000 ) ) ;
#19239 = ORIENTED_EDGE ( 'NONE', *, *, #63421, .F. ) ;
#19240 = CARTESIAN_POINT ( 'NONE',  ( -50.04601614386864838, -25.27517885246146534, 2.868514059739770250 ) ) ;
#19241 = CARTESIAN_POINT ( 'NONE',  ( -19.94816486946033507, 6.322790147265108018, -1.500000000000002220 ) ) ;
#19242 = CARTESIAN_POINT ( 'NONE',  ( -21.91604229967229500, -0.6759211909499470705, 11.49999999999999645 ) ) ;
#19243 = PLANE ( 'NONE',  #67404 ) ;
#19244 = CARTESIAN_POINT ( 'NONE',  ( -21.69688529672534827, 6.072505851105969299, 11.49999999999998934 ) ) ;
#19245 = CARTESIAN_POINT ( 'NONE',  ( 5.463070048063013218, -20.23478146675526190, 11.49999999999998934 ) ) ;
#19246 = CARTESIAN_POINT ( 'NONE',  ( -26.22762954581084571, -24.97067058367230175, 6.176716003714248338 ) ) ;
#19247 = CARTESIAN_POINT ( 'NONE',  ( 5.730633878096764278, -5.876774720514418071, 20.45679216967608838 ) ) ;
#19248 = CARTESIAN_POINT ( 'NONE',  ( 6.660000000000001030, 9.283009703645923594, -0.8121581124701985344 ) ) ;
#19249 = CYLINDRICAL_SURFACE ( 'NONE', #60535, 91.74549126261076992 ) ;
#19250 = EDGE_LOOP ( 'NONE', ( #92920, #97836, #92029, #45523 ) ) ;
#19251 = ORIENTED_EDGE ( 'NONE', *, *, #24275, .T. ) ;
#19252 = ORIENTED_EDGE ( 'NONE', *, *, #36833, .F. ) ;
#19253 = CARTESIAN_POINT ( 'NONE',  ( -52.51446550490977927, -23.73766607897671577, -1.055555164236436472 ) ) ;
#19254 = VERTEX_POINT ( 'NONE', #11221 ) ;
#19255 = CARTESIAN_POINT ( 'NONE',  ( 17.49997855696484095, 12.48231381050728928, -1.500000000000002220 ) ) ;
#19256 = ORIENTED_EDGE ( 'NONE', *, *, #8060, .T. ) ;
#19257 = DIRECTION ( 'NONE',  ( 0.000000000000000000, 1.000000000000000000, 0.000000000000000000 ) ) ;
#19258 = CARTESIAN_POINT ( 'NONE',  ( -6.733481718715807141, 19.98004043397084928, -1.500000000000002220 ) ) ;
#19259 = CARTESIAN_POINT ( 'NONE',  ( -60.58953762381671027, -25.00182538069145011, 7.747789668545099317 ) ) ;
#19260 = CARTESIAN_POINT ( 'NONE',  ( 0.000000000000000000, 0.000000000000000000, 0.000000000000000000 ) ) ;
#19262 = CARTESIAN_POINT ( 'NONE',  ( -87.62287095715004170, -24.65952944569304606, 1.056160979905700348 ) ) ;
#19261 = VECTOR ( 'NONE', #60355, 1000.000000000000114 ) ;
#19263 = CARTESIAN_POINT ( 'NONE',  ( -101.5168375974609063, -23.96119346886880663, -0.6495511937832049165 ) ) ;
#19264 = CARTESIAN_POINT ( 'NONE',  ( -51.55620429048340014, -23.48786465467241058, 11.44779295918254647 ) ) ;
#19265 = CARTESIAN_POINT ( 'NONE',  ( -13.14421341422731260, -17.72855101262432242, -1.500000000000002220 ) ) ;
#19266 = EDGE_LOOP ( 'NONE', ( #58596, #42952, #28453, #50935 ) ) ;
#19267 = CARTESIAN_POINT ( 'NONE',  ( -116.5222328135519518, -23.48783264082478439, -1.443836473390061936 ) ) ;
#19268 = CARTESIAN_POINT ( 'NONE',  ( -23.24941632505786870, 6.376774720514426953, 27.45402280011862572 ) ) ;
#19269 = CARTESIAN_POINT ( 'NONE',  ( -41.56322468833811712, -25.31624637032491165, 5.062029375606173609 ) ) ;
#19270 = AXIS2_PLACEMENT_3D ( 'NONE', #39327, #93111, #268 ) ;
#19271 = CARTESIAN_POINT ( 'NONE',  ( -26.95684302982099467, -24.86038313398945476, 2.662461283694073089 ) ) ;
#19273 = CARTESIAN_POINT ( 'NONE',  ( -63.52287095715010423, -24.34917612406836795, 0.1852690917426547679 ) ) ;
#19272 = AXIS2_PLACEMENT_3D ( 'NONE', #88959, #11330, #74227 ) ;
#19274 = CARTESIAN_POINT ( 'NONE',  ( -5.188002292566340934, -20.72503599944539587, 11.49999999999998934 ) ) ;
#19275 = CARTESIAN_POINT ( 'NONE',  ( -121.5562042904833504, -24.64965694238575367, 8.947790433994189385 ) ) ;
#19276 = CARTESIAN_POINT ( 'NONE',  ( -91.16087763667918864, -25.31973986624387862, 5.294390042787146200 ) ) ;
#19277 = CARTESIAN_POINT ( 'NONE',  ( -64.64730567560253860, -23.73791477778911840, 11.05961554403170766 ) ) ;
#19278 = CARTESIAN_POINT ( 'NONE',  ( -80.72042306966947933, -25.12719728850807499, 7.077500010625388249 ) ) ;
#19279 = CARTESIAN_POINT ( 'NONE',  ( 9.831018646898828095, -20.30805102056165623, -1.500000000000002220 ) ) ;
#19280 = ADVANCED_FACE ( 'NONE', ( #20311 ), #88857, .T. ) ;
#19281 = LINE ( 'NONE', #81192, #53922 ) ;
#19282 = ORIENTED_EDGE ( 'NONE', *, *, #80310, .T. ) ;
#19283 = CARTESIAN_POINT ( 'NONE',  ( 4.487249349319938574, -5.876774720514420736, 21.01618089687719504 ) ) ;
#19284 = CARTESIAN_POINT ( 'NONE',  ( -99.62287095715005592, -23.47593901973091235, -1.443836447539001089 ) ) ;
#19285 = CARTESIAN_POINT ( 'NONE',  ( 6.816645498261984848, 18.52099371530728789, 11.49999999999999645 ) ) ;
#19286 = CARTESIAN_POINT ( 'NONE',  ( -67.52287095715006160, -29.50248528299804818, 1.056150453629036701 ) ) ;
#19287 = VECTOR ( 'NONE', #19947, 1000.000000000000114 ) ;
#19288 = CARTESIAN_POINT ( 'NONE',  ( -119.5228709571500616, -23.48783264082477018, -1.443836473390082142 ) ) ;
#19289 = ORIENTED_EDGE ( 'NONE', *, *, #65073, .T. ) ;
#19290 = CARTESIAN_POINT ( 'NONE',  ( -42.58953762381671737, -23.47593901973091235, -1.443836447539011525 ) ) ;
#19291 = CARTESIAN_POINT ( 'NONE',  ( -29.79725469281722994, -24.60094484029862372, 4.359878766298754371 ) ) ;
#19293 = EDGE_CURVE ( 'NONE', #7634, #20357, #77392, .T. ) ;
#19292 = DIRECTION ( 'NONE',  ( 1.000000000000000000, 3.773278334444166432E-23, 8.201307841325785021E-29 ) ) ;
#19294 = CARTESIAN_POINT ( 'NONE',  ( -19.98381242416700587, 8.274006965216138099, 11.49999999999998934 ) ) ;
#19295 = ADVANCED_FACE ( 'NONE', ( #96454 ), #12704, .F. ) ;
#19296 = CARTESIAN_POINT ( 'NONE',  ( -126.6228709571500275, -23.95044443724993499, 10.65354141964649592 ) ) ;
#19297 = CARTESIAN_POINT ( 'NONE',  ( -101.5228709571500758, -23.48786465467241769, 11.44779295918254114 ) ) ;
#19298 = EDGE_CURVE ( 'NONE', #19368, #96700, #35565, .T. ) ;
#19299 = CARTESIAN_POINT ( 'NONE',  ( -92.55620429048337883, -23.48783264082478084, -1.443836473390063269 ) ) ;
#19300 = FACE_OUTER_BOUND ( 'NONE', #29863, .T. ) ;
#19301 = CARTESIAN_POINT ( 'NONE',  ( 10.99584971316270732, 16.45119811332560289, -1.500000000000002220 ) ) ;
#19302 = ORIENTED_EDGE ( 'NONE', *, *, #6831, .T. ) ;
#19303 = ADVANCED_FACE ( 'NONE', ( #50790 ), #42688, .T. ) ;
#19304 = CARTESIAN_POINT ( 'NONE',  ( 15.69265952521009488, -12.80212094623039576, 11.49999999999999645 ) ) ;
#19305 = CARTESIAN_POINT ( 'NONE',  ( 5.641575934020636396, -5.876774720514419847, 20.76276410292889096 ) ) ;
#19306 = CIRCLE ( 'NONE', #85729, 129.7684398600581517 ) ;
#19307 = ORIENTED_EDGE ( 'NONE', *, *, #19791, .F. ) ;
#19308 = CARTESIAN_POINT ( 'NONE',  ( 6.573941812937369455, 0.2639660507643281639, 9.334907998774166978E-16 ) ) ;
#19309 = DIRECTION ( 'NONE',  ( -3.773278334453079618E-23, 0.9999999999976377785, 2.173523156925979975E-06 ) ) ;
#19310 = DIRECTION ( 'NONE',  ( 0.8219392559241307517, 0.5637660281018075370, -0.08114015731558690825 ) ) ;
#19311 = CARTESIAN_POINT ( 'NONE',  ( -103.6228709571500559, -23.72773821059535493, 11.05748984161097681 ) ) ;
#19312 = DIRECTION ( 'NONE',  ( -1.000000000000000000, -0.000000000000000000, -0.000000000000000000 ) ) ;
#19313 = CARTESIAN_POINT ( 'NONE',  ( 17.53424486177994623, -9.724335930198575895, 11.49999999999998934 ) ) ;
#19314 = EDGE_CURVE ( 'NONE', #18354, #88212, #19815, .T. ) ;
#19315 = LINE ( 'NONE', #35057, #58063 ) ;
#19316 = ORIENTED_EDGE ( 'NONE', *, *, #18778, .T. ) ;
#19317 = B_SPLINE_CURVE_WITH_KNOTS ( 'NONE', 3,
 ( #52626, #90685, #53141, #21164 ),
 .UNSPECIFIED., .F., .F.,
 ( 4, 4 ),
 ( 0.2599715638078484714, 0.2689779950799639496 ),
 .UNSPECIFIED. ) ;
#19318 = ADVANCED_FACE ( 'NONE', ( #87849 ), #18333, .T. ) ;
#19319 = CARTESIAN_POINT ( 'NONE',  ( -73.62287095715005592, -24.64965695001468404, 8.947790433994184056 ) ) ;
#19320 = CARTESIAN_POINT ( 'NONE',  ( -124.6228709571500559, -29.50250243563736774, 8.947779886222134493 ) ) ;
#19321 = DIRECTION ( 'NONE',  ( 0.9701425001453318764, 0.2425356250363331356, 0.000000000000000000 ) ) ;
#19322 = CARTESIAN_POINT ( 'NONE',  ( -105.5228709571500616, -23.84047902841601996, -0.8780736468305707643 ) ) ;
#19323 = CARTESIAN_POINT ( 'NONE',  ( -73.51160046725669872, -23.96119346886880663, -0.6495511937832116889 ) ) ;
#19324 = EDGE_CURVE ( 'NONE', #99120, #50584, #72634, .T. ) ;
#19325 = CARTESIAN_POINT ( 'NONE',  ( -117.5228709571500758, -23.47596703998600631, 11.44779298504227860 ) ) ;
#19326 = B_SPLINE_CURVE_WITH_KNOTS ( 'NONE', 3,
 ( #28283, #51631, #59750, #5940 ),
 .UNSPECIFIED., .F., .F.,
 ( 4, 4 ),
 ( 0.000000000000000000, 9.999999999998897304E-05 ),
 .UNSPECIFIED. ) ;
#19327 = DIRECTION ( 'NONE',  ( 0.000000000000000000, 0.000000000000000000, -1.000000000000000000 ) ) ;
#19328 = ORIENTED_EDGE ( 'NONE', *, *, #63219, .T. ) ;
#19329 = VECTOR ( 'NONE', #15325, 1000.000000000000000 ) ;
#19330 = CARTESIAN_POINT ( 'NONE',  ( -13.46841296510753061, 15.22696965993213070, 11.49999999999998934 ) ) ;
#19331 = ORIENTED_EDGE ( 'NONE', *, *, #58844, .T. ) ;
#19332 = B_SPLINE_CURVE_WITH_KNOTS ( 'NONE', 3,
 ( #59071, #28606, #42362, #80897 ),
 .UNSPECIFIED., .F., .F.,
 ( 4, 4 ),
 ( 0.8210863176411906661, 0.8300927489133060888 ),
 .UNSPECIFIED. ) ;
#19333 = CARTESIAN_POINT ( 'NONE',  ( -2.941484630304247450, -22.72858670154147376, 11.49999999999998934 ) ) ;
#19334 = EDGE_CURVE ( 'NONE', #39695, #69684, #67724, .T. ) ;
#19335 = CARTESIAN_POINT ( 'NONE',  ( 31.61557479013512761, 6.410763075590563354, 26.52166531862750531 ) ) ;
#19336 = ORIENTED_EDGE ( 'NONE', *, *, #55821, .T. ) ;
#19337 = AXIS2_PLACEMENT_3D ( 'NONE', #66198, #5263, #97119 ) ;
#19338 = CARTESIAN_POINT ( 'NONE',  ( -49.12145562309674318, -25.27906036046082150, 4.198313730648785658 ) ) ;
#19339 = ADVANCED_FACE ( 'NONE', ( #28430 ), #61406, .F. ) ;
#19340 = CARTESIAN_POINT ( 'NONE',  ( -76.52287095715009002, -24.50216790748203977, 0.6166512839542565017 ) ) ;
#19341 = AXIS2_PLACEMENT_3D ( 'NONE', #100044, #84843, #60534 ) ;
#19342 = CARTESIAN_POINT ( 'NONE',  ( -90.52287095715006160, -24.99156044556202616, 7.747789690856173195 ) ) ;
#19343 = CARTESIAN_POINT ( 'NONE',  ( -21.21068194950259311, 0.7780057951688260642, 11.49999999999999645 ) ) ;
#19344 = CIRCLE ( 'NONE', #77644, 1.250000000000001110 ) ;
#19345 = CARTESIAN_POINT ( 'NONE',  ( -22.11188964843745453, -1.696007508606716341, 11.49999999999998934 ) ) ;
#19346 = CARTESIAN_POINT ( 'NONE',  ( 19.36870410414886479, 7.000668502413378569, -1.500000000000002220 ) ) ;
#19348 = EDGE_LOOP ( 'NONE', ( #56717, #52952, #94623, #87388 ) ) ;
#19347 = AXIS2_PLACEMENT_3D ( 'NONE', #87791, #39604, #23869 ) ;
#19349 = CARTESIAN_POINT ( 'NONE',  ( -41.64786393905067285, -23.96119346886880663, -0.6495511937831990323 ) ) ;
#19350 = ORIENTED_EDGE ( 'NONE', *, *, #83136, .F. ) ;
#19351 = CARTESIAN_POINT ( 'NONE',  ( -54.65090589817863531, -23.73766607897669445, -1.055555164236461563 ) ) ;
#19352 = CARTESIAN_POINT ( 'NONE',  ( -91.15361000704997707, -29.50249591506787894, 5.947779886229223045 ) ) ;
#19353 = VERTEX_POINT ( 'NONE', #13701 ) ;
#19354 = ORIENTED_EDGE ( 'NONE', *, *, #55210, .T. ) ;
#19355 = B_SPLINE_CURVE_WITH_KNOTS ( 'NONE', 3,
 ( #66508, #34534, #88825, #26917 ),
 .UNSPECIFIED., .F., .F.,
 ( 4, 4 ),
 ( 0.000000000000000000, 1.000000000000000000 ),
 .UNSPECIFIED. ) ;
#19356 = ORIENTED_EDGE ( 'NONE', *, *, #67881, .F. ) ;
#19357 = CARTESIAN_POINT ( 'NONE',  ( 0.3910256410256441884, -6.376774720514427841, 21.75000000000000000 ) ) ;
#19358 = CARTESIAN_POINT ( 'NONE',  ( -108.5895376238166961, -24.65952944569304961, 1.056160979905701014 ) ) ;
#19359 = CARTESIAN_POINT ( 'NONE',  ( -130.5728709571500588, -23.53198925593397917, 11.48393099501408976 ) ) ;
#19360 = CARTESIAN_POINT ( 'NONE',  ( 9.628234360240019996, 18.42577530400075858, -1.500000000000002220 ) ) ;
#19361 = CARTESIAN_POINT ( 'NONE',  ( 16.02445091669267185, 14.69945503153335764, 11.49999999999999645 ) ) ;
#19362 = ORIENTED_EDGE ( 'NONE', *, *, #59115, .T. ) ;
#19363 = CARTESIAN_POINT ( 'NONE',  ( 0.000000000000000000, 1.826774720514426464, 0.000000000000000000 ) ) ;
#19364 = LINE ( 'NONE', #74158, #28646 ) ;
#19365 = CARTESIAN_POINT ( 'NONE',  ( 22.03792223356247604, -4.036589945906135846, 11.49999999999998934 ) ) ;
#19366 = DIRECTION ( 'NONE',  ( 0.000000000000000000, 1.000000000000000000, 0.000000000000000000 ) ) ;
#19367 = CARTESIAN_POINT ( 'NONE',  ( 0.7734273019049007214, 3.892732205269316292, 1.700000000000006839 ) ) ;
#19368 = VERTEX_POINT ( 'NONE', #22804 ) ;
#19369 = DIRECTION ( 'NONE',  ( -0.09721092304694051167, 0.000000000000000000, 0.9952638024365005887 ) ) ;
#19370 = CARTESIAN_POINT ( 'NONE',  ( -85.62287095715004170, -24.99132157543083821, 2.256160258750667502 ) ) ;
#19371 = B_SPLINE_CURVE_WITH_KNOTS ( 'NONE', 3,
 ( #33893, #47632, #87179, #9054, #25779, #40005, #79059, #63872 ),
 .UNSPECIFIED., .F., .F.,
 ( 4, 2, 2, 4 ),
 ( -0.001240355328176776396, -0.0002398155169398860729, 0.0007607242942970042499, 0.002761803916770786630 ),
 .UNSPECIFIED. ) ;
#19372 = ORIENTED_EDGE ( 'NONE', *, *, #18311, .F. ) ;
#19373 = ORIENTED_EDGE ( 'NONE', *, *, #98934, .F. ) ;
#19374 = DIRECTION ( 'NONE',  ( 0.000000000000000000, -2.173523156925979552E-06, 0.9999999999976378895 ) ) ;
#19375 = ORIENTED_EDGE ( 'NONE', *, *, #28367, .T. ) ;
#19376 = CARTESIAN_POINT ( 'NONE',  ( -7.839647760473957838, 19.78794240023834661, -1.500000000000002220 ) ) ;
#19377 = ORIENTED_EDGE ( 'NONE', *, *, #45870, .F. ) ;
#19378 = CARTESIAN_POINT ( 'NONE',  ( -88.55141844598099965, -24.15543982623907127, -0.2315651400026634277 ) ) ;
#19379 = CARTESIAN_POINT ( 'NONE',  ( 3.267597511969735802, 21.59432767039258394, -1.500000000000002220 ) ) ;
#19380 = CARTESIAN_POINT ( 'NONE',  ( -52.61350461722388161, -23.48786465467240703, 11.44779295918255180 ) ) ;
#19381 = CARTESIAN_POINT ( 'NONE',  ( -10.49914784070103124, -20.09245350529190688, 11.49999999999998934 ) ) ;
#19382 = CARTESIAN_POINT ( 'NONE',  ( 7.480769230769231726, -6.376774720514420736, 20.77403846153845635 ) ) ;
#19383 = CARTESIAN_POINT ( 'NONE',  ( -35.62287095715004170, -24.82558206586143967, 1.605769216559445933 ) ) ;
#19384 = CARTESIAN_POINT ( 'NONE',  ( 9.711643268838683341, -19.58466107313252635, -1.500000000000002220 ) ) ;
#19385 = CARTESIAN_POINT ( 'NONE',  ( 6.996935307331598075, -6.376774720514424288, 21.22729008382901128 ) ) ;
#19386 = ORIENTED_EDGE ( 'NONE', *, *, #55786, .F. ) ;
#19387 = CARTESIAN_POINT ( 'NONE',  ( -13.89275734969026388, -5.965225279485572685, 31.02402280011862246 ) ) ;
#19388 = LINE ( 'NONE', #57480, #21616 ) ;
#19389 = EDGE_LOOP ( 'NONE', ( #67819, #25256, #81920, #40454 ) ) ;
#19390 = CARTESIAN_POINT ( 'NONE',  ( -32.52287095715006160, -23.72773821059535848, 11.05748984161097681 ) ) ;
#19391 = VERTEX_POINT ( 'NONE', #59394 ) ;
#19392 = CARTESIAN_POINT ( 'NONE',  ( -69.55126625704998844, -25.16221347177320666, 3.076695569926833684 ) ) ;
#19393 = CARTESIAN_POINT ( 'NONE',  ( -110.5228709571500616, -23.48783264082477018, -1.443836473390086583 ) ) ;
#19394 = CARTESIAN_POINT ( 'NONE',  ( -21.26230640008892792, -0.7210608269398429693, -1.500000000000002220 ) ) ;
#19395 = CARTESIAN_POINT ( 'NONE',  ( -125.5228709571500616, -25.00182538069146077, 7.747789668545104647 ) ) ;
#19396 = CARTESIAN_POINT ( 'NONE',  ( -26.36141581567544989, -24.97064619426896215, 3.275177712619341541 ) ) ;
#19397 = AXIS2_PLACEMENT_3D ( 'NONE', #32896, #33383, #31893 ) ;
#19398 = CARTESIAN_POINT ( 'NONE',  ( -85.55307269276684679, -24.15503026093913519, -0.2815557561904480921 ) ) ;
#19399 = CARTESIAN_POINT ( 'NONE',  ( -84.62287095715007013, -23.73934037231757443, 11.05740245334328620 ) ) ;
#19400 = CARTESIAN_POINT ( 'NONE',  ( -79.62287095715004170, -23.47596703998600631, 11.44779298504227860 ) ) ;
#19401 = EDGE_LOOP ( 'NONE', ( #128, #62644, #93221, #25838 ) ) ;
#19402 = EDGE_CURVE ( 'NONE', #18934, #3335, #81009, .T. ) ;
#19403 = CARTESIAN_POINT ( 'NONE',  ( -15.85469643196389278, -11.46343829903102396, 11.49999999999999645 ) ) ;
#19404 = CARTESIAN_POINT ( 'NONE',  ( -108.5228709571500616, -23.47596703998600631, 11.44779298504228038 ) ) ;
#19405 = VECTOR ( 'NONE', #34840, 1000.000000000000000 ) ;
#19406 = EDGE_CURVE ( 'NONE', #78138, #71524, #28940, .T. ) ;
#19407 = CARTESIAN_POINT ( 'NONE',  ( -29.26213830025908180, -24.96129339002881409, 7.420498735244676958 ) ) ;
#19408 = ORIENTED_EDGE ( 'NONE', *, *, #487, .T. ) ;
#19409 = EDGE_CURVE ( 'NONE', #78997, #81513, #46170, .T. ) ;
#19410 = CARTESIAN_POINT ( 'NONE',  ( -78.52287095715006160, -23.47596703998600631, 11.44779298504228571 ) ) ;
#19411 = CARTESIAN_POINT ( 'NONE',  ( -99.74640623490535063, -25.25095820245264733, 5.397458776702524830 ) ) ;
#19412 = AXIS2_PLACEMENT_3D ( 'NONE', #25506, #48860, #81293 ) ;
#19413 = ADVANCED_FACE ( 'NONE', ( #53789 ), #15211, .T. ) ;
#19414 = CARTESIAN_POINT ( 'NONE',  ( -109.6228709571500559, -23.47593901973091235, -1.443836447538999312 ) ) ;
#19415 = CARTESIAN_POINT ( 'NONE',  ( -60.52287095715007581, -24.52232992886362695, 0.6492154411905999289 ) ) ;
#19416 = CARTESIAN_POINT ( 'NONE',  ( 13.13437215454093199, 14.66711140016434278, -1.500000000000002220 ) ) ;
#19417 = VECTOR ( 'NONE', #88880, 1000.000000000000000 ) ;
#19418 = VERTEX_POINT ( 'NONE', #69001 ) ;
#19419 = B_SPLINE_CURVE_WITH_KNOTS ( 'NONE', 3,
 ( #95931, #63000, #10197, #18312 ),
 .UNSPECIFIED., .F., .F.,
 ( 4, 4 ),
 ( 0.000000000000000000, 9.999999999998897304E-05 ),
 .UNSPECIFIED. ) ;
#19420 = AXIS2_PLACEMENT_3D ( 'NONE', #77201, #90450, #69103 ) ;
#19421 = LINE ( 'NONE', #18917, #29409 ) ;
#19422 = DIRECTION ( 'NONE',  ( 0.6599726524652352877, 0.000000000000000000, -0.7512896232465891000 ) ) ;
#19423 = VECTOR ( 'NONE', #43378, 1000.000000000000000 ) ;
#19424 = CALENDAR_DATE ( 2026, 9, 10 ) ;
#19425 = ORIENTED_EDGE ( 'NONE', *, *, #96289, .T. ) ;
#19426 = CARTESIAN_POINT ( 'NONE',  ( -74.52287095715009002, -23.96127896941631974, -0.6493128931038065765 ) ) ;
#19427 = CARTESIAN_POINT ( 'NONE',  ( -126.2228709571500644, -23.47593901973090524, -1.443836447538996204 ) ) ;
#19428 = FACE_OUTER_BOUND ( 'NONE', #92845, .T. ) ;
#19429 = CARTESIAN_POINT ( 'NONE',  ( -118.5893591438163526, -24.34968618360934300, 0.1864209137778906622 ) ) ;
#19430 = CARTESIAN_POINT ( 'NONE',  ( -78.92810380439237861, -25.14083923594767356, 2.947789366383930520 ) ) ;
#19431 = CARTESIAN_POINT ( 'NONE',  ( -76.22287095715006444, -23.47596703998600631, 11.44779298504227683 ) ) ;
#19432 = LINE ( 'NONE', #73721, #4065 ) ;
#19433 = CARTESIAN_POINT ( 'NONE',  ( 4.608267332293128682, -19.41724391825443874, 11.49999999999998934 ) ) ;
#19434 = CARTESIAN_POINT ( 'NONE',  ( -0.09684473721908999633, -21.79626877218119319, 10.45301531419930896 ) ) ;
#19435 = CARTESIAN_POINT ( 'NONE',  ( 9.006517291608927778, -17.75031788249398446, -1.500000000000002220 ) ) ;
#19436 = ORIENTED_EDGE ( 'NONE', *, *, #47785, .T. ) ;
#19437 = CARTESIAN_POINT ( 'NONE',  ( -71.52287095715009002, -24.50216790748204687, 0.6166512839542508395 ) ) ;
#19438 = EDGE_CURVE ( 'NONE', #84636, #31830, #14061, .T. ) ;
#19439 = DIRECTION ( 'NONE',  ( 1.000000000000000000, 0.000000000000000000, 0.000000000000000000 ) ) ;
#19440 = CARTESIAN_POINT ( 'NONE',  ( 8.422997646657599091, -6.376774720514429617, -25.04887774224060237 ) ) ;
#19441 = CARTESIAN_POINT ( 'NONE',  ( -20.31193019649481357, 4.361987795224258946, 11.49999999999999645 ) ) ;
#19442 = CARTESIAN_POINT ( 'NONE',  ( -37.62287095715005592, -23.47593901973091235, -1.443836447539011525 ) ) ;
#19443 = FACE_OUTER_BOUND ( 'NONE', #38362, .T. ) ;
#19444 = VERTEX_POINT ( 'NONE', #84214 ) ;
#19445 = DIRECTION ( 'NONE',  ( -0.000000000000000000, 1.000000000000000000, -0.000000000000000000 ) ) ;
#19446 = FACE_OUTER_BOUND ( 'NONE', #45459, .T. ) ;
#19447 = ORIENTED_EDGE ( 'NONE', *, *, #78705, .F. ) ;
#19448 = CARTESIAN_POINT ( 'NONE',  ( 17.32893120472914816, 10.46255702124672027, -1.500000000000002220 ) ) ;
#19449 = CARTESIAN_POINT ( 'NONE',  ( -55.55620429048338593, -25.00158670708909270, 2.256160236439165967 ) ) ;
#19450 = CARTESIAN_POINT ( 'NONE',  ( -53.62287095715005592, -24.64898659630528499, 1.056161002820821038 ) ) ;
#19451 = CARTESIAN_POINT ( 'NONE',  ( 21.57151214508649772, 3.625915217019311583E-15, 0.5000000000000000000 ) ) ;
#19453 = EDGE_LOOP ( 'NONE', ( #99635, #71137, #81429, #88868 ) ) ;
#19452 = EDGE_CURVE ( 'NONE', #80644, #74508, #79729, .T. ) ;
#19454 = CARTESIAN_POINT ( 'NONE',  ( -80.36322839271868190, -25.31553952166217414, 4.968560711380208161 ) ) ;
#19455 = DIRECTION ( 'NONE',  ( -1.000000000000000000, -3.773278334444166432E-23, -8.201307841325785021E-29 ) ) ;
#19456 = CARTESIAN_POINT ( 'NONE',  ( 9.011679573027636891, 17.89655708981447901, -1.500000000000002220 ) ) ;
#19457 = CARTESIAN_POINT ( 'NONE',  ( -20.73700405699343463, 3.470425206167693233, 11.49999999999999645 ) ) ;
#19458 = DIRECTION ( 'NONE',  ( -1.607395343451207646E-13, 0.000000000000000000, -1.000000000000000000 ) ) ;
#19459 = DIRECTION ( 'NONE',  ( -0.000000000000000000, 1.000000000000000000, -0.000000000000000000 ) ) ;
#19460 = CARTESIAN_POINT ( 'NONE',  ( -17.89045161427552699, -12.92718102017995641, -1.500000000000002220 ) ) ;
#19461 = B_SPLINE_CURVE_WITH_KNOTS ( 'NONE', 3,
 ( #32542, #63514, #9707, #94434 ),
 .UNSPECIFIED., .F., .F.,
 ( 4, 4 ),
 ( 0.5201573561134056334, 0.5291637873855210561 ),
 .UNSPECIFIED. ) ;
#19463 = EDGE_CURVE ( 'NONE', #79914, #14468, #95369, .T. ) ;
#19462 = CIRCLE ( 'NONE', #32441, 129.7684398600581517 ) ;
#19464 = CARTESIAN_POINT ( 'NONE',  ( 11.22434917415779054, 4.132774715458839232, -26.87660878605755599 ) ) ;
#19465 = CARTESIAN_POINT ( 'NONE',  ( -47.62287095715005592, -23.94994826722565762, -0.6494450866342735829 ) ) ;
#19466 = DIRECTION ( 'NONE',  ( 0.000000000000000000, 0.000000000000000000, -1.000000000000000000 ) ) ;
#19467 = CARTESIAN_POINT ( 'NONE',  ( 0.000000000000000000, 1.477225279485574028, 0.000000000000000000 ) ) ;
#19468 = DIRECTION ( 'NONE',  ( 0.000000000000000000, 0.000000000000000000, 1.000000000000000000 ) ) ;
#19469 = VERTEX_POINT ( 'NONE', #82721 ) ;
#19470 = AXIS2_PLACEMENT_3D ( 'NONE', #56565, #95607, #27097 ) ;
#19471 = ORIENTED_EDGE ( 'NONE', *, *, #44281, .F. ) ;
#19472 = CARTESIAN_POINT ( 'NONE',  ( 11.98973536156539943, 2.682774720514426559, -26.26140391504922178 ) ) ;
#19473 = CARTESIAN_POINT ( 'NONE',  ( -81.52287095715006160, -23.47596703998600631, 11.44779298504228571 ) ) ;
#19474 = PLANE ( 'NONE',  #58479 ) ;
#19475 = CARTESIAN_POINT ( 'NONE',  ( -20.56140336115741718, 0.6910293267889283664, -1.500000000000002220 ) ) ;
#19476 = CARTESIAN_POINT ( 'NONE',  ( 10.28227983848843152, -18.94921665015282031, 11.49999999999999645 ) ) ;
#19478 = ORIENTED_EDGE ( 'NONE', *, *, #38773, .F. ) ;
#19477 = AXIS2_PLACEMENT_3D ( 'NONE', #98433, #35564, #59906 ) ;
#19479 = DIRECTION ( 'NONE',  ( -0.000000000000000000, 1.000000000000000000, -0.000000000000000000 ) ) ;
#19480 = CARTESIAN_POINT ( 'NONE',  ( 6.431189903846153300, -5.876774720514424288, 20.08974358974358765 ) ) ;
#19481 = CARTESIAN_POINT ( 'NONE',  ( -87.62287095715004170, -29.50250786944525672, 11.44777988621623344 ) ) ;
#19482 = CARTESIAN_POINT ( 'NONE',  ( -20.85237562250380350, -7.973873963886685345, 11.49999999999998934 ) ) ;
#19483 = CARTESIAN_POINT ( 'NONE',  ( -82.62287095715007013, -24.66019654487199375, 8.947790411086128159 ) ) ;
#19484 = LINE ( 'NONE', #57576, #20515 ) ;
#19485 = EDGE_LOOP ( 'NONE', ( #57440, #60577, #65356, #92175, #61421, #904, #67312, #41126, #12056, #91928, #89631, #20094, #49599, #26550, #89544, #99507, #72265, #59669 ) ) ;
#19486 = CARTESIAN_POINT ( 'NONE',  ( 33.08751910920749140, -4.671536413567966228, -11.65282283138775377 ) ) ;
#19487 = AXIS2_PLACEMENT_3D ( 'NONE', #57241, #57733, #95779 ) ;
#19488 = LINE ( 'NONE', #51949, #2161 ) ;
#19489 = VECTOR ( 'NONE', #43570, 1000.000000000000114 ) ;
#19490 = B_SPLINE_CURVE_WITH_KNOTS ( 'NONE', 3,
 ( #67866, #5947, #37412, #19671, #68358, #21168, #4473 ),
 .UNSPECIFIED., .F., .F.,
 ( 4, 1, 1, 1, 4 ),
 ( 0.000000000000000000, 0.2537340756906634187, 0.5030351201318574716, 0.7500135973308806880, 1.000000000000000000 ),
 .UNSPECIFIED. ) ;
#19491 = CARTESIAN_POINT ( 'NONE',  ( 15.14581745102402088, -14.33592658440916523, -1.500000000000002220 ) ) ;
#19492 = ORIENTED_EDGE ( 'NONE', *, *, #41328, .T. ) ;
#19494 = ORIENTED_EDGE ( 'NONE', *, *, #16136, .F. ) ;
#19493 = CARTESIAN_POINT ( 'NONE',  ( 15.22325621495362391, -2.682774720514426559, -27.23549315679322547 ) ) ;
#19495 = ORIENTED_EDGE ( 'NONE', *, *, #80963, .T. ) ;
#19496 = CIRCLE ( 'NONE', #47110, 6.099999999999999645 ) ;
#19497 = CARTESIAN_POINT ( 'NONE',  ( -51.07434835877342749, -25.29404817037084285, 4.468853319241254063 ) ) ;
#19498 = CARTESIAN_POINT ( 'NONE',  ( 21.04674311342985860, -0.3259866984596996864, -1.500000000000002220 ) ) ;
#19499 = AXIS2_PLACEMENT_3D ( 'NONE', #54672, #1881, #9485 ) ;
#19500 = VERTEX_POINT ( 'NONE', #13197 ) ;
#19501 = CARTESIAN_POINT ( 'NONE',  ( -95.92287095715009571, -23.47593901973090880, -1.443836447538997314 ) ) ;
#19502 = FACE_OUTER_BOUND ( 'NONE', #62883, .T. ) ;
#19503 = CARTESIAN_POINT ( 'NONE',  ( -120.6235064687828356, -25.00182538069146787, 7.747789668545044250 ) ) ;
#19504 = CARTESIAN_POINT ( 'NONE',  ( -28.58953762381673158, -23.31696865966051391, -1.443835777057014047 ) ) ;
#19505 = CARTESIAN_POINT ( 'NONE',  ( -84.22287095715007865, -23.47593901973090169, -1.443836447538996870 ) ) ;
#19506 = CARTESIAN_POINT ( 'NONE',  ( -14.78470843206283902, -15.91074852019131924, -1.500000000000002220 ) ) ;
#19507 = DIRECTION ( 'NONE',  ( 0.000000000000000000, 0.000000000000000000, 1.000000000000000000 ) ) ;
#19509 = EDGE_LOOP ( 'NONE', ( #31609, #20458, #8914, #91490 ) ) ;
#19508 = CARTESIAN_POINT ( 'NONE',  ( 20.70802603420765564, 8.137917507125113303, 11.49999999999999645 ) ) ;
#19510 = CARTESIAN_POINT ( 'NONE',  ( -50.72223433783125301, -25.31441730805603285, 5.237078674425484692 ) ) ;
#19511 = DIRECTION ( 'NONE',  ( 0.000000000000000000, 0.000000000000000000, 1.000000000000000000 ) ) ;
#19512 = CARTESIAN_POINT ( 'NONE',  ( -100.6228709571500559, -23.47593901973091235, -1.443836447539001089 ) ) ;
#19513 = EDGE_LOOP ( 'NONE', ( #28852, #14871, #4433, #84115 ) ) ;
#19515 = EDGE_LOOP ( 'NONE', ( #67492, #81650, #70828, #97348 ) ) ;
#19514 = CARTESIAN_POINT ( 'NONE',  ( -53.92287095715006018, -23.47593901973090169, -1.443836447538997980 ) ) ;
#19516 = ORIENTED_EDGE ( 'NONE', *, *, #11877, .T. ) ;
#19517 = DIRECTION ( 'NONE',  ( -0.000000000000000000, 1.000000000000000000, -0.000000000000000000 ) ) ;
#19518 = CARTESIAN_POINT ( 'NONE',  ( -49.10647344728249664, -25.27836164187442236, 4.050120676592289470 ) ) ;
#19519 = CARTESIAN_POINT ( 'NONE',  ( -10.24059822343757808, -5.876774720514426953, 17.17691942396160698 ) ) ;
#19520 = CARTESIAN_POINT ( 'NONE',  ( -46.22287095715005734, -23.47596703998600631, 11.44779298504227683 ) ) ;
#19521 = ORIENTED_EDGE ( 'NONE', *, *, #43892, .F. ) ;
#19522 = EDGE_CURVE ( 'NONE', #53541, #24982, #8208, .T. ) ;
#19523 = CARTESIAN_POINT ( 'NONE',  ( -130.5728709571500588, -24.54081503060122671, 9.556887179928187592 ) ) ;
#19524 = CARTESIAN_POINT ( 'NONE',  ( 22.44084908143146251, -0.7541981612834567361, -1.500000000000002220 ) ) ;
#19525 = VERTEX_POINT ( 'NONE', #23820 ) ;
#19526 = CARTESIAN_POINT ( 'NONE',  ( -100.0561916307745491, -25.05145249402578500, 7.523995081915606065 ) ) ;
#19527 = CARTESIAN_POINT ( 'NONE',  ( 23.22151214508649986, 3.827981938878625524E-15, -1.699999999999999956 ) ) ;
#19528 = EDGE_CURVE ( 'NONE', #5224, #26794, #17718, .T. ) ;
#19529 = CARTESIAN_POINT ( 'NONE',  ( 2.628295812946869425, -5.876774720514412742, 19.40849182188139110 ) ) ;
#19530 = CARTESIAN_POINT ( 'NONE',  ( -64.62287095715007013, -23.47596703998600631, 11.44779298504227683 ) ) ;
#19531 = EDGE_CURVE ( 'NONE', #70011, #96235, #8102, .T. ) ;
#19532 = CARTESIAN_POINT ( 'NONE',  ( -30.60160445864372747, -24.57215472537218304, 9.174899246800713115 ) ) ;
#19533 = CARTESIAN_POINT ( 'NONE',  ( 19.03533760385612439, 4.641190475545474037, -1.500000000000002220 ) ) ;
#19534 = EDGE_CURVE ( 'NONE', #37940, #55816, #82073, .T. ) ;
#19535 = CARTESIAN_POINT ( 'NONE',  ( -46.52204141198475185, -23.48783264082476663, -1.443836473390096575 ) ) ;
#19536 = ORIENTED_EDGE ( 'NONE', *, *, #5596, .T. ) ;
#19537 = CARTESIAN_POINT ( 'NONE',  ( -15.55086147716002110, 14.89234021980106881, -1.500000000000002220 ) ) ;
#19538 = CARTESIAN_POINT ( 'NONE',  ( -121.6228709571500417, -23.48783264082478794, -1.443836473390058384 ) ) ;
#19539 = EDGE_CURVE ( 'NONE', #41151, #87739, #22746, .T. ) ;
#19540 = FACE_OUTER_BOUND ( 'NONE', #68258, .T. ) ;
#19541 = LINE ( 'NONE', #81943, #29781 ) ;
#19542 = VECTOR ( 'NONE', #46958, 1000.000000000000114 ) ;
#19543 = CARTESIAN_POINT ( 'NONE',  ( 8.160000000000000142, 0.000000000000000000, 0.000000000000000000 ) ) ;
#19544 = CARTESIAN_POINT ( 'NONE',  ( 4.903590608199674072, 22.46510890469962263, -1.500000000000002220 ) ) ;
#19545 = APPROVAL_DATE_TIME ( #58133, #39556 ) ;
#19546 = LINE ( 'NONE', #50506, #45078 ) ;
#19547 = CARTESIAN_POINT ( 'NONE',  ( -0.02075734969026423599, -6.475225279485573360, -28.03397719988137382 ) ) ;
#19548 = CARTESIAN_POINT ( 'NONE',  ( 6.297820759360134524, 19.07352124001985771, 11.49999999999999645 ) ) ;
#19549 = FACE_OUTER_BOUND ( 'NONE', #41617, .T. ) ;
#19550 = CARTESIAN_POINT ( 'NONE',  ( 10.24059822343757808, -6.376774720514426953, 0.000000000000000000 ) ) ;
#19551 = CARTESIAN_POINT ( 'NONE',  ( -34.62287095715005592, -29.50247984919015209, -1.443849546365062242 ) ) ;
#19552 = CARTESIAN_POINT ( 'NONE',  ( 0.3244565263465140070, -1.558659884777350735, 2.575303280952439950E-15 ) ) ;
#19553 = EDGE_CURVE ( 'NONE', #18378, #4330, #65219, .T. ) ;
#19554 = CARTESIAN_POINT ( 'NONE',  ( 14.85834502026402681, 3.582999323269832725, -27.37203305628894867 ) ) ;
#19555 = CARTESIAN_POINT ( 'NONE',  ( 11.68167410197319001, -16.05257874518773065, 11.49999999999998934 ) ) ;
#19556 = CARTESIAN_POINT ( 'NONE',  ( -113.5892054360595722, -24.34968618360934300, 0.1864209137778879699 ) ) ;
#19557 = CARTESIAN_POINT ( 'NONE',  ( 19.69511366699831001, -0.05742560045514189665, -1.500000000000002220 ) ) ;
#19558 = CARTESIAN_POINT ( 'NONE',  ( 14.92699176545193573, -5.063793094955947538, -27.26229911407732942 ) ) ;
#19559 = VECTOR ( 'NONE', #15021, 1000.000000000000000 ) ;
#19560 = CONTEXT_DEPENDENT_SHAPE_REPRESENTATION ( #607, #35295 ) ;
#19562 = VECTOR ( 'NONE', #24087, 1000.000000000000000 ) ;
#19561 = DESIGN_CONTEXT ( 'detailed design', #68626, 'design' ) ;
#19563 = DIRECTION ( 'NONE',  ( -1.000000000000000000, -0.000000000000000000, -0.000000000000000000 ) ) ;
#19564 = CARTESIAN_POINT ( 'NONE',  ( 2.903846153846159517, -6.376774720514415407, 19.99999999999999289 ) ) ;
#19565 = CARTESIAN_POINT ( 'NONE',  ( -15.40095275084150117, -13.70674696055758801, 11.49999999999999645 ) ) ;
#19566 = CARTESIAN_POINT ( 'NONE',  ( -33.58953762381672448, -23.47596703998600276, 11.44779298504227505 ) ) ;
#19567 = B_SPLINE_CURVE_WITH_KNOTS ( 'NONE', 3,
 ( #37960, #61318, #53705, #15123, #77006, #38462 ),
 .UNSPECIFIED., .F., .F.,
 ( 4, 2, 4 ),
 ( 1.570755371634454886E-05, 0.001396183895866091439, 0.002776660238015838614 ),
 .UNSPECIFIED. ) ;
#19568 = CARTESIAN_POINT ( 'NONE',  ( 9.629844747126790949, -20.51516216672183290, 11.49999999999999645 ) ) ;
#19569 = EDGE_LOOP ( 'NONE', ( #75489, #89761, #93747 ) ) ;
#19570 = CARTESIAN_POINT ( 'NONE',  ( -69.38174606678134637, -25.12219007809040505, 6.471609302863886803 ) ) ;
#19571 = PLANE ( 'NONE',  #56530 ) ;
#19572 = ADVANCED_FACE ( 'NONE', ( #15711 ), #46675, .T. ) ;
#19573 = DIRECTION ( 'NONE',  ( -0.000000000000000000, 1.000000000000000000, -0.000000000000000000 ) ) ;
#19574 = DIRECTION ( 'NONE',  ( 0.000000000000000000, -2.173523156925979552E-06, 0.9999999999976378895 ) ) ;
#19575 = ORIENTED_EDGE ( 'NONE', *, *, #45542, .T. ) ;
#19576 = ORIENTED_EDGE ( 'NONE', *, *, #74142, .F. ) ;
#19577 = CARTESIAN_POINT ( 'NONE',  ( -99.29843613443789252, -25.24457243405052509, 6.219452043175907718 ) ) ;
#19578 = CARTESIAN_POINT ( 'NONE',  ( -4.526818761702180893, -22.41603498850323817, -1.500000000000002220 ) ) ;
#19579 = LINE ( 'NONE', #27208, #89182 ) ;
#19580 = CARTESIAN_POINT ( 'NONE',  ( 20.63042821663210091, 6.393326493806346100, -1.500000000000002220 ) ) ;
#19581 = CARTESIAN_POINT ( 'NONE',  ( -113.6244772655058739, -24.51419770103157347, 9.386484678747168076 ) ) ;
#19582 = CARTESIAN_POINT ( 'NONE',  ( -76.52287095715007581, -23.48786465467241769, 11.44779295918254469 ) ) ;
#19583 = CARTESIAN_POINT ( 'NONE',  ( -22.36795837939145670, 2.692536522722862813, 11.49999999999999645 ) ) ;
#19584 = ORIENTED_EDGE ( 'NONE', *, *, #81750, .F. ) ;
#19585 = CARTESIAN_POINT ( 'NONE',  ( -43.63416939196337552, -24.34968618360933590, 0.1864209137778851388 ) ) ;
#19586 = CARTESIAN_POINT ( 'NONE',  ( 18.29167757401336303, -12.14499471347784798, -1.500000000000002220 ) ) ;
#19587 = CARTESIAN_POINT ( 'NONE',  ( -44.56061661862030832, -23.73791477778911130, 11.05961554403171121 ) ) ;
#19588 = DIRECTION ( 'NONE',  ( 0.000000000000000000, 0.9999999999976377785, 2.173523156925979128E-06 ) ) ;
#19589 = ORIENTED_EDGE ( 'NONE', *, *, #22920, .T. ) ;
#19590 = DIRECTION ( 'NONE',  ( 0.000000000000000000, 2.173523156925980399E-06, -0.9999999999976378895 ) ) ;
#19591 = ADVANCED_FACE ( 'NONE', ( #2000 ), #24818, .T. ) ;
#19592 = CARTESIAN_POINT ( 'NONE',  ( 13.91401389203221406, 5.965225279485572685, 158.0376437107427137 ) ) ;
#19593 = ORIENTED_EDGE ( 'NONE', *, *, #52797, .T. ) ;
#19594 = DIRECTION ( 'NONE',  ( -0.5656310827093757876, 2.995395837334947896E-15, -0.8246584009594636333 ) ) ;
#19595 = ORIENTED_EDGE ( 'NONE', *, *, #86883, .T. ) ;
#19596 = VERTEX_POINT ( 'NONE', #32948 ) ;
#19597 = EDGE_LOOP ( 'NONE', ( #83847, #93460, #88627, #94093 ) ) ;
#19598 = CARTESIAN_POINT ( 'NONE',  ( -49.53224087187288660, -25.30395130311601193, 5.541308293284908260 ) ) ;
#19599 = CARTESIAN_POINT ( 'NONE',  ( -10.34999999999999254, 4.999999999999999112, 2.100000000000000089 ) ) ;
#19600 = CARTESIAN_POINT ( 'NONE',  ( -104.6235422597730036, -24.66019654487200441, 8.947790411086108620 ) ) ;
#19601 = CARTESIAN_POINT ( 'NONE',  ( -9.549598871097368047, 18.00506641634745009, -1.500000000000002220 ) ) ;
#19602 = EDGE_CURVE ( 'NONE', #96476, #58114, #39554, .T. ) ;
#19603 = EDGE_LOOP ( 'NONE', ( #89596, #67862, #76236, #3148, #7226, #58296 ) ) ;
#19604 = CARTESIAN_POINT ( 'NONE',  ( -71.66622694754684630, -25.20680239340841311, 6.551726662353233976 ) ) ;
#19605 = CARTESIAN_POINT ( 'NONE',  ( -50.70418202325330270, -25.12629190293465697, 2.864576727199638295 ) ) ;
#19606 = B_SPLINE_CURVE_WITH_KNOTS ( 'NONE', 3,
 ( #8889, #40342, #26114, #64711, #10386, #32722, #62693 ),
 .UNSPECIFIED., .F., .F.,
 ( 4, 1, 1, 1, 4 ),
 ( 0.000000000000000000, 0.2537340756906609762, 0.5030351201318566945, 0.7500135973308793558, 1.000000000000000000 ),
 .UNSPECIFIED. ) ;
#19607 = CARTESIAN_POINT ( 'NONE',  ( -105.5156730399040441, -24.15503026093913519, -0.2815557561904565298 ) ) ;
#19608 = CARTESIAN_POINT ( 'NONE',  ( -71.53177174497976409, -25.03149702581040614, 6.885843724247062703 ) ) ;
#19609 = ORIENTED_EDGE ( 'NONE', *, *, #4660, .F. ) ;
#19610 = CARTESIAN_POINT ( 'NONE',  ( -27.89567495842467082, -24.76880856562122801, 2.285879846231543500 ) ) ;
#19611 = CARTESIAN_POINT ( 'NONE',  ( -107.6228709571500701, -29.50248528299804818, 1.056150453629043584 ) ) ;
#19612 = B_SPLINE_CURVE_WITH_KNOTS ( 'NONE', 3,
 ( #67974, #6559, #23265, #13654 ),
 .UNSPECIFIED., .F., .F.,
 ( 4, 4 ),
 ( 0.000000000000000000, 9.999999999998897304E-05 ),
 .UNSPECIFIED. ) ;
#19613 = ORIENTED_EDGE ( 'NONE', *, *, #62876, .T. ) ;
#19614 = CARTESIAN_POINT ( 'NONE',  ( 8.872108392497455753, -18.76566404461018678, -1.500000000000002220 ) ) ;
#19615 = AXIS2_PLACEMENT_3D ( 'NONE', #65623, #49892, #95545 ) ;
#19616 = ORIENTED_EDGE ( 'NONE', *, *, #47821, .T. ) ;
#19617 = APPROVAL ( #88588, 'UNKNOWN' ) ;
#19619 = ORIENTED_EDGE ( 'NONE', *, *, #60438, .T. ) ;
#19618 = PLANE ( 'NONE',  #16672 ) ;
#19620 = CARTESIAN_POINT ( 'NONE',  ( -41.51335775656676930, -23.73791477778911485, 11.05961554403170766 ) ) ;
#19621 = CARTESIAN_POINT ( 'NONE',  ( -105.5228709571500616, -24.99156044556202971, 7.747789690856173195 ) ) ;
#19622 = VERTEX_POINT ( 'NONE', #16711 ) ;
#19623 = ORIENTED_EDGE ( 'NONE', *, *, #15326, .F. ) ;
#19624 = CARTESIAN_POINT ( 'NONE',  ( -114.6228709571500843, -24.34917612406838217, 0.1852690917426682848 ) ) ;
#19625 = CARTESIAN_POINT ( 'NONE',  ( 10.01577673925062584, 3.316774720514425567, -27.02510548822787584 ) ) ;
#19626 = LINE ( 'NONE', #12515, #69627 ) ;
#19627 = CARTESIAN_POINT ( 'NONE',  ( -43.64732276058348504, -23.96169478059712432, 10.65365249895718769 ) ) ;
#19629 = EDGE_LOOP ( 'NONE', ( #31384, #73804, #38041, #19494 ) ) ;
#19628 = CARTESIAN_POINT ( 'NONE',  ( 12.17348956504948987, -18.45705692928949659, 11.49999999999999645 ) ) ;
#19630 = CARTESIAN_POINT ( 'NONE',  ( -108.5164791698326070, -24.15543982623908192, -0.2315651400026445539 ) ) ;
#19631 = CARTESIAN_POINT ( 'NONE',  ( 19.70651319644445465, -11.07993823016455792, -1.500000000000002220 ) ) ;
#19633 = ORIENTED_EDGE ( 'NONE', *, *, #39155, .F. ) ;
#19632 = CARTESIAN_POINT ( 'NONE',  ( 5.265981236333619456E-16, 1.826774720514426464, -4.300000000000000711 ) ) ;
#19634 = AXIS2_PLACEMENT_3D ( 'NONE', #55122, #40393, #1835 ) ;
#19635 = ORIENTED_EDGE ( 'NONE', *, *, #26671, .F. ) ;
#19636 =( GEOMETRIC_REPRESENTATION_CONTEXT ( 3 ) GLOBAL_UNCERTAINTY_ASSIGNED_CONTEXT ( ( #37787 ) ) GLOBAL_UNIT_ASSIGNED_CONTEXT ( ( #19934, #20423, #28063 ) ) REPRESENTATION_CONTEXT ( 'NONE', 'WORKASPACE' ) );
#19637 = CARTESIAN_POINT ( 'NONE',  ( -69.52287095715006160, -23.47593901973090169, -1.443836447538996870 ) ) ;
#19638 = CARTESIAN_POINT ( 'NONE',  ( -128.5228709571500474, -23.48783264083417066, -1.443836473375472274 ) ) ;
#19639 = ORIENTED_EDGE ( 'NONE', *, *, #43489, .F. ) ;
#19640 = CARTESIAN_POINT ( 'NONE',  ( 13.39648796734645231, 16.42122281929413319, -1.500000000000002220 ) ) ;
#19641 = B_SPLINE_CURVE_WITH_KNOTS ( 'NONE', 3,
 ( #13425, #81463, #67742, #20537 ),
 .UNSPECIFIED., .F., .F.,
 ( 4, 4 ),
 ( 0.000000000000000000, 0.0004038461538461435296 ),
 .UNSPECIFIED. ) ;
#19642 = DIRECTION ( 'NONE',  ( 0.000000000000000000, -1.000000000000000000, 0.000000000000000000 ) ) ;
#19643 = CARTESIAN_POINT ( 'NONE',  ( -41.86995616089613748, -25.27977532709532227, 4.210709737483026238 ) ) ;
#19644 = CARTESIAN_POINT ( 'NONE',  ( 21.15698459081360383, -7.064864530413820454, -1.500000000000002220 ) ) ;
#19645 = CARTESIAN_POINT ( 'NONE',  ( -50.22356044790234364, -25.03220905709108735, 7.558303196641526611 ) ) ;
#19646 = VERTEX_POINT ( 'NONE', #47677 ) ;
#19647 = DIRECTION ( 'NONE',  ( 0.000000000000000000, -1.000000000000000000, -0.000000000000000000 ) ) ;
#19648 = CARTESIAN_POINT ( 'NONE',  ( -37.62372550051912157, -24.65952944569304606, 1.056160979905695907 ) ) ;
#19649 = CARTESIAN_POINT ( 'NONE',  ( -111.5228709571500616, -24.65952944569305316, 1.056160979905704123 ) ) ;
#19650 = CARTESIAN_POINT ( 'NONE',  ( 3.036358173076929123, -5.876774720514420736, 20.87990785256409865 ) ) ;
#19651 = CARTESIAN_POINT ( 'NONE',  ( -17.64752530894654470, 8.349842952099315596, 11.49999999999998934 ) ) ;
#19652 = EDGE_CURVE ( 'NONE', #41451, #56734, #49383, .T. ) ;
#19653 = CARTESIAN_POINT ( 'NONE',  ( 21.36505145794347982, 1.902718533054148509, -1.500000000000002220 ) ) ;
#19654 = CARTESIAN_POINT ( 'NONE',  ( -0.9257915630711897048, -5.876774720514408301, 19.25892998154168012 ) ) ;
#19655 = ADVANCED_FACE ( 'NONE', ( #78591 ), #65916, .F. ) ;
#19656 = PLANE ( 'NONE',  #16302 ) ;
#19657 = CARTESIAN_POINT ( 'NONE',  ( -58.52287095715004739, -23.47593901973090169, -1.443836447538997092 ) ) ;
#19658 = CARTESIAN_POINT ( 'NONE',  ( -0.9122204482399535186, 22.77315974801211240, -1.500000000000002220 ) ) ;
#19659 = DIRECTION ( 'NONE',  ( 0.8094161543772597778, 4.975585788371511936E-29, -0.5872354630240994577 ) ) ;
#19660 = FACE_OUTER_BOUND ( 'NONE', #13627, .T. ) ;
#19661 = DIRECTION ( 'NONE',  ( 0.000000000000000000, 1.000000000000000000, 0.000000000000000000 ) ) ;
#19662 = CARTESIAN_POINT ( 'NONE',  ( 19.92730240972663935, 0.8534881809820089593, 11.49999999999999645 ) ) ;
#19663 = CARTESIAN_POINT ( 'NONE',  ( -78.58953762381671027, -24.64898659630367916, 1.056161002820386274 ) ) ;
#19664 = CARTESIAN_POINT ( 'NONE',  ( -39.60861305632572282, -23.73791477778911485, 11.05961554403170943 ) ) ;
#19665 = CARTESIAN_POINT ( 'NONE',  ( 11.62916340711181284, 5.965225279485572685, 28.75961759920349792 ) ) ;
#19666 = ORIENTED_EDGE ( 'NONE', *, *, #34891, .F. ) ;
#19667 = EDGE_CURVE ( 'NONE', #75111, #28349, #37336, .T. ) ;
#19668 = CARTESIAN_POINT ( 'NONE',  ( 9.278253834636469577, -6.376774720514426953, 18.51871304725684553 ) ) ;
#19669 = CARTESIAN_POINT ( 'NONE',  ( 33.12653832968937451, 0.3587747205144265483, -7.315055336576590683 ) ) ;
#19670 = CARTESIAN_POINT ( 'NONE',  ( 15.89274262425319861, 14.76810421718133171, 11.49999999999998934 ) ) ;
#19671 = CARTESIAN_POINT ( 'NONE',  ( -4.752075056065355518, -6.376774720514406525, 19.17724329193115551 ) ) ;
#19672 = CARTESIAN_POINT ( 'NONE',  ( 17.64699390344983598, -8.409456921668478913, -1.500000000000002220 ) ) ;
#19673 = CARTESIAN_POINT ( 'NONE',  ( -55.57062048815932087, -23.48786465467241413, 11.44779295918254647 ) ) ;
#19674 = APPROVAL_ROLE ( '' ) ;
#19675 = FACE_OUTER_BOUND ( 'NONE', #64059, .T. ) ;
#19676 = CARTESIAN_POINT ( 'NONE',  ( 13.86372479123709311, 15.02075200336711092, 11.49999999999999645 ) ) ;
#19677 = CARTESIAN_POINT ( 'NONE',  ( -50.04514766445114304, -25.30330263116561440, 5.239125874704871677 ) ) ;
#19678 = AXIS2_PLACEMENT_3D ( 'NONE', #59632, #30156, #14924 ) ;
#19679 = CARTESIAN_POINT ( 'NONE',  ( 1.949999999999999956, -0.1925000000000001710, 0.1924999999999999212 ) ) ;
#19680 = ORIENTED_EDGE ( 'NONE', *, *, #92916, .F. ) ;
#19681 = PLANE ( 'NONE',  #32963 ) ;
#19682 = DIRECTION ( 'NONE',  ( -3.773278334453080206E-23, 0.9999999999976377785, 2.173523156925979975E-06 ) ) ;
#19683 = DIRECTION ( 'NONE',  ( -0.5630016722799275897, -4.164321980682959710E-15, 0.8264557562326038109 ) ) ;
#19684 = LINE ( 'NONE', #43545, #1421 ) ;
#19685 = VERTEX_POINT ( 'NONE', #26330 ) ;
#19686 = CARTESIAN_POINT ( 'NONE',  ( 5.642655980204820843, -6.376774720514418959, 20.71586687040766961 ) ) ;
#19687 = EDGE_CURVE ( 'NONE', #97228, #73442, #77194, .T. ) ;
#19688 = VECTOR ( 'NONE', #4966, 1000.000000000000114 ) ;
#19689 = CARTESIAN_POINT ( 'NONE',  ( 13.47786528765806580, -18.65256936556403744, 11.49999999999999645 ) ) ;
#19690 = CARTESIAN_POINT ( 'NONE',  ( -17.51746294255814718, -14.55262482891283504, -1.500000000000002220 ) ) ;
#19691 = CARTESIAN_POINT ( 'NONE',  ( -110.5228709571500616, -24.99132157543167310, 2.256160258750667502 ) ) ;
#19692 = CARTESIAN_POINT ( 'NONE',  ( -33.52287095715006160, -24.64898659630367206, 1.056161002820817485 ) ) ;
#19693 = CARTESIAN_POINT ( 'NONE',  ( -120.5228709571500900, -23.84081130425355965, 10.88220057483161263 ) ) ;
#19694 = CC_DESIGN_APPROVAL ( #66842, ( #95340 ) ) ;
#19695 = CARTESIAN_POINT ( 'NONE',  ( -27.13414387080440093, -0.3587747205144061202, -10.21530720150730609 ) ) ;
#19696 = CARTESIAN_POINT ( 'NONE',  ( -110.5222005161765679, -23.48783264082476308, -1.443836473390091468 ) ) ;
#19697 = CARTESIAN_POINT ( 'NONE',  ( 1.740910633133015972, 21.82039641801506846, 11.49999999999998934 ) ) ;
#19698 = EDGE_CURVE ( 'NONE', #95505, #79014, #5873, .T. ) ;
#19699 = CARTESIAN_POINT ( 'NONE',  ( -19.77875734969026311, -6.143225279485574397, 27.35402280011862430 ) ) ;
#19700 = DIRECTION ( 'NONE',  ( 0.000000000000000000, 0.000000000000000000, -1.000000000000000000 ) ) ;
#19701 = CARTESIAN_POINT ( 'NONE',  ( -28.62287095715004881, -29.50250473134420659, 10.00399446418115268 ) ) ;
#19702 = DIRECTION ( 'NONE',  ( -3.639962309748244178E-15, -1.000000000000000000, 2.135627652102599075E-15 ) ) ;
#19703 = ORIENTED_EDGE ( 'NONE', *, *, #59636, .T. ) ;
#19704 = CARTESIAN_POINT ( 'NONE',  ( -5.688044216684545518, -19.60349290560521140, -1.500000000000002220 ) ) ;
#19705 = EDGE_LOOP ( 'NONE', ( #8248, #20962, #70094, #70931, #31327, #79635, #9837, #77027, #15886, #20731, #42309 ) ) ;
#19706 = EDGE_LOOP ( 'NONE', ( #34948, #21789, #25513, #10580, #75410, #44750, #37957, #55344, #81008, #77486, #61949, #35473, #9203, #88512, #95234, #42085 ) ) ;
#19707 = ORIENTED_EDGE ( 'NONE', *, *, #9937, .F. ) ;
#19708 = VERTEX_POINT ( 'NONE', #79609 ) ;
#19709 = CARTESIAN_POINT ( 'NONE',  ( 20.35648204094723468, -10.72454223111430593, -1.500000000000002220 ) ) ;
#19710 = CARTESIAN_POINT ( 'NONE',  ( -80.52287095715003318, -24.15431212366389957, -0.2830839119429247042 ) ) ;
#19711 = CARTESIAN_POINT ( 'NONE',  ( 18.82035724208558491, -7.196742317222773799, -1.500000000000002220 ) ) ;
#19712 = VERTEX_POINT ( 'NONE', #80610 ) ;
#19713 = DIRECTION ( 'NONE',  ( 1.000000000000000000, 0.000000000000000000, 0.000000000000000000 ) ) ;
#19714 = DIRECTION ( 'NONE',  ( 0.000000000000000000, -1.000000000000000000, 0.000000000000000000 ) ) ;
#19715 = DIRECTION ( 'NONE',  ( 0.000000000000000000, -0.9999999999976377785, -2.173523156925979128E-06 ) ) ;
#19716 = CARTESIAN_POINT ( 'NONE',  ( 1.949999999999999956, -0.1925000000000001155, -0.1925000000000000600 ) ) ;
#19718 = ORIENTED_EDGE ( 'NONE', *, *, #33860, .T. ) ;
#19717 = CARTESIAN_POINT ( 'NONE',  ( -17.20161093224466953, -12.68000408521323408, 11.49999999999999645 ) ) ;
#19719 = DIRECTION ( 'NONE',  ( 0.000000000000000000, 0.9999999999976377785, 2.173523156925979975E-06 ) ) ;
#19720 = ORIENTED_EDGE ( 'NONE', *, *, #97720, .T. ) ;
#19721 = CARTESIAN_POINT ( 'NONE',  ( -19.27636426328722763, -11.15942449563467775, -1.500000000000002220 ) ) ;
#19722 = CARTESIAN_POINT ( 'NONE',  ( -20.51892249978613236, 2.527598752449112585, -1.500000000000002220 ) ) ;
#19723 = ADVANCED_FACE ( 'NONE', ( #12088 ), #33942, .T. ) ;
#19724 = ORIENTED_EDGE ( 'NONE', *, *, #55449, .T. ) ;
#19725 = CIRCLE ( 'NONE', #1935, 253.2618649670780826 ) ;
#19726 = DIRECTION ( 'NONE',  ( -3.773278334453079030E-23, 0.9999999999976377785, 2.173523156925979128E-06 ) ) ;
#19727 = ORIENTED_EDGE ( 'NONE', *, *, #48272, .T. ) ;
#19728 = DIRECTION ( 'NONE',  ( 4.251773225433346808E-15, 0.000000000000000000, -1.000000000000000000 ) ) ;
#19729 = ORIENTED_EDGE ( 'NONE', *, *, #3162, .F. ) ;
#19730 = CARTESIAN_POINT ( 'NONE',  ( 11.41483471809167405, 6.475225279485574248, -27.05170832580397189 ) ) ;
#19731 = CARTESIAN_POINT ( 'NONE',  ( 20.89173079421859214, 1.537965369061287557, -1.500000000000002220 ) ) ;
#19732 = CARTESIAN_POINT ( 'NONE',  ( 20.64021973274467570, 7.317367941133321452, 11.49999999999999645 ) ) ;
#19733 = FACE_OUTER_BOUND ( 'NONE', #33228, .T. ) ;
#19734 = CARTESIAN_POINT ( 'NONE',  ( -16.74547196562220464, 15.07928529822544661, -1.500000000000002220 ) ) ;
#19735 = EDGE_CURVE ( 'NONE', #65316, #10349, #13048, .T. ) ;
#19736 = CARTESIAN_POINT ( 'NONE',  ( 0.7041596644206948863, -20.94928778062849162, 11.49999999999998934 ) ) ;
#19737 = CARTESIAN_POINT ( 'NONE',  ( -110.5228709571500048, -24.51163499207180152, 0.6490370598555574855 ) ) ;
#19738 = CARTESIAN_POINT ( 'NONE',  ( 5.641575934020636396, -6.376774720514420736, 20.76276410292889096 ) ) ;
#19739 = CARTESIAN_POINT ( 'NONE',  ( -114.5228709571500616, -23.48783264083396105, -1.443836473375806895 ) ) ;
#19740 = CARTESIAN_POINT ( 'NONE',  ( -31.66446019296015280, -24.87219037988794312, 1.747789950295620232 ) ) ;
#19741 = ORIENTED_EDGE ( 'NONE', *, *, #32528, .F. ) ;
#19742 = VERTEX_POINT ( 'NONE', #11100 ) ;
#19743 = VERTEX_POINT ( 'NONE', #42069 ) ;
#19744 = VECTOR ( 'NONE', #76689, 1000.000000000000000 ) ;
#19745 = CARTESIAN_POINT ( 'NONE',  ( 10.46399479596396453, 2.682774720514426559, -27.03001098546561920 ) ) ;
#19746 = ORIENTED_EDGE ( 'NONE', *, *, #73543, .F. ) ;
#19747 = CARTESIAN_POINT ( 'NONE',  ( 1.049947104896167049, -21.43676768134831434, -1.500000000000002220 ) ) ;
#19748 = CARTESIAN_POINT ( 'NONE',  ( -0.02075734969026423599, 5.866774720514426278, 22.60902280011862686 ) ) ;
#19749 = ORIENTED_EDGE ( 'NONE', *, *, #92027, .T. ) ;
#19750 = CARTESIAN_POINT ( 'NONE',  ( 11.82777538550527119, 17.46297031709455183, 11.49999999999998934 ) ) ;
#19751 = CARTESIAN_POINT ( 'NONE',  ( -0.02075734969026423599, 5.965225279485572685, -0.08597719988137648983 ) ) ;
#19752 = CARTESIAN_POINT ( 'NONE',  ( -67.62287095715005592, -24.64898659630367916, 1.056161002820824368 ) ) ;
#19753 = CARTESIAN_POINT ( 'NONE',  ( -50.64239288538053074, -24.40133493613049964, 9.663955038902802386 ) ) ;
#19754 = CARTESIAN_POINT ( 'NONE',  ( -101.6235504250154236, -24.65952944569305316, 1.056160979905706121 ) ) ;
#19755 = CARTESIAN_POINT ( 'NONE',  ( -109.3611003627813147, -25.29407500041303791, 4.275929869372101955 ) ) ;
#19756 = CARTESIAN_POINT ( 'NONE',  ( -21.55788180805707555, 4.768121097544787190, -1.500000000000002220 ) ) ;
#19757 = ORIENTED_EDGE ( 'NONE', *, *, #54052, .T. ) ;
#19758 = ADVANCED_FACE ( 'NONE', ( #3997 ), #96337, .F. ) ;
#19759 = DIRECTION ( 'NONE',  ( 0.000000000000000000, 0.9999999999976377785, 2.173523156925979975E-06 ) ) ;
#19760 = EDGE_CURVE ( 'NONE', #62593, #88005, #72381, .T. ) ;
#19761 = CC_DESIGN_SECURITY_CLASSIFICATION ( #3711, ( #100432 ) ) ;
#19762 = CARTESIAN_POINT ( 'NONE',  ( -51.91911984596691809, -25.31633312187877394, 5.987871665635145391 ) ) ;
#19763 = CARTESIAN_POINT ( 'NONE',  ( -41.81544514806834201, -25.27955868049266996, 4.607988218795668445 ) ) ;
#19764 = CARTESIAN_POINT ( 'NONE',  ( -62.62750437465097519, -24.51419770103156281, 9.386484678747184063 ) ) ;
#19765 = AXIS2_PLACEMENT_3D ( 'NONE', #36171, #5709, #52892 ) ;
#19766 = LOCAL_TIME ( 0, 54, 15.00000000000000000, #85943 ) ;
#19767 = CARTESIAN_POINT ( 'NONE',  ( -96.62287095715007013, -23.73934037231757088, 11.05740245334328975 ) ) ;
#19768 = CARTESIAN_POINT ( 'NONE',  ( 16.11712757473013014, 13.99349609535929773, 11.49999999999998934 ) ) ;
#19769 = DIRECTION ( 'NONE',  ( -0.1254312216594016538, 0.000000000000000000, -0.9921023176230513441 ) ) ;
#19770 = CARTESIAN_POINT ( 'NONE',  ( -11.64875734969026233, -0.3587747205144265483, 31.02402280011862246 ) ) ;
#19771 = EDGE_CURVE ( 'NONE', #99974, #81663, #72515, .T. ) ;
#19772 = FACE_OUTER_BOUND ( 'NONE', #114, .T. ) ;
#19773 = CARTESIAN_POINT ( 'NONE',  ( -81.23220280989026776, -25.17055267398807317, 6.810866775833154030 ) ) ;
#19774 = CARTESIAN_POINT ( 'NONE',  ( -9.675873947287982446, 20.46574270456686406, -1.500000000000002220 ) ) ;
#19775 = ADVANCED_FACE ( 'NONE', ( #81110 ), #2924, .T. ) ;
#19776 = DIRECTION ( 'NONE',  ( 1.000000000000000000, 0.000000000000000000, 0.000000000000000000 ) ) ;
#19777 = VERTEX_POINT ( 'NONE', #36929 ) ;
#19778 = CARTESIAN_POINT ( 'NONE',  ( 4.453188626415028217, -5.876774720514422512, 21.07953283331298167 ) ) ;
#19779 = CARTESIAN_POINT ( 'NONE',  ( -99.52287095715009002, -23.47593901973090524, -1.443836447538996648 ) ) ;
#19780 = CARTESIAN_POINT ( 'NONE',  ( -17.81549539028256746, -8.563599010019245839, 11.49999999999999645 ) ) ;
#19781 = CARTESIAN_POINT ( 'NONE',  ( -82.62287095715005592, -23.95044443724992789, 10.65354141964649592 ) ) ;
#19782 = CARTESIAN_POINT ( 'NONE',  ( -32.07722060962683486, -25.27409513349664749, 3.734526454214742497 ) ) ;
#19783 = EDGE_LOOP ( 'NONE', ( #25832, #26085, #3305, #25963 ) ) ;
#19784 = ADVANCED_FACE ( 'NONE', ( #20198 ), #84099, .T. ) ;
#19785 = LINE ( 'NONE', #58869, #74952 ) ;
#19786 = CARTESIAN_POINT ( 'NONE',  ( -70.52287095715007581, -24.83620972994590659, 8.398175272781360334 ) ) ;
#19787 = CARTESIAN_POINT ( 'NONE',  ( -102.6228709571500559, -24.64898659630368272, 1.056161002820829697 ) ) ;
#19788 = CARTESIAN_POINT ( 'NONE',  ( -15.70146493180990888, -14.86199287721409590, -1.500000000000002220 ) ) ;
#19789 = LINE ( 'NONE', #56390, #90697 ) ;
#19790 = CARTESIAN_POINT ( 'NONE',  ( -18.23339674026497903, -6.527145932826366348, -1.500000000000002220 ) ) ;
#19791 = EDGE_CURVE ( 'NONE', #46870, #45965, #26362, .T. ) ;
#19792 = B_SPLINE_CURVE_WITH_KNOTS ( 'NONE', 3,
 ( #57706, #89146, #3922, #81538, #25235, #96259 ),
 .UNSPECIFIED., .F., .F.,
 ( 4, 2, 4 ),
 ( 1.570755371634013412E-05, 0.001396183895866087536, 0.002776660238015834711 ),
 .UNSPECIFIED. ) ;
#19793 = FACE_OUTER_BOUND ( 'NONE', #18006, .T. ) ;
#19794 = DIRECTION ( 'NONE',  ( 0.000000000000000000, -1.000000000000000000, 0.000000000000000000 ) ) ;
#19795 = CARTESIAN_POINT ( 'NONE',  ( -18.77405512783484198, 6.205181830411797606, -1.500000000000002220 ) ) ;
#19796 = ORIENTED_EDGE ( 'NONE', *, *, #61018, .T. ) ;
#19797 = CARTESIAN_POINT ( 'NONE',  ( 2.300710779914242110, 20.15441874099239783, 11.49999999999999645 ) ) ;
#19798 = CARTESIAN_POINT ( 'NONE',  ( -119.5228709571500474, -23.73934037231757799, 11.05740245334328087 ) ) ;
#19800 = CIRCLE ( 'NONE', #70002, 18.50000000000000000 ) ;
#19799 = CARTESIAN_POINT ( 'NONE',  ( -51.62287095715005592, -29.50248528299804818, 1.056150453629033370 ) ) ;
#19801 = ORIENTED_EDGE ( 'NONE', *, *, #45987, .F. ) ;
#19802 = CARTESIAN_POINT ( 'NONE',  ( 8.500000000000000000, 0.000000000000000000, -3.750000000000000000 ) ) ;
#19803 = LINE ( 'NONE', #4102, #83309 ) ;
#19804 = CARTESIAN_POINT ( 'NONE',  ( 27.53860345374771867, -1.477225279485574028, -9.482392034746240483 ) ) ;
#19805 = CARTESIAN_POINT ( 'NONE',  ( -92.58953762381672448, -24.66019654487199730, 8.947790411086121054 ) ) ;
#19806 = CARTESIAN_POINT ( 'NONE',  ( -86.92287095715003886, -23.47596703998600276, 11.44779298504227683 ) ) ;
#19807 = CARTESIAN_POINT ( 'NONE',  ( 11.39338536883839659, -16.50304575528446804, 11.49999999999998934 ) ) ;
#19808 = CARTESIAN_POINT ( 'NONE',  ( -126.5228709571500616, -24.64965694238408034, 8.947790433994189385 ) ) ;
#19809 = ORIENTED_EDGE ( 'NONE', *, *, #79470, .T. ) ;
#19810 = CARTESIAN_POINT ( 'NONE',  ( -58.55620429048338593, -24.66019654487199020, 8.947790411086135265 ) ) ;
#19811 = AXIS2_PLACEMENT_3D ( 'NONE', #3850, #34790, #65761 ) ;
#19812 = CARTESIAN_POINT ( 'NONE',  ( 10.54059822343757880, -6.376774720514426953, 22.82308057603841078 ) ) ;
#19813 = CARTESIAN_POINT ( 'NONE',  ( 24.50000000000000000, 0.000000000000000000, -1.103411337323757957 ) ) ;
#19814 = VECTOR ( 'NONE', #97071, 1000.000000000000000 ) ;
#19815 = LINE ( 'NONE', #81731, #98295 ) ;
#19816 = DIRECTION ( 'NONE',  ( 0.000000000000000000, 3.055962005780221396E-15, -1.000000000000000000 ) ) ;
#19817 = EDGE_CURVE ( 'NONE', #59400, #27745, #96625, .T. ) ;
#19818 = DIRECTION ( 'NONE',  ( -0.000000000000000000, 2.173523156925979552E-06, -0.9999999999976378895 ) ) ;
#19819 = ORIENTED_EDGE ( 'NONE', *, *, #70735, .F. ) ;
#19820 = CARTESIAN_POINT ( 'NONE',  ( -12.25758032491116367, 16.21837406056298292, 11.49999999999998934 ) ) ;
#19821 = ORIENTED_EDGE ( 'NONE', *, *, #83621, .F. ) ;
#19822 = CARTESIAN_POINT ( 'NONE',  ( 2.319610639010541764, -22.79860127089448696, 11.49999999999998934 ) ) ;
#19823 = CARTESIAN_POINT ( 'NONE',  ( 31.62401270459618630, 4.290926300276496796, 26.86768354919275836 ) ) ;
#19824 = ORIENTED_EDGE ( 'NONE', *, *, #36573, .F. ) ;
#19825 = CARTESIAN_POINT ( 'NONE',  ( -49.34131120686307526, -25.30051202764760632, 4.642102575841966505 ) ) ;
#19826 = CARTESIAN_POINT ( 'NONE',  ( -49.66108014839032592, -25.26264131307726757, 6.884432116491313813 ) ) ;
#19827 = VECTOR ( 'NONE', #60983, 1000.000000000000114 ) ;
#19828 = CARTESIAN_POINT ( 'NONE',  ( -72.58953762381672448, -23.47593901973091235, -1.443836447539006196 ) ) ;
#19829 = CARTESIAN_POINT ( 'NONE',  ( 20.83148622972472808, -3.941400823363257366, 11.49999999999999645 ) ) ;
#19830 = SECURITY_CLASSIFICATION ( '', '', #26308 ) ;
#19831 = CARTESIAN_POINT ( 'NONE',  ( -15.97456084408017674, 15.39233244482803009, 11.49999999999998934 ) ) ;
#19832 = CARTESIAN_POINT ( 'NONE',  ( 20.45670835789597319, 2.398913822417158226, -1.500000000000002220 ) ) ;
#19833 = ADVANCED_FACE ( 'NONE', ( #52161 ), #87972, .T. ) ;
#19834 = ORIENTED_EDGE ( 'NONE', *, *, #63480, .T. ) ;
#19835 = CARTESIAN_POINT ( 'NONE',  ( -41.65560179646217165, -23.73766607897670866, -1.055555164236441801 ) ) ;
#19836 = ORIENTED_EDGE ( 'NONE', *, *, #72506, .T. ) ;
#19837 = LINE ( 'NONE', #5625, #62486 ) ;
#19838 = CARTESIAN_POINT ( 'NONE',  ( -126.6228709571500843, -24.66019654487200441, 8.947790411086119278 ) ) ;
#19839 = ORIENTED_EDGE ( 'NONE', *, *, #95018, .T. ) ;
#19840 = VERTEX_POINT ( 'NONE', #83091 ) ;
#19841 = EDGE_CURVE ( 'NONE', #89121, #72949, #13581, .T. ) ;
#19842 = ORIENTED_EDGE ( 'NONE', *, *, #71223, .F. ) ;
#19843 = VECTOR ( 'NONE', #33106, 1000.000000000000114 ) ;
#19844 = CARTESIAN_POINT ( 'NONE',  ( -71.20541289166536103, -29.50249360700573931, 4.885880847770192048 ) ) ;
#19845 = DIRECTION ( 'NONE',  ( 0.000000000000000000, -0.9999999999976377785, -2.173523156925979128E-06 ) ) ;
#19846 = CARTESIAN_POINT ( 'NONE',  ( -94.55620429048336462, -24.64965694238574656, 8.947790433994196491 ) ) ;
#19847 = CARTESIAN_POINT ( 'NONE',  ( 10.87737074370964407, 17.65887017642603851, -1.500000000000002220 ) ) ;
#19848 = CARTESIAN_POINT ( 'NONE',  ( 18.95625057990686813, 10.65820999021175730, 11.49999999999999645 ) ) ;
#19849 = ORIENTED_EDGE ( 'NONE', *, *, #84965, .T. ) ;
#19850 = EDGE_CURVE ( 'NONE', #14468, #36980, #20411, .T. ) ;
#19851 = DIRECTION ( 'NONE',  ( 1.000000000000000000, 0.000000000000000000, 0.000000000000000000 ) ) ;
#19852 = CARTESIAN_POINT ( 'NONE',  ( -119.6228709571501128, -24.35013146730203815, 9.818937971375104823 ) ) ;
#19853 = CARTESIAN_POINT ( 'NONE',  ( 20.43785579724129420, 9.289222182981756504, -1.500000000000002220 ) ) ;
#19854 = ADVANCED_FACE ( 'NONE', ( #7470 ), #62283, .T. ) ;
#19855 = ADVANCED_FACE ( 'NONE', ( #8978 ), #38430, .F. ) ;
#19856 = LINE ( 'NONE', #35607, #69150 ) ;
#19857 = DIRECTION ( 'NONE',  ( 0.3133898629642195011, 5.365801633547218220E-16, -0.9496245541219264785 ) ) ;
#19858 = ORIENTED_EDGE ( 'NONE', *, *, #45998, .F. ) ;
#19859 = CARTESIAN_POINT ( 'NONE',  ( -75.52287095715006160, -24.14321612903116332, -0.2833117244521500266 ) ) ;
#19860 = FACE_OUTER_BOUND ( 'NONE', #45985, .T. ) ;
#19861 = B_SPLINE_SURFACE_WITH_KNOTS ( 'NONE', 3, 1, ( 
 ( #14032, #91661 ),
 ( #21639, #99756 ),
 ( #30261, #61240 ),
 ( #52119, #14536 ),
 ( #21149, #43997 ),
 ( #53125, #69330 ),
 ( #67350, #61739 ),
 ( #22141, #28775 ),
 ( #6437, #83043 ),
 ( #45512, #92656 ),
 ( #82555, #68341 ),
 ( #37393, #60737 ),
 ( #13038, #74930 ),
 ( #5435, #59738 ),
 ( #13533, #75430 ),
 ( #5931, #36884 ),
 ( #67851, #39382 ),
 ( #32266, #819 ),
 ( #94160, #47504 ) ),
 .UNSPECIFIED., .F., .F., .F.,
 ( 4, 1, 1, 1, 1, 1, 1, 1, 1, 1, 1, 1, 1, 1, 1, 1, 4 ),
 ( 2, 2 ),
 ( 0.000000000000000000, 0.07735147826526167503, 0.1497817737883350153, 0.2198699552839552540, 0.2879755066202374092, 0.3546781060271980701, 0.4187834319376945169, 0.4827347082469889417, 0.5473072519464179386, 0.5826981022599692084, 0.6240955651677930760, 0.6712929496345362290, 0.7243202075485730695, 0.7838489433400213091, 0.8494366971205804528, 0.9216570148063001344, 1.000000000000000000 ),
 ( 0.000000000000000000, 1.000000000000000000 ),
 .UNSPECIFIED. ) ;
#19862 = EDGE_CURVE ( 'NONE', #13321, #39067, #56765, .T. ) ;
#19863 = ORIENTED_EDGE ( 'NONE', *, *, #100264, .T. ) ;
#19864 = ORIENTED_EDGE ( 'NONE', *, *, #75366, .T. ) ;
#19865 = CARTESIAN_POINT ( 'NONE',  ( -46.48369806289436923, -24.66019654487199375, 8.947790411086122830 ) ) ;
#19866 = VERTEX_POINT ( 'NONE', #46056 ) ;
#19867 = VECTOR ( 'NONE', #36626, 1000.000000000000114 ) ;
#19868 = CARTESIAN_POINT ( 'NONE',  ( 12.11089201280794470, -17.53110042540249225, -1.500000000000002220 ) ) ;
#19869 = ORIENTED_EDGE ( 'NONE', *, *, #1374, .T. ) ;
#19870 = CARTESIAN_POINT ( 'NONE',  ( -88.59161115057158042, -24.15543982623907837, -0.2315651400026634832 ) ) ;
#19871 = CARTESIAN_POINT ( 'NONE',  ( 21.07893183998518438, -5.767110019903106455, -1.500000000000002220 ) ) ;
#19872 = CARTESIAN_POINT ( 'NONE',  ( 29.73860345376319358, 4.772774720514425972, -8.849814207987163783 ) ) ;
#19873 = CARTESIAN_POINT ( 'NONE',  ( 20.21490908150494192, 10.32750977814155391, -1.500000000000002220 ) ) ;
#19874 = CARTESIAN_POINT ( 'NONE',  ( -41.42599659256448774, -25.28892559315755761, 3.925284093188281087 ) ) ;
#19875 = CARTESIAN_POINT ( 'NONE',  ( -35.62287095715004881, -24.62226745350438506, 0.9660975649728152925 ) ) ;
#19876 = CARTESIAN_POINT ( 'NONE',  ( 11.39931579351042679, 18.75040340349860557, -1.500000000000002220 ) ) ;
#19877 = CARTESIAN_POINT ( 'NONE',  ( 6.826756808399247589, -6.376774720514424288, 21.36722843294932161 ) ) ;
#19878 = ORIENTED_EDGE ( 'NONE', *, *, #16253, .F. ) ;
#19879 = FACE_OUTER_BOUND ( 'NONE', #35725, .T. ) ;
#19881 = EDGE_CURVE ( 'NONE', #67682, #13448, #53670, .T. ) ;
#19880 = FACE_OUTER_BOUND ( 'NONE', #19018, .T. ) ;
#19882 = EDGE_CURVE ( 'NONE', #87855, #44756, #93208, .T. ) ;
#19883 = ORIENTED_EDGE ( 'NONE', *, *, #78299, .F. ) ;
#19884 = DIRECTION ( 'NONE',  ( 0.000000000000000000, -1.000000000000000000, 0.000000000000000000 ) ) ;
#19885 = ORIENTED_EDGE ( 'NONE', *, *, #75762, .F. ) ;
#19886 = VECTOR ( 'NONE', #13426, 1000.000000000000114 ) ;
#19887 = CARTESIAN_POINT ( 'NONE',  ( -40.48848937406284421, -25.17730189479833669, 6.892737719230496829 ) ) ;
#19888 = CARTESIAN_POINT ( 'NONE',  ( -10.24013151130244736, -23.09176648418334921, 1.095224832288505201 ) ) ;
#19889 = CARTESIAN_POINT ( 'NONE',  ( -21.25539211000977957, 0.9166567589900279645, -1.500000000000002220 ) ) ;
#19890 = CARTESIAN_POINT ( 'NONE',  ( -112.5139921198612711, -24.65952944569305316, 1.056160979905707675 ) ) ;
#19891 = CARTESIAN_POINT ( 'NONE',  ( -26.14706027629300422, -24.75186366296204454, 4.097425152336787058 ) ) ;
#19892 = EDGE_CURVE ( 'NONE', #90405, #49749, #40921, .T. ) ;
#19893 = CARTESIAN_POINT ( 'NONE',  ( -85.58094847593091004, -25.00158670708910691, 2.256160236439219258 ) ) ;
#19894 = CARTESIAN_POINT ( 'NONE',  ( -68.50597231294825917, -24.15543982623907127, -0.2315651400026649820 ) ) ;
#19895 = ADVANCED_FACE ( 'NONE', ( #23693 ), #15089, .F. ) ;
#19896 = CARTESIAN_POINT ( 'NONE',  ( -39.62287095715005592, -23.48786465467240347, 11.44779295918255180 ) ) ;
#19897 = ORIENTED_EDGE ( 'NONE', *, *, #69369, .F. ) ;
#19898 = CARTESIAN_POINT ( 'NONE',  ( -13.18904525526904692, 14.46673508071025971, 11.49999999999999645 ) ) ;
#19899 = CARTESIAN_POINT ( 'NONE',  ( -99.12380231474227799, -25.27434709648489886, 4.001575133896465353 ) ) ;
#19900 = PLANE ( 'NONE',  #15602 ) ;
#19901 = ORIENTED_EDGE ( 'NONE', *, *, #87757, .T. ) ;
#19902 = EDGE_CURVE ( 'NONE', #93720, #14489, #70030, .T. ) ;
#19903 = CARTESIAN_POINT ( 'NONE',  ( 4.038745349937860496, -5.876774720514428729, 21.81354843764681206 ) ) ;
#19904 = CARTESIAN_POINT ( 'NONE',  ( -99.16166289166532977, -25.31166538673566180, 5.311370725864150266 ) ) ;
#19906 = EDGE_CURVE ( 'NONE', #3020, #36632, #85598, .T. ) ;
#19905 = DIRECTION ( 'NONE',  ( 0.000000000000000000, -0.9999999999976377785, -2.173523156925979128E-06 ) ) ;
#19907 = VECTOR ( 'NONE', #81334, 1000.000000000000114 ) ;
#19908 = CARTESIAN_POINT ( 'NONE',  ( -40.62287095715004170, -24.14406661707770141, 10.28769366152061160 ) ) ;
#19909 = CARTESIAN_POINT ( 'NONE',  ( 17.62393913918218402, -8.800128315780904487, -1.500000000000002220 ) ) ;
#19910 = ADVANCED_FACE ( 'NONE', ( #47557 ), #9331, .T. ) ;
#19912 = ORIENTED_EDGE ( 'NONE', *, *, #72035, .F. ) ;
#19911 = SECURITY_CLASSIFICATION ( '', '', #62255 ) ;
#19913 = CARTESIAN_POINT ( 'NONE',  ( -9.749999999999984013, 18.74999999999999645, 2.100000000000000089 ) ) ;
#19914 = CARTESIAN_POINT ( 'NONE',  ( -114.6228709571500559, -29.50250243563736774, 8.947779886222136270 ) ) ;
#19915 = B_SPLINE_CURVE_WITH_KNOTS ( 'NONE', 3,
 ( #2277, #3773, #63685, #10876 ),
 .UNSPECIFIED., .F., .F.,
 ( 4, 4 ),
 ( 1.798233777275264259E-11, 0.002370364882941363924 ),
 .UNSPECIFIED. ) ;
#19916 = AXIS2_PLACEMENT_3D ( 'NONE', #46375, #78311, #39754 ) ;
#19918 = EDGE_CURVE ( 'NONE', #10895, #15452, #51892, .T. ) ;
#19917 = CALENDAR_DATE ( 2026, 9, 10 ) ;
#19919 = EDGE_LOOP ( 'NONE', ( #44964, #50286, #97124, #89606 ) ) ;
#19920 = CARTESIAN_POINT ( 'NONE',  ( -28.49194798280535323, 5.965225279485572685, 28.38521343323375490 ) ) ;
#19921 = CARTESIAN_POINT ( 'NONE',  ( -105.6228709571501128, -24.82576562982392687, 8.398263435472967942 ) ) ;
#19922 = CARTESIAN_POINT ( 'NONE',  ( -47.54695344001475377, -24.15543982623907127, -0.2315651400026536022 ) ) ;
#19923 = CARTESIAN_POINT ( 'NONE',  ( -84.52287095715006160, -23.47596703998600631, 11.44779298504228571 ) ) ;
#19924 = CYLINDRICAL_SURFACE ( 'NONE', #66347, 11.85241003308275864 ) ;
#19925 = FACE_OUTER_BOUND ( 'NONE', #8685, .T. ) ;
#19926 = VECTOR ( 'NONE', #27140, 1000.000000000000114 ) ;
#19927 = CARTESIAN_POINT ( 'NONE',  ( -117.5228709571500758, -29.50250243563736774, 8.947779886222134493 ) ) ;
#19928 = CARTESIAN_POINT ( 'NONE',  ( 17.47191945374660094, 9.613082372698542599, 11.49999999999998934 ) ) ;
#19929 = CARTESIAN_POINT ( 'NONE',  ( 7.166666666666668739, -6.376774720514420736, 20.78665865384614975 ) ) ;
#19930 = CARTESIAN_POINT ( 'NONE',  ( -0.05005869551267223827, -22.40195084843249518, 1.075460532450188023 ) ) ;
#19931 = ORIENTED_EDGE ( 'NONE', *, *, #55536, .F. ) ;
#19932 = CARTESIAN_POINT ( 'NONE',  ( 19.92151214508649915, 3.625915217019311583E-15, -1.699999999999999956 ) ) ;
#19933 = CARTESIAN_POINT ( 'NONE',  ( 3.787259615384621192, -6.376774720514426065, 21.48076923076922640 ) ) ;
#19934 =( LENGTH_UNIT ( ) NAMED_UNIT ( * ) SI_UNIT ( .MILLI., .METRE. ) );
#19935 = CARTESIAN_POINT ( 'NONE',  ( 8.655157120174900243, -3.316774720514428232, -28.10018424651253000 ) ) ;
#19936 = CARTESIAN_POINT ( 'NONE',  ( -125.6228709571500559, -29.50250786944525672, 11.44777988621622633 ) ) ;
#19937 = CARTESIAN_POINT ( 'NONE',  ( 2.230654205607476737, -0.1647943925233645579, -7.922169807384186089E-16 ) ) ;
#19938 = CARTESIAN_POINT ( 'NONE',  ( -26.11702346598058710, -24.95514697357233302, 4.364016039383404433 ) ) ;
#19939 = CARTESIAN_POINT ( 'NONE',  ( 2.750000000000001332, 27.59999999999999432, 2.100000000000000089 ) ) ;
#19940 = ORIENTED_EDGE ( 'NONE', *, *, #47500, .T. ) ;
#19941 = B_SPLINE_SURFACE_WITH_KNOTS ( 'NONE', 3, 1, ( 
 ( #83891, #37229 ),
 ( #7768, #14873 ),
 ( #9652, #40609 ),
 ( #91500, #29107 ),
 ( #86770, #14373 ),
 ( #21979, #30102 ),
 ( #30604, #68181 ),
 ( #94383, #60083 ),
 ( #29604, #76271 ),
 ( #52960, #6765 ),
 ( #100090, #92003 ),
 ( #22473, #45841 ),
 ( #32489, #63462 ),
 ( #7260, #38214 ),
 ( #69170, #10656 ),
 ( #2056, #89277 ),
 ( #50222, #17768 ),
 ( #95388, #96386 ),
 ( #41113, #34494 ) ),
 .UNSPECIFIED., .F., .F., .F.,
 ( 4, 1, 1, 1, 1, 1, 1, 1, 1, 1, 1, 1, 1, 1, 1, 1, 4 ),
 ( 2, 2 ),
 ( 0.000000000000000000, 0.07607173695556672388, 0.1487517145745168301, 0.2184027938458466545, 0.2857595810623843602, 0.3505980236748781342, 0.4149640445981273573, 0.4780693385717832977, 0.5417606760069103577, 0.6043498585387204747, 0.6640750210708951107, 0.7214636230802008443, 0.7775871282364469339, 0.8326444469271317983, 0.8878435110684590459, 0.9434603426519472258, 1.000000000000000000 ),
 ( 0.000000000000000000, 1.000000000000000000 ),
 .UNSPECIFIED. ) ;
#19942 = FACE_OUTER_BOUND ( 'NONE', #73063, .T. ) ;
#19943 = CYLINDRICAL_SURFACE ( 'NONE', #17766, 2.899999999999999467 ) ;
#19944 = ORIENTED_EDGE ( 'NONE', *, *, #93302, .T. ) ;
#19945 = CARTESIAN_POINT ( 'NONE',  ( 8.375906630400100639, -18.44307005126401933, -1.500000000000002220 ) ) ;
#19946 = B_SPLINE_CURVE_WITH_KNOTS ( 'NONE', 3,
 ( #26192, #3377, #50530, #65781 ),
 .UNSPECIFIED., .F., .F.,
 ( 4, 4 ),
 ( 0.000000000000000000, 1.000000000000000000 ),
 .UNSPECIFIED. ) ;
#19947 = DIRECTION ( 'NONE',  ( -3.773278334453079618E-23, 0.9999999999976377785, 2.173523156925979975E-06 ) ) ;
#19948 = DIRECTION ( 'NONE',  ( 0.000000000000000000, -0.9999999999976377785, -2.173523156925979975E-06 ) ) ;
#19949 = CIRCLE ( 'NONE', #23208, 1.250000000000001998 ) ;
#19950 = CARTESIAN_POINT ( 'NONE',  ( 13.10664265030973930, -0.3587747205144256601, -28.64597719988137570 ) ) ;
#19951 = EDGE_LOOP ( 'NONE', ( #96367, #9175, #19375, #11388 ) ) ;
#19952 = CARTESIAN_POINT ( 'NONE',  ( -80.09162780144649219, -25.31560333233622373, 5.003082748975755223 ) ) ;
#19953 = LINE ( 'NONE', #89974, #71368 ) ;
#19954 = CARTESIAN_POINT ( 'NONE',  ( 2.879247915899910470, -19.84986158617241614, -1.500000000000002220 ) ) ;
#19955 = AXIS2_PLACEMENT_3D ( 'NONE', #63265, #9457, #54643 ) ;
#19956 = CARTESIAN_POINT ( 'NONE',  ( 14.98681507544721292, -14.71779577663021321, 11.49999999999999645 ) ) ;
#19957 = DIRECTION ( 'NONE',  ( -1.000000000000000000, 7.960204194457801640E-17, 0.000000000000000000 ) ) ;
#19958 = CARTESIAN_POINT ( 'NONE',  ( 10.86264265030973952, -5.965225279485574461, -27.62597719988137612 ) ) ;
#19959 = CARTESIAN_POINT ( 'NONE',  ( 18.88560736741940005, 11.47387103136259690, 11.49999999999998934 ) ) ;
#19960 = B_SPLINE_CURVE_WITH_KNOTS ( 'NONE', 3,
 ( #50907, #32807, #59024, #12821 ),
 .UNSPECIFIED., .F., .F.,
 ( 4, 4 ),
 ( 0.4401001892501570922, 0.4491066205222725150 ),
 .UNSPECIFIED. ) ;
#19961 = CARTESIAN_POINT ( 'NONE',  ( -39.46140038746126777, -25.27805951068589962, 4.366343927290111893 ) ) ;
#19962 = EDGE_CURVE ( 'NONE', #18378, #79772, #11979, .T. ) ;
#19963 = CARTESIAN_POINT ( 'NONE',  ( -91.62287095715004170, -24.64965695001468404, 8.947790433994180503 ) ) ;
#19964 = DIRECTION ( 'NONE',  ( -1.000000000000000000, -3.773278334444166432E-23, -8.201307841325785021E-29 ) ) ;
#19965 = ORIENTED_EDGE ( 'NONE', *, *, #70456, .T. ) ;
#19966 = CARTESIAN_POINT ( 'NONE',  ( -72.63060126349051870, -24.34968618360933590, 0.1864209137778795600 ) ) ;
#19967 = DIRECTION ( 'NONE',  ( 0.000000000000000000, -1.000000000000000000, 0.000000000000000000 ) ) ;
#19968 = EDGE_CURVE ( 'NONE', #95644, #82884, #88116, .T. ) ;
#19969 = VERTEX_POINT ( 'NONE', #49560 ) ;
#19970 = ADVANCED_FACE ( 'NONE', ( #50545 ), #18095, .T. ) ;
#19971 = EDGE_LOOP ( 'NONE', ( #43586, #26968, #80985, #81512 ) ) ;
#19972 = CARTESIAN_POINT ( 'NONE',  ( -49.52287095715006160, -24.64898659630367561, 1.056161002820821038 ) ) ;
#19973 = LINE ( 'NONE', #82374, #66519 ) ;
#19974 = CARTESIAN_POINT ( 'NONE',  ( -76.51216158835003966, -23.96119346886880663, -0.6495511937832058047 ) ) ;
#19975 = CARTESIAN_POINT ( 'NONE',  ( -12.99546161633903552, -15.93940442571882876, -1.500000000000002220 ) ) ;
#19976 = EDGE_CURVE ( 'NONE', #32255, #33057, #40010, .T. ) ;
#19977 = CARTESIAN_POINT ( 'NONE',  ( -21.01953065494444317, -4.859126342152997324, 11.49999999999999645 ) ) ;
#19978 = VERTEX_POINT ( 'NONE', #80489 ) ;
#19979 = CARTESIAN_POINT ( 'NONE',  ( -49.27764846858840997, -25.26180677598144086, 6.145204968850301874 ) ) ;
#19980 = CARTESIAN_POINT ( 'NONE',  ( -56.52287095715008292, -24.66019654487199375, 8.947790411086122830 ) ) ;
#19981 = CARTESIAN_POINT ( 'NONE',  ( -8.160000000000000142, -6.754662360505033547, 7.925641719537454222 ) ) ;
#19982 = CARTESIAN_POINT ( 'NONE',  ( -11.77839732991513166, 18.97803183815481987, -1.500000000000002220 ) ) ;
#19983 = EDGE_CURVE ( 'NONE', #7232, #9237, #62673, .T. ) ;
#19984 = ADVANCED_FACE ( 'NONE', ( #95720 ), #19085, .T. ) ;
#19986 = CARTESIAN_POINT ( 'NONE',  ( -59.62287095715002039, -24.51387760970724372, 9.387446482453427166 ) ) ;
#19985 = AXIS2_PLACEMENT_3D ( 'NONE', #71194, #1685, #63091 ) ;
#19987 = CARTESIAN_POINT ( 'NONE',  ( -32.38277616518237778, -25.12026506542016335, 2.831122744435439209 ) ) ;
#19988 = VERTEX_POINT ( 'NONE', #72894 ) ;
#19989 = CARTESIAN_POINT ( 'NONE',  ( -1.044871794871793602, -5.876774720514418071, 20.44941907051282115 ) ) ;
#19990 = CARTESIAN_POINT ( 'NONE',  ( 30.09341516180546350, 2.682774720514426559, -11.39311774897855756 ) ) ;
#19991 = EDGE_CURVE ( 'NONE', #53340, #2549, #33740, .T. ) ;
#19992 = CARTESIAN_POINT ( 'NONE',  ( -20.64841573231975147, 3.066018724555340746, 11.49999999999998934 ) ) ;
#19993 = ORIENTED_EDGE ( 'NONE', *, *, #59871, .T. ) ;
#19995 = ORIENTED_EDGE ( 'NONE', *, *, #73115, .T. ) ;
#19994 = LINE ( 'NONE', #27622, #6898 ) ;
#19996 = ORIENTED_EDGE ( 'NONE', *, *, #52888, .T. ) ;
#19997 = VECTOR ( 'NONE', #83543, 1000.000000000000000 ) ;
#19998 = CARTESIAN_POINT ( 'NONE',  ( -100.5847584379934716, -24.92592662359561118, 8.075495903017998245 ) ) ;
#19999 = CARTESIAN_POINT ( 'NONE',  ( 19.97611676871187569, -6.800378171449690257, -1.500000000000002220 ) ) ;
#20000 = ORIENTED_EDGE ( 'NONE', *, *, #84718, .F. ) ;
#20001 = CARTESIAN_POINT ( 'NONE',  ( -28.52287095715006870, -23.78714491118143570, -0.6496296804704170258 ) ) ;
#20002 = FACE_OUTER_BOUND ( 'NONE', #61341, .T. ) ;
#20003 = CARTESIAN_POINT ( 'NONE',  ( -115.5228709571500616, -23.48783264082477018, -1.443836473390083475 ) ) ;
#20004 = VECTOR ( 'NONE', #70575, 1000.000000000000227 ) ;
#20005 = CARTESIAN_POINT ( 'NONE',  ( -68.58953762381672448, -23.48786465467241058, 11.44779295918254647 ) ) ;
#20006 = CARTESIAN_POINT ( 'NONE',  ( -39.62287095715005592, -29.50250786944525672, 11.44777988621624232 ) ) ;
#20007 = CARTESIAN_POINT ( 'NONE',  ( 14.13103794885040898, -16.47871000921984219, -1.500000000000002220 ) ) ;
#20008 = CARTESIAN_POINT ( 'NONE',  ( -86.62287095715004170, -24.64965695001468404, 8.947790433994180503 ) ) ;
#20010 = EDGE_LOOP ( 'NONE', ( #81405, #16896, #16853, #6779 ) ) ;
#20009 = CARTESIAN_POINT ( 'NONE',  ( 1.019757120859956512, 22.21710203930399175, 11.49999999999999645 ) ) ;
#20011 = DIRECTION ( 'NONE',  ( -0.9890158633619158257, -0.1478094111296165691, -0.000000000000000000 ) ) ;
#20012 = CARTESIAN_POINT ( 'NONE',  ( -92.62287095715005592, -23.47596703998600631, 11.44779298504227860 ) ) ;
#20013 = ADVANCED_FACE ( 'NONE', ( #34325 ), #89113, .F. ) ;
#20014 = DIRECTION ( 'NONE',  ( 0.000000000000000000, 0.9999999999976377785, 2.173523156925978705E-06 ) ) ;
#20015 = ORIENTED_EDGE ( 'NONE', *, *, #80046, .F. ) ;
#20017 = VERTEX_POINT ( 'NONE', #4381 ) ;
#20016 = DIRECTION ( 'NONE',  ( 0.000000000000000000, 0.000000000000000000, 1.000000000000000000 ) ) ;
#20018 = EDGE_CURVE ( 'NONE', #12764, #18999, #63799, .T. ) ;
#20019 = ORIENTED_EDGE ( 'NONE', *, *, #59986, .T. ) ;
#20020 = PLANE ( 'NONE',  #93483 ) ;
#20021 = DIRECTION ( 'NONE',  ( 0.000000000000000000, -2.173523156925979552E-06, 0.9999999999976378895 ) ) ;
#20022 = CARTESIAN_POINT ( 'NONE',  ( -63.52287095715006160, -24.65952944569304606, 1.056160979905695463 ) ) ;
#20023 = CARTESIAN_POINT ( 'NONE',  ( -67.62287095715005592, -29.50248528299804818, 1.056150453629036701 ) ) ;
#20024 = DIRECTION ( 'NONE',  ( 0.000000000000000000, 0.000000000000000000, -1.000000000000000000 ) ) ;
#20025 = EDGE_LOOP ( 'NONE', ( #17681, #28841, #33830, #731 ) ) ;
#20026 = B_SPLINE_CURVE_WITH_KNOTS ( 'NONE', 3,
 ( #40874, #48501, #65244, #41891 ),
 .UNSPECIFIED., .F., .F.,
 ( 4, 4 ),
 ( 6.358484078632993896E-06, 0.001058107079912193370 ),
 .UNSPECIFIED. ) ;
#20028 = CARTESIAN_POINT ( 'NONE',  ( 17.66168439605153395, -8.020940556088177686, 11.49999999999999645 ) ) ;
#20027 =( REPRESENTATION_RELATIONSHIP ('NONE','NONE', #96270, #36681 ) REPRESENTATION_RELATIONSHIP_WITH_TRANSFORMATION ( #46521 )SHAPE_REPRESENTATION_RELATIONSHIP( ) );
#20030 = CARTESIAN_POINT ( 'NONE',  ( -69.52287095715006160, -23.94994826722564341, -0.6494450866342730277 ) ) ;
#20029 =( BOUNDED_SURFACE ( )  B_SPLINE_SURFACE ( 3, 2, ( 
 ( #10961, #65281, #32793 ),
 ( #63774, #73366, #95196 ),
 ( #3862, #79965, #33797 ),
 ( #65774, #2356, #33287 ) ),
 .UNSPECIFIED., .F., .F., .T. ) 
 B_SPLINE_SURFACE_WITH_KNOTS ( ( 4, 4 ),
 ( 3, 3 ),
 ( 0.004439845973569162343, 0.004703938444645663561 ),
 ( 0.000000000000000000, 1.000000000000000000 ),
 .UNSPECIFIED. ) 
 GEOMETRIC_REPRESENTATION_ITEM ( )  RATIONAL_B_SPLINE_SURFACE ( (
 ( 1.000000000000000000, 0.9005394799515968884, 1.000000000000000000),
 ( 1.000000000000000000, 0.9005352985759393913, 1.000000000000000000),
 ( 1.000000000000000000, 0.8990570573199260229, 1.000000000000000000),
 ( 1.000000000000000000, 0.8962098481621323387, 1.000000000000000000) ) ) 
 REPRESENTATION_ITEM ( '' )  SURFACE ( )  );
#20031 = CARTESIAN_POINT ( 'NONE',  ( -6.716530693746936898, -21.44081863256500142, -1.500000000000002220 ) ) ;
#20032 = ORIENTED_EDGE ( 'NONE', *, *, #1110, .T. ) ;
#20034 = CARTESIAN_POINT ( 'NONE',  ( -45.22287095715006444, -23.47593901973090169, -1.443836447538997758 ) ) ;
#20033 = AXIS2_PLACEMENT_3D ( 'NONE', #67208, #28627, #65720 ) ;
#20035 = CARTESIAN_POINT ( 'NONE',  ( 2.650685085285006348, -5.876774720514410966, 19.28073557658628445 ) ) ;
#20036 = CARTESIAN_POINT ( 'NONE',  ( -28.32169924589829080, -0.3587747205143964613, -8.244178532169451401 ) ) ;
#20038 = EDGE_CURVE ( 'NONE', #69195, #13115, #17594, .T. ) ;
#20037 = CARTESIAN_POINT ( 'NONE',  ( -130.5728709571500588, -24.47917135695840685, 9.440663514584123561 ) ) ;
#20039 = CARTESIAN_POINT ( 'NONE',  ( -0.6043519431218743465, -19.59835197619436187, 11.49999999999998934 ) ) ;
#20040 = AXIS2_PLACEMENT_3D ( 'NONE', #36495, #84164, #53236 ) ;
#20041 = CARTESIAN_POINT ( 'NONE',  ( 8.671512145086499146, -1.000000000000000222, 3.746884140868835367 ) ) ;
#20042 = VERTEX_POINT ( 'NONE', #4874 ) ;
#20043 = CARTESIAN_POINT ( 'NONE',  ( -14.25192491085926072, -16.12266454619898326, -1.500000000000002220 ) ) ;
#20044 = CARTESIAN_POINT ( 'NONE',  ( -121.5895376238167387, -23.48783264082478794, -1.443836473390058384 ) ) ;
#20045 = CARTESIAN_POINT ( 'NONE',  ( -81.14580165399679856, -25.31572674173500914, 5.096590159266133568 ) ) ;
#20046 = CARTESIAN_POINT ( 'NONE',  ( 30.93860345374796594, -0.6647747205144264315, 19.84760796525321780 ) ) ;
#20047 = EDGE_CURVE ( 'NONE', #40585, #55689, #88199, .T. ) ;
#20048 = DIRECTION ( 'NONE',  ( 0.000000000000000000, 2.173523156893721996E-06, -0.9999999999976377785 ) ) ;
#20049 = CARTESIAN_POINT ( 'NONE',  ( -6.529369910325518944, -22.02198592821369516, -1.500000000000002220 ) ) ;
#20050 = COORDINATED_UNIVERSAL_TIME_OFFSET ( 0, 0, .AHEAD. ) ;
#20051 = CARTESIAN_POINT ( 'NONE',  ( -46.62287095715004881, -24.66019654487198665, 8.947790411086135265 ) ) ;
#20052 = CARTESIAN_POINT ( 'NONE',  ( -53.50203224161664650, -24.15543982623906771, -0.2315651400026670914 ) ) ;
#20053 = CARTESIAN_POINT ( 'NONE',  ( -7.946508460909448956, -18.53024980520100939, 11.49999999999999645 ) ) ;
#20054 = CARTESIAN_POINT ( 'NONE',  ( -109.4252266130965552, -25.28814134756654397, 3.135431506998875406 ) ) ;
#20055 = CARTESIAN_POINT ( 'NONE',  ( -25.92875734969026169, -5.356774720514426491, 23.50402280011861933 ) ) ;
#20056 = CARTESIAN_POINT ( 'NONE',  ( -4.177535645411178500, -5.876774720514415407, 20.17598923696320767 ) ) ;
#20057 = CARTESIAN_POINT ( 'NONE',  ( -113.5228709571500758, -23.48783264082477373, -1.443836473390082586 ) ) ;
#20058 = CARTESIAN_POINT ( 'NONE',  ( 15.22325621495362391, 2.682774720514426559, -27.23549315679322547 ) ) ;
#20059 = CARTESIAN_POINT ( 'NONE',  ( -15.96263503330635380, 11.84234753045382682, -1.500000000000002220 ) ) ;
#20060 = CARTESIAN_POINT ( 'NONE',  ( -113.5528542040558051, -24.34968618360933945, 0.1864209137778880254 ) ) ;
#20061 = CARTESIAN_POINT ( 'NONE',  ( -19.67082186522023690, -1.387426831159568108, -1.500000000000002220 ) ) ;
#20062 = CARTESIAN_POINT ( 'NONE',  ( -126.5902073615529133, -23.96169478059714564, 10.65365249895716637 ) ) ;
#20063 = CARTESIAN_POINT ( 'NONE',  ( -125.6228709571501128, -24.62285846362216546, 9.038163152653524435 ) ) ;
#20064 = CARTESIAN_POINT ( 'NONE',  ( -79.52287095715006160, -23.47596703998600631, 11.44779298504228571 ) ) ;
#20065 = CARTESIAN_POINT ( 'NONE',  ( -9.109090448966927767, 18.51201596650851400, 11.49999999999999645 ) ) ;
#20066 = CARTESIAN_POINT ( 'NONE',  ( -39.22484595018107711, -25.27985428963552650, 4.963673027505932644 ) ) ;
#20067 = CARTESIAN_POINT ( 'NONE',  ( -24.90875734969025501, 0.3587747205144265483, 26.43402280011862615 ) ) ;
#20068 = CIRCLE ( 'NONE', #52453, 3.060000000000000053 ) ;
#20069 = CARTESIAN_POINT ( 'NONE',  ( -21.16080155796574047, 8.166215375980355518, 11.49999999999999645 ) ) ;
#20070 = VERTEX_POINT ( 'NONE', #51054 ) ;
#20071 = CARTESIAN_POINT ( 'NONE',  ( -29.62287096154833677, -23.39681786206389447, 11.44779298504227860 ) ) ;
#20072 = CARTESIAN_POINT ( 'NONE',  ( 30.62809631291915835, 4.628857374213141362, 27.84496821199607908 ) ) ;
#20073 = AXIS2_PLACEMENT_3D ( 'NONE', #5933, #67853, #83553 ) ;
#20074 = CARTESIAN_POINT ( 'NONE',  ( -63.52208789522248367, -23.48783264082476308, -1.443836473390093245 ) ) ;
#20075 = CARTESIAN_POINT ( 'NONE',  ( -2.599001758237162285, -6.376774720514413630, 19.60308799987317485 ) ) ;
#20076 = VERTEX_POINT ( 'NONE', #82484 ) ;
#20077 = EDGE_LOOP ( 'NONE', ( #31064, #12250, #88654, #85242, #65431, #75278 ) ) ;
#20078 = PLANE ( 'NONE',  #54983 ) ;
#20079 = CARTESIAN_POINT ( 'NONE',  ( -20.58715743568940226, -9.973749938417524774, -1.500000000000002220 ) ) ;
#20080 = FACE_OUTER_BOUND ( 'NONE', #9741, .T. ) ;
#20081 = CARTESIAN_POINT ( 'NONE',  ( 15.46703529437019853, -15.08741104398349187, -1.500000000000002220 ) ) ;
#20082 = DIRECTION ( 'NONE',  ( -0.000000000000000000, -1.000000000000000000, -0.000000000000000000 ) ) ;
#20083 = CARTESIAN_POINT ( 'NONE',  ( -50.62287095715005592, -29.50248789122583659, 2.256150453626215580 ) ) ;
#20084 = CARTESIAN_POINT ( 'NONE',  ( 22.38532167473930556, -2.757513164441831144, 11.49999999999999645 ) ) ;
#20085 = ORIENTED_EDGE ( 'NONE', *, *, #37579, .F. ) ;
#20086 = FACE_OUTER_BOUND ( 'NONE', #18424, .T. ) ;
#20087 = CARTESIAN_POINT ( 'NONE',  ( 21.52718982488130450, -4.553922534329950089, 11.49999999999998934 ) ) ;
#20088 = FACE_OUTER_BOUND ( 'NONE', #18278, .T. ) ;
#20089 = LINE ( 'NONE', #58173, #58416 ) ;
#20091 = ORIENTED_EDGE ( 'NONE', *, *, #54413, .T. ) ;
#20090 = EDGE_CURVE ( 'NONE', #97596, #51332, #75363, .T. ) ;
#20092 = CARTESIAN_POINT ( 'NONE',  ( 19.75748517575715368, -0.3587747205144265483, 28.87153971905864580 ) ) ;
#20093 = DIRECTION ( 'NONE',  ( 0.000000000000000000, 0.000000000000000000, 1.000000000000000000 ) ) ;
#20094 = ORIENTED_EDGE ( 'NONE', *, *, #59473, .T. ) ;
#20095 = CARTESIAN_POINT ( 'NONE',  ( -49.58953762381672448, -23.48786465467241058, 11.44779295918254824 ) ) ;
#20096 = EDGE_CURVE ( 'NONE', #100230, #5942, #14302, .T. ) ;
#20097 = VERTEX_POINT ( 'NONE', #27712 ) ;
#20098 = ORIENTED_EDGE ( 'NONE', *, *, #17015, .T. ) ;
#20099 = ORIENTED_EDGE ( 'NONE', *, *, #96521, .F. ) ;
#20100 = CARTESIAN_POINT ( 'NONE',  ( -49.28565304951956705, -25.27399216425258643, 6.009773539330731218 ) ) ;
#20101 = DIRECTION ( 'NONE',  ( 3.773278334444167608E-23, -1.000000000000000000, 0.000000000000000000 ) ) ;
#20102 = FACE_OUTER_BOUND ( 'NONE', #73227, .T. ) ;
#20103 = CARTESIAN_POINT ( 'NONE',  ( 18.38310620586021571, 8.829655622120887060, -1.500000000000002220 ) ) ;
#20104 = AXIS2_PLACEMENT_3D ( 'NONE', #23190, #72764, #47054 ) ;
#20105 = ADVANCED_FACE ( 'NONE', ( #83982 ), #28206, .T. ) ;
#20106 = ORIENTED_EDGE ( 'NONE', *, *, #60001, .F. ) ;
#20107 = PLANE ( 'NONE',  #10465 ) ;
#20108 = CARTESIAN_POINT ( 'NONE',  ( -88.62287095715001328, -23.73907113216992215, -1.053371485793224371 ) ) ;
#20109 = ADVANCED_FACE ( 'NONE', ( #14461 ), #68270, .T. ) ;
#20110 = CARTESIAN_POINT ( 'NONE',  ( -97.52287095715004739, -23.72747288104470087, -1.053458166803225460 ) ) ;
#20111 = DIRECTION ( 'NONE',  ( 0.000000000000000000, -0.9999999999976377785, -2.173523156925979975E-06 ) ) ;
#20112 = ORIENTED_EDGE ( 'NONE', *, *, #21897, .T. ) ;
#20113 = CARTESIAN_POINT ( 'NONE',  ( -29.00221282414159418, -25.21531865948820084, 3.230369517096869370 ) ) ;
#20115 = VECTOR ( 'NONE', #8361, 1000.000000000000000 ) ;
#20114 = CARTESIAN_POINT ( 'NONE',  ( -33.52287095715006160, -24.65952944569303895, 1.056160979905690134 ) ) ;
#20116 = EDGE_CURVE ( 'NONE', #28117, #10751, #88119, .T. ) ;
#20117 = ORIENTED_EDGE ( 'NONE', *, *, #5693, .F. ) ;
#20118 = EDGE_CURVE ( 'NONE', #63848, #93973, #69190, .T. ) ;
#20119 = CARTESIAN_POINT ( 'NONE',  ( -16.26442346200556344, 12.93145763113255775, -1.500000000000002220 ) ) ;
#20120 = VERTEX_POINT ( 'NONE', #22070 ) ;
#20122 = VERTEX_POINT ( 'NONE', #66794 ) ;
#20121 = CARTESIAN_POINT ( 'NONE',  ( -40.29361789974588959, -25.30535304242862082, 5.078340751659213836 ) ) ;
#20123 = CARTESIAN_POINT ( 'NONE',  ( -107.6228709571500701, -29.50250786944525672, 11.44777988621622988 ) ) ;
#20124 = CARTESIAN_POINT ( 'NONE',  ( -129.6234738311520971, -24.66019654487200086, 8.947790411086113949 ) ) ;
#20125 = VERTEX_POINT ( 'NONE', #83478 ) ;
#20126 = ORIENTED_EDGE ( 'NONE', *, *, #6284, .T. ) ;
#20127 = FACE_OUTER_BOUND ( 'NONE', #84014, .T. ) ;
#20128 = CARTESIAN_POINT ( 'NONE',  ( -121.5228709571500048, -23.47593901973090524, -1.443836447538996204 ) ) ;
#20129 = CARTESIAN_POINT ( 'NONE',  ( -55.58953762381672448, -23.48783264082478084, -1.443836473390068820 ) ) ;
#20130 = CARTESIAN_POINT ( 'NONE',  ( -71.30358265130861639, -25.24515230220021422, 6.178525869656843916 ) ) ;
#20132 = EDGE_LOOP ( 'NONE', ( #33237, #80496, #5578, #87474 ) ) ;
#20131 = CARTESIAN_POINT ( 'NONE',  ( 19.10104996495751450, -11.12853483292915691, 11.49999999999999645 ) ) ;
#20133 = DIRECTION ( 'NONE',  ( 0.000000000000000000, 0.000000000000000000, 1.000000000000000000 ) ) ;
#20134 = CARTESIAN_POINT ( 'NONE',  ( -15.94491270116497184, -16.04792668696150315, 11.49999999999998934 ) ) ;
#20136 = ORIENTED_EDGE ( 'NONE', *, *, #35385, .T. ) ;
#20135 = DIRECTION ( 'NONE',  ( 0.000000000000000000, 0.000000000000000000, 1.000000000000000000 ) ) ;
#20137 = ORIENTED_EDGE ( 'NONE', *, *, #48524, .T. ) ;
#20138 = CARTESIAN_POINT ( 'NONE',  ( -78.58953762381672448, -24.66019654487198665, 8.947790411086133489 ) ) ;
#20139 = B_SPLINE_CURVE_WITH_KNOTS ( 'NONE', 3,
 ( #43853, #57592, #10905, #73796, #88529, #41868 ),
 .UNSPECIFIED., .F., .F.,
 ( 4, 2, 4 ),
 ( 0.000000000000000000, 0.001380901958385391580, 0.002761803916770783161 ),
 .UNSPECIFIED. ) ;
#20140 = B_SPLINE_SURFACE_WITH_KNOTS ( 'NONE', 3, 1, ( 
 ( #72546, #25858 ),
 ( #95371, #49220 ),
 ( #56833, #3038 ),
 ( #57337, #74039 ),
 ( #42604, #19730 ),
 ( #35482, #57829 ),
 ( #43096, #65950 ),
 ( #89262, #80651 ),
 ( #26364, #42105 ),
 ( #87766, #66454 ),
 ( #41600, #18739 ),
 ( #58325, #4535 ),
 ( #4032, #34976 ),
 ( #11136, #50207 ) ),
 .UNSPECIFIED., .F., .F., .F.,
 ( 4, 2, 2, 2, 2, 2, 4 ),
 ( 2, 2 ),
 ( 0.000000000000000000, 0.2500000000000001110, 0.3750000000000001110, 0.5000000000000002220, 0.6250000000000003331, 0.7500000000000004441, 1.000000000000000000 ),
 ( 0.000000000000000000, 1.000000000000000000 ),
 .UNSPECIFIED. ) ;
#20141 = CARTESIAN_POINT ( 'NONE',  ( -57.64983551063303224, -23.73791477778911840, 11.05961554403170588 ) ) ;
#20142 = ORIENTED_EDGE ( 'NONE', *, *, #80614, .F. ) ;
#20143 = CARTESIAN_POINT ( 'NONE',  ( -14.54676392617323266, -15.37779485849079464, 11.49999999999998934 ) ) ;
#20144 = CARTESIAN_POINT ( 'NONE',  ( -40.01839366089613748, -25.29345411398207943, 5.509688073139549225 ) ) ;
#20145 = CARTESIAN_POINT ( 'NONE',  ( 8.793911523065595759, -20.50603677605392150, -1.500000000000002220 ) ) ;
#20146 = CARTESIAN_POINT ( 'NONE',  ( 14.61581670307174008, -6.376774720514426953, -27.35847990810646024 ) ) ;
#20147 = ORIENTED_EDGE ( 'NONE', *, *, #86883, .F. ) ;
#20148 = CARTESIAN_POINT ( 'NONE',  ( -123.6228709571500559, -24.64898659630368627, 1.056161002820833028 ) ) ;
#20149 = FACE_OUTER_BOUND ( 'NONE', #52712, .T. ) ;
#20150 = DIRECTION ( 'NONE',  ( 0.000000000000000000, 0.000000000000000000, -1.000000000000000000 ) ) ;
#20151 = CARTESIAN_POINT ( 'NONE',  ( -83.55620429048336462, -24.64965694238574301, 8.947790433994201820 ) ) ;
#20152 = CARTESIAN_POINT ( 'NONE',  ( -18.49313839071750820, -6.238557295281221826, 11.49999999999998934 ) ) ;
#20153 = CARTESIAN_POINT ( 'NONE',  ( 17.37860173834871347, 12.56526366372364301, -1.500000000000002220 ) ) ;
#20154 = CARTESIAN_POINT ( 'NONE',  ( -26.98755670591954114, -24.92774695839280241, 1.764414538584399894 ) ) ;
#20155 = CARTESIAN_POINT ( 'NONE',  ( -112.6228709571500559, -29.50247984919015209, -1.443849546365048253 ) ) ;
#20156 = CARTESIAN_POINT ( 'NONE',  ( -115.5228709571500616, -24.99132157543084531, 2.256160258750667502 ) ) ;
#20157 = ADVANCED_FACE ( 'NONE', ( #20086 ), #28071, .T. ) ;
#20159 = VECTOR ( 'NONE', #23292, 1000.000000000000000 ) ;
#20158 = CARTESIAN_POINT ( 'NONE',  ( -10.93939140624874007, -20.02795264745160608, -1.500000000000002220 ) ) ;
#20160 = EDGE_CURVE ( 'NONE', #92435, #31493, #75615, .T. ) ;
#20161 = CALENDAR_DATE ( 2026, 9, 10 ) ;
#20162 = CARTESIAN_POINT ( 'NONE',  ( -46.52287095715006160, -24.65952944569304606, 1.056160979905693686 ) ) ;
#20163 = CARTESIAN_POINT ( 'NONE',  ( 8.671512145086502699, -1.000000000000001998, -3.746884140868835367 ) ) ;
#20164 = CARTESIAN_POINT ( 'NONE',  ( -19.52388446859773552, -3.948942086532154061, 11.49999999999999645 ) ) ;
#20165 = CARTESIAN_POINT ( 'NONE',  ( -69.52287095715010423, -23.96127896941631974, -0.6493128931038036900 ) ) ;
#20166 = FACE_OUTER_BOUND ( 'NONE', #89490, .T. ) ;
#20167 = DIRECTION ( 'NONE',  ( -1.000000000000000000, -3.773278334444166432E-23, -8.201307841325785021E-29 ) ) ;
#20168 = ORIENTED_EDGE ( 'NONE', *, *, #66521, .T. ) ;
#20169 = CARTESIAN_POINT ( 'NONE',  ( -25.63707821144803845, -24.86039540779550094, 3.655391356329271257 ) ) ;
#20170 = LINE ( 'NONE', #51132, #15060 ) ;
#20171 = AXIS2_PLACEMENT_3D ( 'NONE', #71410, #64322, #24221 ) ;
#20172 = CARTESIAN_POINT ( 'NONE',  ( 0.4029737066630413311, -21.70969715354747009, -1.500000000000002220 ) ) ;
#20173 = CARTESIAN_POINT ( 'NONE',  ( -88.88918693012689687, -25.25676012837779183, 6.101892527513559372 ) ) ;
#20174 = CARTESIAN_POINT ( 'NONE',  ( -19.49195742049215241, -1.735909528584683947, -1.500000000000002220 ) ) ;
#20175 = DIRECTION ( 'NONE',  ( 3.773278334444166432E-23, -1.000000000000000000, 0.000000000000000000 ) ) ;
#20176 = VERTEX_POINT ( 'NONE', #62663 ) ;
#20177 = APPROVAL_DATE_TIME ( #90696, #78479 ) ;
#20178 = CARTESIAN_POINT ( 'NONE',  ( 2.499999999999995115, 19.99999999999999645, 2.100000000000000089 ) ) ;
#20179 = CARTESIAN_POINT ( 'NONE',  ( -17.38880980700008294, 10.71821138944157603, 11.49999999999999645 ) ) ;
#20180 = CARTESIAN_POINT ( 'NONE',  ( -49.28019047777514317, -25.25808854711805651, 6.078199934834979778 ) ) ;
#20181 = EDGE_CURVE ( 'NONE', #1269, #56546, #30042, .T. ) ;
#20182 = DIRECTION ( 'NONE',  ( 0.000000000000000000, 0.000000000000000000, 1.000000000000000000 ) ) ;
#20183 = ORIENTED_EDGE ( 'NONE', *, *, #91792, .T. ) ;
#20184 = CARTESIAN_POINT ( 'NONE',  ( -4.926336369345162502, -0.3587747205143967943, -28.61095484066305161 ) ) ;
#20185 = CARTESIAN_POINT ( 'NONE',  ( 0.1011420733776737524, 1.446399035885977957, 8.999999999999987566 ) ) ;
#20186 = CARTESIAN_POINT ( 'NONE',  ( -116.6298700828398864, -23.48786465467241769, 11.44779295918253759 ) ) ;
#20187 = CARTESIAN_POINT ( 'NONE',  ( -109.5906689592580108, -24.15543982623907482, -0.2315651400026587092 ) ) ;
#20188 = ORIENTED_EDGE ( 'NONE', *, *, #26083, .F. ) ;
#20189 = CARTESIAN_POINT ( 'NONE',  ( 6.059061188053544988, -6.376774720514417183, 20.16803580207560742 ) ) ;
#20190 = B_SPLINE_CURVE_WITH_KNOTS ( 'NONE', 3,
 ( #76583, #61394, #92816, #22790 ),
 .UNSPECIFIED., .F., .F.,
 ( 4, 4 ),
 ( 0.4808433584723854071, 0.4898497897445006632 ),
 .UNSPECIFIED. ) ;
#20191 = CARTESIAN_POINT ( 'NONE',  ( -21.58539018223340022, -8.019882488244659768, 11.49999999999999645 ) ) ;
#20192 = CARTESIAN_POINT ( 'NONE',  ( -21.69093436787670726, -6.948586514802197023, -1.500000000000002220 ) ) ;
#20193 = CARTESIAN_POINT ( 'NONE',  ( -70.35039385224574460, -25.31517373849778352, 4.853613849468179531 ) ) ;
#20194 = CARTESIAN_POINT ( 'NONE',  ( -110.6228709571500559, -29.50247984919015209, -1.443849546365048253 ) ) ;
#20195 = LINE ( 'NONE', #43056, #38737 ) ;
#20196 = VECTOR ( 'NONE', #59117, 1000.000000000000000 ) ;
#20197 = CARTESIAN_POINT ( 'NONE',  ( -70.52287095715009002, -24.63287334234179582, 0.9662140553045422964 ) ) ;
#20198 = FACE_OUTER_BOUND ( 'NONE', #49851, .T. ) ;
#20199 = CARTESIAN_POINT ( 'NONE',  ( 9.607415760296678542, -19.69187540195887465, -1.500000000000002220 ) ) ;
#20200 = CARTESIAN_POINT ( 'NONE',  ( -87.55620429048337883, -24.65952944569304606, 1.056160979905701902 ) ) ;
#20201 = CARTESIAN_POINT ( 'NONE',  ( -0.3244794670026783234, -9.612687562450236811, 9.000000000000000000 ) ) ;
#20202 = FACE_OUTER_BOUND ( 'NONE', #14818, .T. ) ;
#20203 = DIRECTION ( 'NONE',  ( -0.000000000000000000, -1.000000000000000000, 0.000000000000000000 ) ) ;
#20204 = VERTEX_POINT ( 'NONE', #77849 ) ;
#20205 = CARTESIAN_POINT ( 'NONE',  ( -16.87313589883980214, -11.49665204554024989, -1.500000000000002220 ) ) ;
#20206 = ORIENTED_EDGE ( 'NONE', *, *, #57500, .F. ) ;
#20207 = VERTEX_POINT ( 'NONE', #92091 ) ;
#20208 = ORIENTED_EDGE ( 'NONE', *, *, #36592, .T. ) ;
#20209 = EDGE_LOOP ( 'NONE', ( #59996, #56442 ) ) ;
#20210 = CARTESIAN_POINT ( 'NONE',  ( -1.973530150111237003, 22.95712487800313539, -1.500000000000002220 ) ) ;
#20211 = CARTESIAN_POINT ( 'NONE',  ( 8.160000000000000142, 2.888964624466060727, -0.2527516539682188590 ) ) ;
#20212 = CARTESIAN_POINT ( 'NONE',  ( 18.82617747125253871, -7.458514806974097411, -1.500000000000002220 ) ) ;
#20213 = EDGE_CURVE ( 'NONE', #41039, #48956, #46526, .T. ) ;
#20214 = ORIENTED_EDGE ( 'NONE', *, *, #17646, .F. ) ;
#20215 = LINE ( 'NONE', #75001, #57429 ) ;
#20216 = CARTESIAN_POINT ( 'NONE',  ( -48.52287095715006160, -24.66019654487200086, 8.947790411086119278 ) ) ;
#20217 = ADVANCED_FACE ( 'NONE', ( #84482 ), #42650, .T. ) ;
#20218 = CARTESIAN_POINT ( 'NONE',  ( -95.50969526946468591, -24.40034930558991633, 0.3402023900116099009 ) ) ;
#20219 = CARTESIAN_POINT ( 'NONE',  ( -41.62287095715006302, -24.64965695001467694, 8.947790433994187609 ) ) ;
#20221 = ORIENTED_EDGE ( 'NONE', *, *, #66082, .T. ) ;
#20220 = CARTESIAN_POINT ( 'NONE',  ( 7.684279652734260502, -19.92951104315265809, 11.49999999999999645 ) ) ;
#20222 = CARTESIAN_POINT ( 'NONE',  ( 7.041152093163508319, -5.876774720514424288, 21.17127001373575368 ) ) ;
#20223 = EDGE_CURVE ( 'NONE', #40883, #35091, #61522, .T. ) ;
#20224 = ORIENTED_EDGE ( 'NONE', *, *, #2700, .F. ) ;
#20225 = CARTESIAN_POINT ( 'NONE',  ( 14.63995501510512653, -16.76770752772931772, 11.49999999999998934 ) ) ;
#20226 = EDGE_CURVE ( 'NONE', #31854, #53293, #42126, .T. ) ;
#20227 = CARTESIAN_POINT ( 'NONE',  ( -16.33875328525262560, 12.67428768300982256, -1.500000000000002220 ) ) ;
#20228 = VECTOR ( 'NONE', #21920, 1000.000000000000000 ) ;
#20229 = ORIENTED_EDGE ( 'NONE', *, *, #4654, .F. ) ;
#20230 = CARTESIAN_POINT ( 'NONE',  ( -69.86193069524509269, -25.03707830618030172, 7.590867772707288630 ) ) ;
#20231 = ORIENTED_EDGE ( 'NONE', *, *, #98722, .T. ) ;
#20232 = CARTESIAN_POINT ( 'NONE',  ( 31.84105487026623393, 5.152774720514427642, -11.95870468328481806 ) ) ;
#20233 = ORIENTED_EDGE ( 'NONE', *, *, #52617, .F. ) ;
#20234 = CARTESIAN_POINT ( 'NONE',  ( -17.98194200498208062, 10.70670730041394947, -1.500000000000002220 ) ) ;
#20235 = ADVANCED_FACE ( 'NONE', ( #63670 ), #18966, .F. ) ;
#20236 = CARTESIAN_POINT ( 'NONE',  ( 18.32745805453730981, -11.99952526121574259, 11.49999999999999645 ) ) ;
#20237 = AXIS2_PLACEMENT_3D ( 'NONE', #81147, #3534, #66450 ) ;
#20238 = CARTESIAN_POINT ( 'NONE',  ( -89.62590178745654157, -24.51419770103157703, 9.386484678747175181 ) ) ;
#20239 = CARTESIAN_POINT ( 'NONE',  ( -10.06026007034034464, -20.14757889648583244, -1.500000000000002220 ) ) ;
#20240 = CARTESIAN_POINT ( 'NONE',  ( 15.12549221760053086, 14.48511125727034177, -1.500000000000002220 ) ) ;
#20241 = DIRECTION ( 'NONE',  ( 1.000000000000000000, 3.773278334444166432E-23, 8.201307841325785021E-29 ) ) ;
#20242 = LINE ( 'NONE', #43103, #25383 ) ;
#20243 = DIRECTION ( 'NONE',  ( -0.000000000000000000, 1.000000000000000000, -0.000000000000000000 ) ) ;
#20244 = DIRECTION ( 'NONE',  ( 0.000000000000000000, 0.000000000000000000, 1.000000000000000000 ) ) ;
#20245 = VERTEX_POINT ( 'NONE', #65672 ) ;
#20246 = B_SPLINE_CURVE_WITH_KNOTS ( 'NONE', 3,
 ( #25692, #81486, #79978, #10464, #48553, #49547, #66277, #80477 ),
 .UNSPECIFIED., .F., .F.,
 ( 4, 2, 2, 4 ),
 ( 6.384118678614035137E-06, 0.002007151183507257120, 0.003007534715921580341, 0.004007918248335903127 ),
 .UNSPECIFIED. ) ;
#20247 = ORIENTED_EDGE ( 'NONE', *, *, #16028, .F. ) ;
#20248 = EDGE_LOOP ( 'NONE', ( #29225, #86890, #22963, #16304 ) ) ;
#20249 = PLANE ( 'NONE',  #64491 ) ;
#20250 = CARTESIAN_POINT ( 'NONE',  ( -16.43003769262999469, -13.82051474754189258, -1.500000000000002220 ) ) ;
#20251 = PLANE ( 'NONE',  #11621 ) ;
#20252 = ORIENTED_EDGE ( 'NONE', *, *, #17141, .T. ) ;
#20253 = CARTESIAN_POINT ( 'NONE',  ( -17.90976863334866920, 11.11529090135583075, 11.49999999999998934 ) ) ;
#20254 = CARTESIAN_POINT ( 'NONE',  ( -36.52287095715006870, -24.65952944569304606, 1.056160979905691910 ) ) ;
#20255 = CARTESIAN_POINT ( 'NONE',  ( 3.474198977381013798, -6.376774720514426065, 21.79108561604954986 ) ) ;
#20256 = DIRECTION ( 'NONE',  ( -3.773278334444167608E-23, 1.000000000000000000, 0.000000000000000000 ) ) ;
#20257 = CARTESIAN_POINT ( 'NONE',  ( 7.805843057017202824, -6.475225279485576024, -27.15467198446602026 ) ) ;
#20258 = CARTESIAN_POINT ( 'NONE',  ( -90.62287095715004170, -24.99156045073392818, 7.747789690856161648 ) ) ;
#20259 = CARTESIAN_POINT ( 'NONE',  ( -16.97254739485517661, -14.18817111035334655, -1.500000000000002220 ) ) ;
#20260 = CARTESIAN_POINT ( 'NONE',  ( -58.62287095715004881, -29.50250786944525672, 11.44777988621623876 ) ) ;
#20261 = CARTESIAN_POINT ( 'NONE',  ( -3.054691362729579751, -6.376774720514413630, 19.78730719034165375 ) ) ;
#20262 = CARTESIAN_POINT ( 'NONE',  ( -60.57607103537276316, -25.00158670708909980, 2.256160236439220146 ) ) ;
#20263 = ADVANCED_FACE ( 'NONE', ( #41312 ), #94590, .T. ) ;
#20264 = CARTESIAN_POINT ( 'NONE',  ( 0.000000000000000000, 1.826774720514426464, 0.000000000000000000 ) ) ;
#20265 = VECTOR ( 'NONE', #49530, 1000.000000000000114 ) ;
#20266 = CARTESIAN_POINT ( 'NONE',  ( 13.34776491790984210, -16.67230741956907991, -1.500000000000002220 ) ) ;
#20267 = CARTESIAN_POINT ( 'NONE',  ( -113.5228709571500616, -23.48786465467242479, 11.44779295918253936 ) ) ;
#20268 = FACE_BOUND ( 'NONE', #60568, .T. ) ;
#20269 = EDGE_CURVE ( 'NONE', #26877, #57581, #74800, .T. ) ;
#20270 = CARTESIAN_POINT ( 'NONE',  ( 30.53060340732035982, -1.682774720514426114, -1.272392034746785860 ) ) ;
#20271 = LINE ( 'NONE', #37010, #91339 ) ;
#20272 = CARTESIAN_POINT ( 'NONE',  ( -20.48750165597241590, 9.616757810196778777, -1.500000000000002220 ) ) ;
#20273 = ORIENTED_EDGE ( 'NONE', *, *, #51731, .T. ) ;
#20274 = CARTESIAN_POINT ( 'NONE',  ( 3.902919446070569176, -5.876774720514426953, 21.47497695444087284 ) ) ;
#20275 = CARTESIAN_POINT ( 'NONE',  ( -79.50175546033953822, -24.51314013834316086, 0.6176544820404135105 ) ) ;
#20276 = CARTESIAN_POINT ( 'NONE',  ( 19.18382676146983457, -4.683391092530263755, 11.49999999999999645 ) ) ;
#20277 = LINE ( 'NONE', #43636, #34277 ) ;
#20278 = CARTESIAN_POINT ( 'NONE',  ( -67.58378879032223097, -24.51314013834315730, 0.6176544820404126224 ) ) ;
#20279 = ORIENTED_EDGE ( 'NONE', *, *, #76901, .T. ) ;
#20280 = FACE_OUTER_BOUND ( 'NONE', #11885, .T. ) ;
#20281 = CARTESIAN_POINT ( 'NONE',  ( 22.81105451610979173, -1.475225279485572916, -17.31691820600746823 ) ) ;
#20282 = DIRECTION ( 'NONE',  ( 1.000000000000000000, 0.000000000000000000, 0.000000000000000000 ) ) ;
#20283 = CARTESIAN_POINT ( 'NONE',  ( -7.466173891270859286, -20.28576548065916541, 11.49999999999998934 ) ) ;
#20284 = CARTESIAN_POINT ( 'NONE',  ( -49.10668015502195516, -25.10935369951826956, 3.950018049247062457 ) ) ;
#20285 = CARTESIAN_POINT ( 'NONE',  ( -9.899997732206244905, -16.63842163800745766, -1.500000000000002220 ) ) ;
#20286 = CARTESIAN_POINT ( 'NONE',  ( -92.52287095715006160, -23.48783264083452593, -1.443836473374927820 ) ) ;
#20287 = CARTESIAN_POINT ( 'NONE',  ( -85.58953762381671027, -25.00182538069145366, 7.747789668545099317 ) ) ;
#20288 = CARTESIAN_POINT ( 'NONE',  ( -15.51018552496569392, -12.33189742059753868, 11.49999999999998934 ) ) ;
#20289 = ORIENTED_EDGE ( 'NONE', *, *, #22177, .T. ) ;
#20290 = B_SPLINE_CURVE_WITH_KNOTS ( 'NONE', 3,
 ( #66802, #97229, #97723, #35338, #5871, #74385 ),
 .UNSPECIFIED., .F., .F.,
 ( 4, 2, 4 ),
 ( 0.000000000000000000, 0.001380764517853252504, 0.002761529035706505007 ),
 .UNSPECIFIED. ) ;
#20291 = CARTESIAN_POINT ( 'NONE',  ( -6.888417027594036846, 19.07602104198033643, 11.49999999999999645 ) ) ;
#20292 = CARTESIAN_POINT ( 'NONE',  ( -88.52287095715006160, -29.50248528299804818, 1.056150453629040253 ) ) ;
#20293 = VECTOR ( 'NONE', #83595, 1000.000000000000114 ) ;
#20294 = CC_DESIGN_PERSON_AND_ORGANIZATION_ASSIGNMENT ( #66368, #5440, ( #87801 ) ) ;
#20295 = CARTESIAN_POINT ( 'NONE',  ( 5.981014360695730225, -6.376774720514426065, 21.36744920115099333 ) ) ;
#20296 = VERTEX_POINT ( 'NONE', #32689 ) ;
#20297 = CARTESIAN_POINT ( 'NONE',  ( -37.52287095715006160, -24.35013146730203815, 9.818937971375104823 ) ) ;
#20298 = CARTESIAN_POINT ( 'NONE',  ( 13.86067930708168738, -5.152774720514425866, -28.23766061416633022 ) ) ;
#20299 = FACE_OUTER_BOUND ( 'NONE', #84220, .T. ) ;
#20300 = CARTESIAN_POINT ( 'NONE',  ( -80.52287095715006160, -24.99132157543083821, 2.256160258750667502 ) ) ;
#20301 = DIRECTION ( 'NONE',  ( -3.773278334453079030E-23, 0.9999999999976377785, 2.173523156925979128E-06 ) ) ;
#20302 = CARTESIAN_POINT ( 'NONE',  ( 20.03642891561555928, 0.6179553080306146029, 11.49999999999998934 ) ) ;
#20303 = AXIS2_PLACEMENT_3D ( 'NONE', #33613, #56968, #73674 ) ;
#20304 = LINE ( 'NONE', #67018, #49952 ) ;
#20305 = ORIENTED_EDGE ( 'NONE', *, *, #62145, .F. ) ;
#20306 = ADVANCED_FACE ( 'NONE', ( #57551 ), #49943, .T. ) ;
#20307 = VECTOR ( 'NONE', #85107, 1000.000000000000000 ) ;
#20308 = CARTESIAN_POINT ( 'NONE',  ( -103.5228709571500474, -24.66019654487200441, 8.947790411086119278 ) ) ;
#20309 = CARTESIAN_POINT ( 'NONE',  ( -127.5228709571500616, -24.33832256527049154, 0.1851278514138698372 ) ) ;
#20310 = LINE ( 'NONE', #51281, #42188 ) ;
#20311 = FACE_OUTER_BOUND ( 'NONE', #68062, .T. ) ;
#20312 = LINE ( 'NONE', #83723, #39705 ) ;
#20313 = DIRECTION ( 'NONE',  ( 0.000000000000000000, 1.000000000000000000, 0.000000000000000000 ) ) ;
#20314 = ORIENTED_EDGE ( 'NONE', *, *, #82552, .F. ) ;
#20315 = CARTESIAN_POINT ( 'NONE',  ( -5.305567426876419468, 19.62801697144059787, -1.500000000000002220 ) ) ;
#20316 = ORIENTED_EDGE ( 'NONE', *, *, #98598, .T. ) ;
#20317 = EDGE_CURVE ( 'NONE', #57723, #9882, #33562, .T. ) ;
#20318 = B_SPLINE_CURVE_WITH_KNOTS ( 'NONE', 3,
 ( #99629, #61107, #69203, #100118 ),
 .UNSPECIFIED., .F., .F.,
 ( 4, 4 ),
 ( 0.4791111652815406852, 0.4801119123223059892 ),
 .UNSPECIFIED. ) ;
#20319 = CARTESIAN_POINT ( 'NONE',  ( 20.38051395842347802, -10.57019977742728578, -1.500000000000002220 ) ) ;
#20320 = CARTESIAN_POINT ( 'NONE',  ( -32.54531990124663565, -24.15543982623907127, -0.2315651400026567941 ) ) ;
#20321 = ORIENTED_EDGE ( 'NONE', *, *, #12141, .F. ) ;
#20322 = FACE_OUTER_BOUND ( 'NONE', #85609, .T. ) ;
#20323 = CARTESIAN_POINT ( 'NONE',  ( 15.00444628775324141, 3.502673593626820736, -27.32858455744129245 ) ) ;
#20324 = CARTESIAN_POINT ( 'NONE',  ( -117.5562042904833930, -23.48786465467241413, 11.44779295918253403 ) ) ;
#20326 = ORIENTED_EDGE ( 'NONE', *, *, #84590, .T. ) ;
#20325 = CARTESIAN_POINT ( 'NONE',  ( -17.78888362263414535, -11.56919986243916654, 11.49999999999999645 ) ) ;
#20327 = AXIS2_PLACEMENT_3D ( 'NONE', #91818, #54779, #99911 ) ;
#20328 = EDGE_CURVE ( 'NONE', #17038, #10813, #61096, .T. ) ;
#20329 = ORIENTED_EDGE ( 'NONE', *, *, #84161, .F. ) ;
#20330 = CARTESIAN_POINT ( 'NONE',  ( -21.14524153552446606, 6.695245452574716261, 11.49999999999998934 ) ) ;
#20331 = EDGE_CURVE ( 'NONE', #80380, #53265, #96713, .T. ) ;
#20332 = CARTESIAN_POINT ( 'NONE',  ( 16.39479758508079144, -12.47777281027006424, -1.500000000000002220 ) ) ;
#20333 = ORIENTED_EDGE ( 'NONE', *, *, #28592, .T. ) ;
#20334 = ORIENTED_EDGE ( 'NONE', *, *, #6926, .F. ) ;
#20335 = CARTESIAN_POINT ( 'NONE',  ( -98.52287095715006160, -29.50250243563736774, 8.947779886222138046 ) ) ;
#20336 = FACE_OUTER_BOUND ( 'NONE', #42601, .T. ) ;
#20337 = VERTEX_POINT ( 'NONE', #48430 ) ;
#20338 = ORIENTED_EDGE ( 'NONE', *, *, #33171, .F. ) ;
#20339 = ORIENTED_EDGE ( 'NONE', *, *, #24691, .T. ) ;
#20340 = PLANE ( 'NONE',  #50280 ) ;
#20341 = PLANE ( 'NONE',  #4927 ) ;
#20342 = DIRECTION ( 'NONE',  ( -0.000000000000000000, -1.000000000000000000, -0.000000000000000000 ) ) ;
#20343 = CARTESIAN_POINT ( 'NONE',  ( 17.22178217532253086, -11.58000449095910867, -1.500000000000002220 ) ) ;
#20344 = ADVANCED_FACE ( 'NONE', ( #88490 ), #79361, .T. ) ;
#20345 = CARTESIAN_POINT ( 'NONE',  ( 21.64095104908334122, -2.195182070091274529, 11.49999999999999645 ) ) ;
#20346 = ORIENTED_EDGE ( 'NONE', *, *, #77257, .F. ) ;
#20347 = CARTESIAN_POINT ( 'NONE',  ( -51.72797971311533161, -25.15689236464227463, 6.906090482414427356 ) ) ;
#20348 = CARTESIAN_POINT ( 'NONE',  ( -39.62287095715005592, -23.48786465467240347, 11.44779295918255180 ) ) ;
#20349 = CARTESIAN_POINT ( 'NONE',  ( -79.52287095715006160, -29.50250243563736774, 8.947779886222141599 ) ) ;
#20350 = CARTESIAN_POINT ( 'NONE',  ( 22.01961411883556252, 4.383451955130949429, -1.500000000000002220 ) ) ;
#20351 = CARTESIAN_POINT ( 'NONE',  ( -51.29424904866267099, -25.26334605459731364, 4.063412005954170070 ) ) ;
#20352 = CARTESIAN_POINT ( 'NONE',  ( -65.63042981099128781, -24.73486907724918282, 1.287355809206962354 ) ) ;
#20353 = EDGE_LOOP ( 'NONE', ( #66952, #8891, #66302, #27746 ) ) ;
#20354 = LINE ( 'NONE', #11754, #82503 ) ;
#20355 = FACE_OUTER_BOUND ( 'NONE', #72153, .T. ) ;
#20356 = ORIENTED_EDGE ( 'NONE', *, *, #84579, .F. ) ;
#20357 = VERTEX_POINT ( 'NONE', #57053 ) ;
#20358 = CARTESIAN_POINT ( 'NONE',  ( -87.62287095715004170, -24.64898659630528854, 1.056161002820827921 ) ) ;
#20359 = EDGE_LOOP ( 'NONE', ( #2018, #21520, #88287, #14866 ) ) ;
#20360 = VECTOR ( 'NONE', #76979, 1000.000000000000227 ) ;
#20361 = CARTESIAN_POINT ( 'NONE',  ( -19.44786352930952233, -8.617208915446557427, -1.500000000000002220 ) ) ;
#20362 = EDGE_LOOP ( 'NONE', ( #24013, #50070, #50373, #85887 ) ) ;
#20363 = CARTESIAN_POINT ( 'NONE',  ( -80.62287095715004170, -25.00182538069145721, 7.747789668545097541 ) ) ;
#20364 = AXIS2_PLACEMENT_3D ( 'NONE', #98995, #36609, #51346 ) ;
#20365 = CARTESIAN_POINT ( 'NONE',  ( 13.86046232669119149, 16.88393516940953276, 11.49999999999998934 ) ) ;
#20366 = CARTESIAN_POINT ( 'NONE',  ( -45.58953762381671737, -23.48783264082478084, -1.443836473390070374 ) ) ;
#20367 = CARTESIAN_POINT ( 'NONE',  ( 21.55457256799317278, 7.124301260279622738, 11.49999999999998934 ) ) ;
#20368 = CARTESIAN_POINT ( 'NONE',  ( -112.5228709571500616, -24.65952944569304961, 1.056160979905704123 ) ) ;
#20369 = AXIS2_PLACEMENT_3D ( 'NONE', #85683, #16163, #71471 ) ;
#20370 = CARTESIAN_POINT ( 'NONE',  ( -49.52287095715006160, -23.48786465467241769, 11.44779295918255002 ) ) ;
#20371 = CARTESIAN_POINT ( 'NONE',  ( 21.10488023177059347, -6.046698511884514460, -1.500000000000002220 ) ) ;
#20372 = CARTESIAN_POINT ( 'NONE',  ( -109.5228709571500332, -24.35013146730204525, 9.818937971375099494 ) ) ;
#20373 = ORIENTED_EDGE ( 'NONE', *, *, #65521, .F. ) ;
#20374 = CARTESIAN_POINT ( 'NONE',  ( -122.5207639614473578, -23.96169478059714564, 10.65365249895717170 ) ) ;
#20375 = CARTESIAN_POINT ( 'NONE',  ( 0.7051282051282027341, -5.876774720514409189, 19.19230769230768985 ) ) ;
#20376 = AXIS2_PLACEMENT_3D ( 'NONE', #68952, #77546, #94280 ) ;
#20377 = AXIS2_PLACEMENT_3D ( 'NONE', #41286, #35179, #59902 ) ;
#20378 = ORIENTED_EDGE ( 'NONE', *, *, #60037, .F. ) ;
#20379 = CARTESIAN_POINT ( 'NONE',  ( -90.62287095715002749, -24.63287334234179582, 0.9662140553045412972 ) ) ;
#20380 = CARTESIAN_POINT ( 'NONE',  ( -128.6228709571500417, -23.47596703998600631, 11.44779298504227860 ) ) ;
#20381 = FACE_OUTER_BOUND ( 'NONE', #64710, .T. ) ;
#20382 = CARTESIAN_POINT ( 'NONE',  ( -19.37389216307569129, 8.798533688548827669, 11.49999999999998934 ) ) ;
#20383 = CARTESIAN_POINT ( 'NONE',  ( -55.62287095715004170, -25.00182538069145011, 7.747789668545097541 ) ) ;
#20384 = CARTESIAN_POINT ( 'NONE',  ( -26.17837527425876942, -24.97064757944748337, 3.912474131936358734 ) ) ;
#20385 = CARTESIAN_POINT ( 'NONE',  ( -85.62363011676973201, -25.00158670708910691, 2.256160236439219258 ) ) ;
#20386 = CARTESIAN_POINT ( 'NONE',  ( -109.2228709571500787, -23.47596703998600631, 11.44779298504227860 ) ) ;
#20387 = ADVANCED_FACE ( 'NONE', ( #58053 ), #95096, .T. ) ;
#20388 = CARTESIAN_POINT ( 'NONE',  ( 28.87399897812681004, 1.682774720514426114, -12.57761096169975445 ) ) ;
#20389 = ORIENTED_EDGE ( 'NONE', *, *, #33412, .F. ) ;
#20390 = CARTESIAN_POINT ( 'NONE',  ( 10.86043079284791091, -16.25897383129715834, 11.49999999999999645 ) ) ;
#20391 = CARTESIAN_POINT ( 'NONE',  ( -108.5228709571500616, -24.50321055353804311, 9.387540953477509831 ) ) ;
#20392 = CARTESIAN_POINT ( 'NONE',  ( -29.80788156245805354, -25.24357952813885575, 5.313887825940373233 ) ) ;
#20393 = EDGE_LOOP ( 'NONE', ( #35947, #8112, #59579, #35551 ) ) ;
#20394 = CARTESIAN_POINT ( 'NONE',  ( 3.797776442307698286, -5.876774720514426953, 21.83974358974358410 ) ) ;
#20395 = CARTESIAN_POINT ( 'NONE',  ( -40.55620429048339304, -23.47596703998600276, 11.44779298504227505 ) ) ;
#20396 = CARTESIAN_POINT ( 'NONE',  ( -31.62287095715005236, -24.64898659630367206, 1.056161002820817485 ) ) ;
#20397 = DIRECTION ( 'NONE',  ( -3.773278334453079030E-23, 0.9999999999976377785, 2.173523156925979128E-06 ) ) ;
#20398 = CARTESIAN_POINT ( 'NONE',  ( 19.47230031930329730, 2.946587627359682493, 11.49999999999998934 ) ) ;
#20399 = ORIENTED_EDGE ( 'NONE', *, *, #8253, .F. ) ;
#20400 = LINE ( 'NONE', #89439, #60218 ) ;
#20401 = CARTESIAN_POINT ( 'NONE',  ( 2.922108196329484375, -5.876774720514417183, 20.36383711510645256 ) ) ;
#20402 = EDGE_CURVE ( 'NONE', #78762, #53932, #30289, .T. ) ;
#20403 = PERSON_AND_ORGANIZATION_ROLE ( 'classification_officer' ) ;
#20404 = EDGE_LOOP ( 'NONE', ( #9918, #85419, #61647, #72781 ) ) ;
#20405 = CARTESIAN_POINT ( 'NONE',  ( -107.5228709571500758, -24.64965694238575011, 8.947790433994192938 ) ) ;
#20406 = CARTESIAN_POINT ( 'NONE',  ( 6.044871794871792048, -6.376774720514401196, 18.16025641025640880 ) ) ;
#20407 = CARTESIAN_POINT ( 'NONE',  ( -47.54067575102843080, -24.34968618360933590, 0.1864209137778879144 ) ) ;
#20408 = CARTESIAN_POINT ( 'NONE',  ( -118.5933790690151142, -23.48783264082477018, -1.443836473390085695 ) ) ;
#20409 = CARTESIAN_POINT ( 'NONE',  ( -7.131053040288445999, -6.376774720514413630, 19.60308799987318196 ) ) ;
#20410 = ADVANCED_FACE ( 'NONE', ( #65176 ), #40134, .T. ) ;
#20411 = B_SPLINE_CURVE_WITH_KNOTS ( 'NONE', 3,
 ( #69882, #16087, #873, #15583, #77969, #16581 ),
 .UNSPECIFIED., .F., .F.,
 ( 4, 2, 4 ),
 ( 0.000000000000000000, 0.001380901958385385509, 0.002761803916770771018 ),
 .UNSPECIFIED. ) ;
#20412 = CARTESIAN_POINT ( 'NONE',  ( -69.57050707393172218, -25.24515113043987569, 5.639419424395426539 ) ) ;
#20413 = CARTESIAN_POINT ( 'NONE',  ( 5.802984775641024662, -5.876774720514403860, 18.35026041666666430 ) ) ;
#20414 = CARTESIAN_POINT ( 'NONE',  ( 19.20567810191101898, 5.375360269454119155, -1.500000000000002220 ) ) ;
#20415 = CARTESIAN_POINT ( 'NONE',  ( -32.52287095715008292, -24.33832256527048088, 0.1851278514138551823 ) ) ;
#20416 = CARTESIAN_POINT ( 'NONE',  ( -0.1188546349483167036, -21.51133334980950806, -1.019432251695407299 ) ) ;
#20417 = ORIENTED_EDGE ( 'NONE', *, *, #80491, .T. ) ;
#20418 = EDGE_CURVE ( 'NONE', #32572, #72422, #62797, .T. ) ;
#20419 = LINE ( 'NONE', #66646, #2201 ) ;
#20420 = CARTESIAN_POINT ( 'NONE',  ( 11.29837800214456855, -4.960377205085137575, -27.59811486027058436 ) ) ;
#20421 = EDGE_CURVE ( 'NONE', #58389, #36250, #5734, .T. ) ;
#20422 = AXIS2_PLACEMENT_3D ( 'NONE', #50636, #89698, #28792 ) ;
#20424 = ADVANCED_FACE ( 'NONE', ( #4252 ), #68142, .T. ) ;
#20423 =( NAMED_UNIT ( * ) PLANE_ANGLE_UNIT ( ) SI_UNIT ( $, .RADIAN. ) );
#20425 = DIRECTION ( 'NONE',  ( 0.000000000000000000, 1.000000000000000000, 0.000000000000000000 ) ) ;
#20426 = CARTESIAN_POINT ( 'NONE',  ( -124.4728709572981131, -25.30561156594276184, 5.197832205049725651 ) ) ;
#20427 = CARTESIAN_POINT ( 'NONE',  ( -81.62638369177169295, -24.51314013834316796, 0.6176544820404249458 ) ) ;
#20428 = B_SPLINE_CURVE_WITH_KNOTS ( 'NONE', 3,
 ( #31742, #25117, #63209, #79409 ),
 .UNSPECIFIED., .F., .F.,
 ( 4, 4 ),
 ( 0.7803431484189624623, 0.7893495796910778850 ),
 .UNSPECIFIED. ) ;
#20429 = FACE_OUTER_BOUND ( 'NONE', #47502, .T. ) ;
#20430 = CARTESIAN_POINT ( 'NONE',  ( -1.409217194013772101, -5.876774720514417183, 20.11414146978959749 ) ) ;
#20431 = AXIS2_PLACEMENT_3D ( 'NONE', #3992, #5975, #90717 ) ;
#20432 = ORIENTED_EDGE ( 'NONE', *, *, #46057, .T. ) ;
#20433 = CARTESIAN_POINT ( 'NONE',  ( 10.34999999999999432, 12.00000000000002309, 2.100000000000000089 ) ) ;
#20435 = VECTOR ( 'NONE', #27843, 1000.000000000000000 ) ;
#20434 = CARTESIAN_POINT ( 'NONE',  ( 30.53060340732035982, 4.132774720517318201, 19.84760796525321780 ) ) ;
#20436 = ORIENTED_EDGE ( 'NONE', *, *, #97893, .F. ) ;
#20437 = VECTOR ( 'NONE', #55440, 1000.000000000000000 ) ;
#20438 = CARTESIAN_POINT ( 'NONE',  ( 18.19722386731275066, -8.884848157732822216, 11.49999999999998934 ) ) ;
#20439 = EDGE_CURVE ( 'NONE', #36659, #21242, #93580, .T. ) ;
#20440 = CARTESIAN_POINT ( 'NONE',  ( -105.5228709571500616, -24.99156044556202971, 7.747789690856173195 ) ) ;
#20441 = VECTOR ( 'NONE', #82686, 1000.000000000000114 ) ;
#20442 = CARTESIAN_POINT ( 'NONE',  ( -43.62287095715004881, -24.64898659630367206, 1.056161002820819261 ) ) ;
#20443 = B_SPLINE_CURVE_WITH_KNOTS ( 'NONE', 3,
 ( #99161, #51514, #29659, #74831, #61126, #22525 ),
 .UNSPECIFIED., .F., .F.,
 ( 4, 2, 4 ),
 ( 6.384118678613478637E-06, 0.001386860460828377587, 0.002767336802978141459 ),
 .UNSPECIFIED. ) ;
#20444 = AXIS2_PLACEMENT_3D ( 'NONE', #46409, #31175, #23047 ) ;
#20445 = CARTESIAN_POINT ( 'NONE',  ( -76.62287095715007013, -24.51283580621364422, 0.6167428607019831421 ) ) ;
#20446 = VERTEX_POINT ( 'NONE', #50427 ) ;
#20447 = CARTESIAN_POINT ( 'NONE',  ( -79.89320743519122914, -25.31550070763928773, 5.063404179320856180 ) ) ;
#20448 = DIRECTION ( 'NONE',  ( -1.000000000000000000, 0.000000000000000000, 0.000000000000000000 ) ) ;
#20449 = CARTESIAN_POINT ( 'NONE',  ( 15.84714387567644955, -12.28532832577633194, -1.500000000000002220 ) ) ;
#20450 = CARTESIAN_POINT ( 'NONE',  ( 17.02745815656931683, -12.38318283856952107, 11.49999999999999645 ) ) ;
#20451 = LINE ( 'NONE', #89480, #8051 ) ;
#20452 = CARTESIAN_POINT ( 'NONE',  ( -111.6228709571500559, -23.72773821059536559, 11.05748984161097326 ) ) ;
#20453 = CARTESIAN_POINT ( 'NONE',  ( -21.12782282263547984, 6.412464199276892707, 11.49999999999998934 ) ) ;
#20454 = EDGE_CURVE ( 'NONE', #25992, #23706, #89481, .T. ) ;
#20455 = CARTESIAN_POINT ( 'NONE',  ( -96.52287095715004739, -24.33832256527049154, 0.1851278514138652020 ) ) ;
#20456 = CARTESIAN_POINT ( 'NONE',  ( -47.62287095715005592, -24.33832256527047733, 0.1851278514138583187 ) ) ;
#20457 = CARTESIAN_POINT ( 'NONE',  ( -50.20044999871004165, -25.27344762162802994, 3.305837191087945381 ) ) ;
#20458 = ORIENTED_EDGE ( 'NONE', *, *, #79093, .F. ) ;
#20459 = EDGE_CURVE ( 'NONE', #5012, #24383, #65131, .T. ) ;
#20460 = LINE ( 'NONE', #90483, #26776 ) ;
#20461 = CARTESIAN_POINT ( 'NONE',  ( -31.65921402591105505, -23.73766607897669800, -1.055555164236445131 ) ) ;
#20462 = ORIENTED_EDGE ( 'NONE', *, *, #14668, .T. ) ;
#20463 = ORIENTED_EDGE ( 'NONE', *, *, #98132, .F. ) ;
#20464 = CARTESIAN_POINT ( 'NONE',  ( -41.52287095715006870, -23.48786465467240347, 11.44779295918255180 ) ) ;
#20465 = CARTESIAN_POINT ( 'NONE',  ( 6.044871794871792048, -6.376774720514401196, 18.16025641025640880 ) ) ;
#20466 = CARTESIAN_POINT ( 'NONE',  ( 8.071512145086499501, -1.000000000000008882, 3.746884140868834923 ) ) ;
#20467 = CARTESIAN_POINT ( 'NONE',  ( -11.86786554430972096, -16.85652113839894639, -1.500000000000002220 ) ) ;
#20468 = EDGE_CURVE ( 'NONE', #55380, #88518, #16645, .T. ) ;
#20469 = CARTESIAN_POINT ( 'NONE',  ( -20.99440926880444636, 4.982473936180791263, 11.49999999999999645 ) ) ;
#20470 = ORIENTED_EDGE ( 'NONE', *, *, #71999, .F. ) ;
#20471 = CARTESIAN_POINT ( 'NONE',  ( -49.86436991692592358, -25.15008860783680333, 7.002718424707902400 ) ) ;
#20472 = CARTESIAN_POINT ( 'NONE',  ( -105.6228709571500559, -23.47596703998600631, 11.44779298504227860 ) ) ;
#20473 = VECTOR ( 'NONE', #96044, 1000.000000000000114 ) ;
#20474 = DIRECTION ( 'NONE',  ( 0.000000000000000000, -1.000000000000000000, 0.000000000000000000 ) ) ;
#20475 = CARTESIAN_POINT ( 'NONE',  ( 22.34790896907852442, -0.4833156648990815651, 11.49999999999998934 ) ) ;
#20476 = EDGE_CURVE ( 'NONE', #24634, #81045, #14831, .T. ) ;
#20477 = CARTESIAN_POINT ( 'NONE',  ( -100.4426124108961176, -25.13313949306887451, 7.101635536975466678 ) ) ;
#20478 = CARTESIAN_POINT ( 'NONE',  ( 7.160000000000000142, -6.754662360505034435, 7.925641719537454222 ) ) ;
#20479 = EDGE_LOOP ( 'NONE', ( #21722, #40701, #20188, #70244 ) ) ;
#20480 = EDGE_CURVE ( 'NONE', #5271, #20866, #79655, .T. ) ;
#20481 = DIRECTION ( 'NONE',  ( 0.000000000000000000, 0.000000000000000000, -1.000000000000000000 ) ) ;
#20482 = CARTESIAN_POINT ( 'NONE',  ( 3.296548071537245495, -5.876774720514426065, 21.29143507544719682 ) ) ;
#20483 = CARTESIAN_POINT ( 'NONE',  ( 14.99592430652175956, 14.54719766626331889, 11.49999999999998934 ) ) ;
#20484 = ORIENTED_EDGE ( 'NONE', *, *, #20727, .T. ) ;
#20486 = ORIENTED_EDGE ( 'NONE', *, *, #86723, .F. ) ;
#20485 = CARTESIAN_POINT ( 'NONE',  ( -90.62287095715004170, -29.50249982740957577, 7.747779886224967605 ) ) ;
#20487 = VERTEX_POINT ( 'NONE', #41077 ) ;
#20488 = CARTESIAN_POINT ( 'NONE',  ( -51.29687923781917647, -25.26364009307625125, 3.993462176398971497 ) ) ;
#20489 = CARTESIAN_POINT ( 'NONE',  ( -15.55823947972799282, -14.28038451723262270, -1.500000000000002220 ) ) ;
#20490 = EDGE_LOOP ( 'NONE', ( #2413, #71673, #57730, #84408, #89612, #11776, #40595, #96022, #5634, #15227, #24813, #7012, #76851, #62443, #27991, #64727, #99740, #44982, #90818, #32072, #24633, #21724, #57801, #78598, #85526, #86689, #10018, #94199, #32882, #34266, #44697, #76486, #28074, #30508, #28330, #79393, #42077, #33827, #95917, #62756, #84768, #81809, #69292, #31965, #98704, #4181, #80121, #22968, #12152, #4604, #90735, #73260, #55842, #36225, #43278, #15828, #50968, #48616, #23199, #22468, #72409, #15719, #42537, #2178, #60718, #39440, #95360, #87129, #37073, #35811, #62699, #47090, #15870, #30720, #57817, #55931, #8846, #37482, #52331, #53986, #60962, #9908, #10511, #52055, #26876, #75203, #92337, #18733, #90533, #54837, #74773, #751, #3417, #29234, #89618, #79266, #69761, #42560, #58477, #96710, #5035, #26940, #78086, #73221, #20596, #15841, #16756, #50997, #64907, #4962, #39573, #32118, #76634, #67415, #98027, #56956, #88065, #36440, #78962, #50964, #99906, #18477, #72074, #31204, #26565, #1103, #52211, #4771, #22080, #43207, #83971, #27696, #9491, #53507, #53701, #96761, #56059, #75465, #64321, #42615, #5466, #12489, #6627, #66549, #55203, #6257, #4892, #33376, #83610, #80647, #44862, #11860, #45873, #52934, #83540, #17732, #35757, #68961, #10893, #53721, #87754, #61294, #28285, #26003, #61808, #78829, #50336, #55427, #48495, #31442, #85396, #19724, #42494, #13089, #37570, #5068, #25707, #29122, #37964, #50900, #71175, #35969, #62832, #76392, #85358, #53081, #18031, #25013, #59410, #83224, #31239, #80202, #6122, #92017, #71984, #83535, #8152, #87281, #58434, #81121, #3332, #33196 ) ) ;
#20491 = CARTESIAN_POINT ( 'NONE',  ( -128.5228709571500758, -24.65952944569305316, 1.056160979905707675 ) ) ;
#20492 = CARTESIAN_POINT ( 'NONE',  ( -22.05275734969026047, 5.965225279485572685, 31.02402280011862246 ) ) ;
#20493 = FACE_OUTER_BOUND ( 'NONE', #14222, .T. ) ;
#20494 = DIRECTION ( 'NONE',  ( 0.000000000000000000, -0.000000000000000000, -1.000000000000000000 ) ) ;
#20495 = PLANE ( 'NONE',  #31937 ) ;
#20496 = CARTESIAN_POINT ( 'NONE',  ( -21.72135255055207281, 0.4632500610043824851, -1.500000000000002220 ) ) ;
#20497 = CARTESIAN_POINT ( 'NONE',  ( -81.22562555205841761, -25.12224328816577312, 6.810745100948484065 ) ) ;
#20499 = ORIENTED_EDGE ( 'NONE', *, *, #96962, .T. ) ;
#20498 = CARTESIAN_POINT ( 'NONE',  ( -11.77839732991513166, 18.97803183815481987, 11.49999999999999645 ) ) ;
#20500 = CARTESIAN_POINT ( 'NONE',  ( -42.52287095715004739, -23.48783264083366973, -1.443836473376261642 ) ) ;
#20501 = CARTESIAN_POINT ( 'NONE',  ( 7.166666666666668739, -6.376774720514414518, 20.78665865384614975 ) ) ;
#20502 = CARTESIAN_POINT ( 'NONE',  ( -106.5228709571500900, -23.72773821059536914, 11.05748984161097326 ) ) ;
#20503 = VERTEX_POINT ( 'NONE', #33451 ) ;
#20504 = VECTOR ( 'NONE', #43647, 1000.000000000000000 ) ;
#20505 = EDGE_LOOP ( 'NONE', ( #78358, #1161, #82292, #1788 ) ) ;
#20506 = ORIENTED_EDGE ( 'NONE', *, *, #56400, .F. ) ;
#20507 = CARTESIAN_POINT ( 'NONE',  ( -100.5101156622768031, -25.13331755552596647, 7.100618926951157484 ) ) ;
#20508 = DIRECTION ( 'NONE',  ( -2.352173255807804438E-16, 2.352173255807796056E-16, 1.000000000000000000 ) ) ;
#20509 = CARTESIAN_POINT ( 'NONE',  ( 30.61138385796263606, -5.156104205939422869, 27.19700247792284031 ) ) ;
#20510 = CARTESIAN_POINT ( 'NONE',  ( -67.52287095715006160, -23.47596703998600631, 11.44779298504228748 ) ) ;
#20511 = AXIS2_PLACEMENT_3D ( 'NONE', #58411, #95452, #74608 ) ;
#20512 = CARTESIAN_POINT ( 'NONE',  ( 31.33322533232960083, 4.132774720514427180, -3.827970713771306155 ) ) ;
#20513 = CARTESIAN_POINT ( 'NONE',  ( -31.52287095715006160, -23.48786465467240347, 11.44779295918255357 ) ) ;
#20514 = VERTEX_POINT ( 'NONE', #45798 ) ;
#20515 = VECTOR ( 'NONE', #18987, 1000.000000000000000 ) ;
#20516 = CARTESIAN_POINT ( 'NONE',  ( -4.359330469889163950, 18.88329184224734192, 11.49999999999999645 ) ) ;
#20517 = CARTESIAN_POINT ( 'NONE',  ( -81.58953762381673869, -23.47596703998600276, 11.44779298504227683 ) ) ;
#20518 = VECTOR ( 'NONE', #5775, 1000.000000000000000 ) ;
#20519 = ORIENTED_EDGE ( 'NONE', *, *, #91117, .F. ) ;
#20520 = CARTESIAN_POINT ( 'NONE',  ( 6.573941812937369455, 0.2639660507643281639, 9.334907998774166978E-16 ) ) ;
#20521 = CARTESIAN_POINT ( 'NONE',  ( 8.476323908354110870, 5.356774720514068555, -27.09030197689322961 ) ) ;
#20522 = CARTESIAN_POINT ( 'NONE',  ( -122.5228709571500616, -23.48786465467241769, 11.44779295918253759 ) ) ;
#20523 = AXIS2_PLACEMENT_3D ( 'NONE', #49169, #58271, #96321 ) ;
#20524 = CARTESIAN_POINT ( 'NONE',  ( -36.52287095715006870, -23.73934037231755667, 11.05740245334329153 ) ) ;
#20525 = CARTESIAN_POINT ( 'NONE',  ( 14.99095386781537975, 12.61000069877385421, 11.49999999999998934 ) ) ;
#20526 = LINE ( 'NONE', #82432, #15329 ) ;
#20527 = EDGE_LOOP ( 'NONE', ( #4263, #2428 ) ) ;
#20528 = CARTESIAN_POINT ( 'NONE',  ( 19.31049906410359895, -9.575588319827552652, -1.500000000000002220 ) ) ;
#20529 = CARTESIAN_POINT ( 'NONE',  ( -56.55620429048340014, -24.64898659630528499, 1.056161002820820594 ) ) ;
#20530 = CARTESIAN_POINT ( 'NONE',  ( -70.61198345729647485, -25.25639593825978579, 7.066381960558362429 ) ) ;
#20532 = B_SPLINE_CURVE_WITH_KNOTS ( 'NONE', 3,
 ( #91072, #22047, #36797, #29173 ),
 .UNSPECIFIED., .F., .F.,
 ( 4, 4 ),
 ( 0.000000000000000000, 0.0001000000000000028644 ),
 .UNSPECIFIED. ) ;
#20531 = LINE ( 'NONE', #5316, #3872 ) ;
#20533 = CARTESIAN_POINT ( 'NONE',  ( -99.72418814851606328, -25.27473278399916623, 3.555267675504576008 ) ) ;
#20534 = CARTESIAN_POINT ( 'NONE',  ( -19.06187107478486098, -12.82570580458313003, -1.500000000000002220 ) ) ;
#20535 = EDGE_CURVE ( 'NONE', #79071, #100041, #38168, .T. ) ;
#20536 = APPROVAL_ROLE ( '' ) ;
#20537 = CARTESIAN_POINT ( 'NONE',  ( -101.3738023147422780, -25.27307239909452008, 3.986250617436227550 ) ) ;
#20538 = LINE ( 'NONE', #22025, #32878 ) ;
#20539 = CARTESIAN_POINT ( 'NONE',  ( -6.497366621441947210, -19.08602653180391329, 11.49999999999999645 ) ) ;
#20540 = CARTESIAN_POINT ( 'NONE',  ( 19.75748517575715368, -0.3587747205144265483, 28.87153971905864580 ) ) ;
#20541 = LINE ( 'NONE', #35788, #92243 ) ;
#20542 = CARTESIAN_POINT ( 'NONE',  ( 12.16765770914787304, -6.475225279485573360, -27.57618308014988173 ) ) ;
#20543 = CARTESIAN_POINT ( 'NONE',  ( 8.000000000000003553, -6.376774720514426953, 22.50000000000000355 ) ) ;
#20544 = DIRECTION ( 'NONE',  ( -0.000000000000000000, -1.000000000000000000, -0.000000000000000000 ) ) ;
#20545 = CARTESIAN_POINT ( 'NONE',  ( 3.337697395173636394, -19.57427954046807983, 11.49999999999998934 ) ) ;
#20547 = EDGE_CURVE ( 'NONE', #52686, #31493, #63939, .T. ) ;
#20546 = CARTESIAN_POINT ( 'NONE',  ( -47.58953762381672448, -24.66019654487199020, 8.947790411086131712 ) ) ;
#20548 = CARTESIAN_POINT ( 'NONE',  ( 19.26447527235507451, 4.322997736827044690, -1.500000000000002220 ) ) ;
#20549 = VECTOR ( 'NONE', #95496, 1000.000000000000114 ) ;
#20550 = EDGE_CURVE ( 'NONE', #1418, #23841, #75943, .T. ) ;
#20551 = CARTESIAN_POINT ( 'NONE',  ( -126.5555559438642490, -24.15620529776629155, 10.23563542870658871 ) ) ;
#20552 = EDGE_CURVE ( 'NONE', #21243, #48074, #38486, .T. ) ;
#20553 = B_SPLINE_CURVE_WITH_KNOTS ( 'NONE', 3,
 ( #69332, #62745, #30770, #55120 ),
 .UNSPECIFIED., .F., .F.,
 ( 4, 4 ),
 ( 0.000000000000000000, 0.0001000000000000028644 ),
 .UNSPECIFIED. ) ;
#20555 = EDGE_CURVE ( 'NONE', #53154, #57700, #94212, .T. ) ;
#20554 = UNCERTAINTY_MEASURE_WITH_UNIT (LENGTH_MEASURE( 1.000000000000000082E-05 ), #50131, 'distance_accuracy_value', 'NONE');
#20556 = CARTESIAN_POINT ( 'NONE',  ( -0.5315124411682757843, -6.376774720514411854, 19.46509473978807847 ) ) ;
#20557 = CARTESIAN_POINT ( 'NONE',  ( 22.81105451610979173, -500000.0000000000582, -18.46691820600746681 ) ) ;
#20558 = CARTESIAN_POINT ( 'NONE',  ( 13.32396043830641830, 15.83023408377254704, 11.49999999999999645 ) ) ;
#20559 = VECTOR ( 'NONE', #15387, 999.9999999999998863 ) ;
#20560 = DIRECTION ( 'NONE',  ( -3.773278334453079618E-23, 0.9999999999976377785, 2.173523156925979975E-06 ) ) ;
#20561 = CARTESIAN_POINT ( 'NONE',  ( 31.60906425211781823, 3.844812497472038793, -2.545713913898462799 ) ) ;
#20562 = CARTESIAN_POINT ( 'NONE',  ( -14.80616194778269623, -17.16973004002414882, 11.49999999999999645 ) ) ;
#20563 = VERTEX_POINT ( 'NONE', #92454 ) ;
#20564 = CARTESIAN_POINT ( 'NONE',  ( -1.044792363895550302, -5.876774720514417183, 20.41272575174754422 ) ) ;
#20565 = CARTESIAN_POINT ( 'NONE',  ( 30.61752088227329693, 5.013017886559611114, 27.44065105897852419 ) ) ;
#20566 = EDGE_CURVE ( 'NONE', #88518, #18541, #21603, .T. ) ;
#20567 = CARTESIAN_POINT ( 'NONE',  ( -63.63676973242693435, -24.15543982623906771, -0.2315651400026651485 ) ) ;
#20568 = CARTESIAN_POINT ( 'NONE',  ( -10.54059822343757880, -5.876774720514426953, 22.82308057603841078 ) ) ;
#20569 = VERTEX_POINT ( 'NONE', #2518 ) ;
#20570 = AXIS2_PLACEMENT_3D ( 'NONE', #23876, #55859, #86785 ) ;
#20571 = ORIENTED_EDGE ( 'NONE', *, *, #64121, .F. ) ;
#20572 = EDGE_CURVE ( 'NONE', #4586, #47607, #99558, .T. ) ;
#20573 = DIRECTION ( 'NONE',  ( 0.000000000000000000, 0.9999999999976377785, 2.173523156925979128E-06 ) ) ;
#20574 = CARTESIAN_POINT ( 'NONE',  ( -22.23020047961643186, 5.420056861400933457, -1.500000000000002220 ) ) ;
#20575 = CARTESIAN_POINT ( 'NONE',  ( -29.59428796461985911, -24.07610702673311209, -0.2315648265717072385 ) ) ;
#20576 = CARTESIAN_POINT ( 'NONE',  ( 20.98369277809155165, -4.918611649023987731, -1.500000000000002220 ) ) ;
#20577 = CARTESIAN_POINT ( 'NONE',  ( -113.5569086508091488, -23.73791477778911840, 11.05961554403170233 ) ) ;
#20578 = CARTESIAN_POINT ( 'NONE',  ( -115.5895376238167245, -24.99156044556120904, 7.747789690856344613 ) ) ;
#20579 = CARTESIAN_POINT ( 'NONE',  ( 6.619388286264371146, -21.57091762011834390, 11.49999999999999645 ) ) ;
#20580 = VERTEX_POINT ( 'NONE', #30060 ) ;
#20581 = CARTESIAN_POINT ( 'NONE',  ( -4.568292318365942073, -5.965225279485572685, 30.06720597538392425 ) ) ;
#20582 = CARTESIAN_POINT ( 'NONE',  ( 14.26656746985186608, 16.74056184347216458, -1.500000000000002220 ) ) ;
#20583 = EDGE_CURVE ( 'NONE', #56064, #67264, #11914, .T. ) ;
#20584 = AXIS2_PLACEMENT_3D ( 'NONE', #45177, #98434, #37553 ) ;
#20585 = CARTESIAN_POINT ( 'NONE',  ( -111.5879375875708917, -24.51314013834316796, 0.6176544820404210601 ) ) ;
#20586 = CARTESIAN_POINT ( 'NONE',  ( -28.45645220296530908, -25.21724939687763367, 7.353599707584590917 ) ) ;
#20587 = VERTEX_POINT ( 'NONE', #32455 ) ;
#20588 = DIRECTION ( 'NONE',  ( 0.000000000000000000, 0.000000000000000000, 1.000000000000000000 ) ) ;
#20589 = CARTESIAN_POINT ( 'NONE',  ( -90.58192276783553609, -25.00182538069147142, 7.747789668545044250 ) ) ;
#20590 = EDGE_LOOP ( 'NONE', ( #72998, #91486, #91084, #77620 ) ) ;
#20591 = VECTOR ( 'NONE', #89524, 1000.000000000000000 ) ;
#20592 = CARTESIAN_POINT ( 'NONE',  ( 10.86264265030973952, 5.965225279485574461, -28.64597719988137570 ) ) ;
#20593 = ORIENTED_EDGE ( 'NONE', *, *, #65273, .T. ) ;
#20594 = AXIS2_PLACEMENT_3D ( 'NONE', #36111, #67080, #44232 ) ;
#20595 = B_SPLINE_CURVE_WITH_KNOTS ( 'NONE', 3,
 ( #32213, #78380, #39830, #16989, #94112, #24598 ),
 .UNSPECIFIED., .F., .F.,
 ( 4, 2, 4 ),
 ( 0.000000000000000000, 0.001380764517854769086, 0.002761529035709538171 ),
 .UNSPECIFIED. ) ;
#20596 = ORIENTED_EDGE ( 'NONE', *, *, #13147, .F. ) ;
#20597 = CARTESIAN_POINT ( 'NONE',  ( -61.52287095715006160, -29.50250786944525672, 11.44777988621623876 ) ) ;
#20598 = CARTESIAN_POINT ( 'NONE',  ( -8.160000000000000142, 0.000000000000000000, 2.399999999999999911 ) ) ;
#20599 = CARTESIAN_POINT ( 'NONE',  ( -102.6228709571500559, -23.47593901973091235, -1.443836447539001089 ) ) ;
#20600 = CARTESIAN_POINT ( 'NONE',  ( 9.511415417357532931, -18.05363124325620205, -1.500000000000002220 ) ) ;
#20601 = ORIENTED_EDGE ( 'NONE', *, *, #47186, .F. ) ;
#20602 = CARTESIAN_POINT ( 'NONE',  ( -2.806649551956928335, -5.876774720514410966, 19.35116211686183618 ) ) ;
#20603 = CARTESIAN_POINT ( 'NONE',  ( -99.52287095715000476, -23.73934037231757443, 11.05740245334328442 ) ) ;
#20604 = EDGE_CURVE ( 'NONE', #73483, #26090, #10116, .T. ) ;
#20605 = CARTESIAN_POINT ( 'NONE',  ( -105.5081720153104357, -24.92564183028979130, 1.928384488918251316 ) ) ;
#20606 = CARTESIAN_POINT ( 'NONE',  ( -70.40598983096596442, -25.25855381519730258, 7.561208889967863556 ) ) ;
#20607 = ORIENTED_EDGE ( 'NONE', *, *, #9217, .T. ) ;
#20608 = CARTESIAN_POINT ( 'NONE',  ( -10.34999999999999254, 2.573529411764704733, 1.544117647058823151 ) ) ;
#20609 = CARTESIAN_POINT ( 'NONE',  ( 6.431189903846153300, -6.376774720514415407, 20.08974358974358765 ) ) ;
#20610 = ORIENTED_EDGE ( 'NONE', *, *, #71317, .F. ) ;
#20611 = CARTESIAN_POINT ( 'NONE',  ( -6.767879454864726974, -19.68250801024624508, -1.500000000000002220 ) ) ;
#20612 = EDGE_CURVE ( 'NONE', #9578, #36415, #53917, .T. ) ;
#20613 = ORIENTED_EDGE ( 'NONE', *, *, #11203, .F. ) ;
#20615 = ORIENTED_EDGE ( 'NONE', *, *, #83229, .F. ) ;
#20614 = PLANE ( 'NONE',  #47467 ) ;
#20616 = CARTESIAN_POINT ( 'NONE',  ( -91.94687923781918926, -25.23397913219354649, 6.409327625488847602 ) ) ;
#20617 = CARTESIAN_POINT ( 'NONE',  ( -56.58953762381675290, -23.47596703998600276, 11.44779298504227505 ) ) ;
#20618 = ORIENTED_EDGE ( 'NONE', *, *, #13552, .T. ) ;
#20619 = ORIENTED_EDGE ( 'NONE', *, *, #92745, .T. ) ;
#20620 = CARTESIAN_POINT ( 'NONE',  ( -33.52287095715008292, -24.33927499327854349, 9.819080762295817166 ) ) ;
#20621 =( BOUNDED_SURFACE ( )  B_SPLINE_SURFACE ( 3, 2, ( 
 ( #81421, #13385, #12887 ),
 ( #66221, #97140, #97631 ),
 ( #44365, #49990, #43367 ),
 ( #67707, #90521, #27137 ) ),
 .UNSPECIFIED., .F., .F., .T. ) 
 B_SPLINE_SURFACE_WITH_KNOTS ( ( 4, 4 ),
 ( 3, 3 ),
 ( 0.004439845973569162343, 0.004703938444645663561 ),
 ( 0.000000000000000000, 1.000000000000000000 ),
 .UNSPECIFIED. ) 
 GEOMETRIC_REPRESENTATION_ITEM ( )  RATIONAL_B_SPLINE_SURFACE ( (
 ( 1.000000000000000000, 0.9005394799515968884, 1.000000000000000000),
 ( 1.000000000000000000, 0.9005352985759397244, 1.000000000000000000),
 ( 1.000000000000000000, 0.8990570573199264670, 1.000000000000000000),
 ( 1.000000000000000000, 0.8962098481621324497, 1.000000000000000000) ) ) 
 REPRESENTATION_ITEM ( '' )  SURFACE ( )  );
#20622 = CARTESIAN_POINT ( 'NONE',  ( -119.4336594584714391, -25.30053190447140921, 4.607786779764230012 ) ) ;
#20623 = CARTESIAN_POINT ( 'NONE',  ( -52.62287095715006302, -24.35013146730203815, 9.818937971375113705 ) ) ;
#20624 = CARTESIAN_POINT ( 'NONE',  ( -71.04293837957820301, -25.31201647013682887, 5.573254820805182419 ) ) ;
#20626 = ORIENTED_EDGE ( 'NONE', *, *, #97578, .T. ) ;
#20625 = CARTESIAN_POINT ( 'NONE',  ( 13.35222405703702186, 17.66689192352044913, 11.49999999999999645 ) ) ;
#20627 = CARTESIAN_POINT ( 'NONE',  ( -108.6278311533503143, -24.15543982623907837, -0.2315651400026445539 ) ) ;
#20628 = CARTESIAN_POINT ( 'NONE',  ( -11.86362535333686807, -19.25999739251378173, -1.500000000000002220 ) ) ;
#20629 = AXIS2_PLACEMENT_3D ( 'NONE', #12262, #27513, #43241 ) ;
#20631 = ORIENTED_EDGE ( 'NONE', *, *, #25606, .F. ) ;
#20630 = CARTESIAN_POINT ( 'NONE',  ( -115.5183015014103916, -24.15602025860897584, 10.28564288303533836 ) ) ;
#20632 = B_SPLINE_CURVE_WITH_KNOTS ( 'NONE', 3,
 ( #18776, #64993, #79178, #86791, #88306, #65492 ),
 .UNSPECIFIED., .F., .F.,
 ( 4, 2, 4 ),
 ( 0.000000000000000000, 0.001380764517854764098, 0.002761529035709528197 ),
 .UNSPECIFIED. ) ;
#20633 = ORIENTED_EDGE ( 'NONE', *, *, #53140, .T. ) ;
#20634 = AXIS2_PLACEMENT_3D ( 'NONE', #93649, #8425, #6925 ) ;
#20635 = CARTESIAN_POINT ( 'NONE',  ( -127.6228709571500559, -23.48783264082479505, -1.443836473390056829 ) ) ;
#20636 = CARTESIAN_POINT ( 'NONE',  ( -89.40841769935769889, -25.23397913219577049, 6.409327625469732226 ) ) ;
#20637 = VERTEX_POINT ( 'NONE', #9115 ) ;
#20638 = CARTESIAN_POINT ( 'NONE',  ( -126.5228709571499763, -23.48783264082477018, -1.443836473390082142 ) ) ;
#20639 = CARTESIAN_POINT ( 'NONE',  ( 7.190675130926929448, -21.12231643677837312, -1.500000000000002220 ) ) ;
#20640 = FACE_OUTER_BOUND ( 'NONE', #26721, .T. ) ;
#20641 = VERTEX_POINT ( 'NONE', #78607 ) ;
#20642 = CARTESIAN_POINT ( 'NONE',  ( -115.5228709571500616, -29.50249982740957577, 7.747779886224967605 ) ) ;
#20643 = FACE_OUTER_BOUND ( 'NONE', #90300, .T. ) ;
#20644 = CARTESIAN_POINT ( 'NONE',  ( -27.70544111104076990, -24.60484793945295934, 1.628749883096155981 ) ) ;
#20645 = VECTOR ( 'NONE', #69825, 1000.000000000000000 ) ;
#20646 = CARTESIAN_POINT ( 'NONE',  ( -49.62287095715007013, -24.33927499327854704, 9.819080762295820719 ) ) ;
#20647 = CARTESIAN_POINT ( 'NONE',  ( 13.99288689683290166, -5.965225279485572685, -28.28242551218217926 ) ) ;
#20648 = CARTESIAN_POINT ( 'NONE',  ( -13.24781383850973349, 14.34467480260970795, 11.49999999999998934 ) ) ;
#20649 = CARTESIAN_POINT ( 'NONE',  ( -20.86232423683148340, -5.086641213604358391, 11.49999999999998934 ) ) ;
#20650 = CARTESIAN_POINT ( 'NONE',  ( -27.12458168156152638, -24.92774685199402285, 1.715462320597556323 ) ) ;
#20651 = CARTESIAN_POINT ( 'NONE',  ( -83.62287095715005592, -23.47593901973091235, -1.443836447539004642 ) ) ;
#20652 = CARTESIAN_POINT ( 'NONE',  ( -120.5562042904833930, -24.99156044556202616, 7.747789690856173195 ) ) ;
#20653 = CARTESIAN_POINT ( 'NONE',  ( -2.521034868938843765, 22.70145277337256218, -1.500000000000002220 ) ) ;
#20654 = VECTOR ( 'NONE', #53191, 1000.000000000000114 ) ;
#20655 = PERSON_AND_ORGANIZATION_ROLE ( 'creator' ) ;
#20656 = DIRECTION ( 'NONE',  ( 0.000000000000000000, 0.000000000000000000, -1.000000000000000000 ) ) ;
#20657 = CARTESIAN_POINT ( 'NONE',  ( 8.071512145086501278, -1.000000000000008882, -3.746884140868835367 ) ) ;
#20658 = CARTESIAN_POINT ( 'NONE',  ( 19.86680303116296287, 2.261939200664708327, 11.49999999999999645 ) ) ;
#20659 = CARTESIAN_POINT ( 'NONE',  ( 4.712727796232553779, 3.316774720514426456, -25.55789472434992859 ) ) ;
#20660 = EDGE_CURVE ( 'NONE', #36444, #49834, #63431, .T. ) ;
#20661 = AXIS2_PLACEMENT_3D ( 'NONE', #77036, #36989, #69441 ) ;
#20662 = ADVANCED_FACE ( 'NONE', ( #9617 ), #2021, .T. ) ;
#20663 = CARTESIAN_POINT ( 'NONE',  ( -39.56974522548517825, -23.48786465467240347, 11.44779295918255002 ) ) ;
#20664 = CARTESIAN_POINT ( 'NONE',  ( -101.6228709571500559, -24.50216790748099882, 0.6166512839513650368 ) ) ;
#20665 = VERTEX_POINT ( 'NONE', #48701 ) ;
#20666 = FACE_OUTER_BOUND ( 'NONE', #91022, .T. ) ;
#20667 = LINE ( 'NONE', #21165, #68519 ) ;
#20668 = EDGE_CURVE ( 'NONE', #18228, #74261, #96855, .T. ) ;
#20669 = CARTESIAN_POINT ( 'NONE',  ( 21.03555826204448209, -5.341079136732027166, -1.500000000000002220 ) ) ;
#20670 = DIRECTION ( 'NONE',  ( -0.000000000000000000, 0.000000000000000000, -1.000000000000000000 ) ) ;
#20671 = CARTESIAN_POINT ( 'NONE',  ( 9.052818235119415746, 17.31195010612007223, -1.500000000000002220 ) ) ;
#20672 = EDGE_CURVE ( 'NONE', #83541, #99862, #51811, .T. ) ;
#20673 = CARTESIAN_POINT ( 'NONE',  ( -128.6228709571500417, -29.50247984919015209, -1.443849546365044922 ) ) ;
#20674 = VERTEX_POINT ( 'NONE', #73032 ) ;
#20675 = CALENDAR_DATE ( 2026, 9, 10 ) ;
#20676 = CARTESIAN_POINT ( 'NONE',  ( -47.52287095715006160, -29.50250243563736774, 8.947779886222146928 ) ) ;
#20677 = CARTESIAN_POINT ( 'NONE',  ( 6.573941812937369455, -7.905506363763796338E-18, 0.2639660507643297183 ) ) ;
#20678 = CARTESIAN_POINT ( 'NONE',  ( -19.72667040167412722, -5.651925516699977337, 11.49999999999999645 ) ) ;
#20679 = CARTESIAN_POINT ( 'NONE',  ( -49.31826291143544694, -25.27387648715609458, 5.882378102033829492 ) ) ;
#20680 = CARTESIAN_POINT ( 'NONE',  ( -113.5895376238167245, -24.66019654487199730, 8.947790411086124607 ) ) ;
#20681 = ADVANCED_FACE ( 'NONE', ( #27348 ), #11610, .T. ) ;
#20682 = EDGE_LOOP ( 'NONE', ( #94008, #80211, #93881, #14021 ) ) ;
#20683 = LINE ( 'NONE', #52644, #96201 ) ;
#20684 = CARTESIAN_POINT ( 'NONE',  ( -43.58953762381672448, -24.66019654487199375, 8.947790411086137041 ) ) ;
#20685 = CARTESIAN_POINT ( 'NONE',  ( -78.62287095715008434, -24.50216790748098816, 0.6166512839513725863 ) ) ;
#20686 = CARTESIAN_POINT ( 'NONE',  ( -61.62287095715004881, -23.47593901973091235, -1.443836447539007972 ) ) ;
#20687 = ORIENTED_EDGE ( 'NONE', *, *, #36706, .T. ) ;
#20688 = FACE_OUTER_BOUND ( 'NONE', #48339, .T. ) ;
#20689 = AXIS2_PLACEMENT_3D ( 'NONE', #70804, #26122, #18008 ) ;
#20690 = CARTESIAN_POINT ( 'NONE',  ( -18.50152239663938403, 13.63810111590111163, 11.49999999999999645 ) ) ;
#20691 = CARTESIAN_POINT ( 'NONE',  ( -21.15473383059569557, 8.456223909384457116, -1.500000000000002220 ) ) ;
#20692 = CARTESIAN_POINT ( 'NONE',  ( 3.045412351277957175, -6.376774720514422512, 20.90433128744512814 ) ) ;
#20693 = B_SPLINE_SURFACE_WITH_KNOTS ( 'NONE', 3, 3, ( 
 ( #44214, #13240, #20852, #51828 ),
 ( #96490, #75147, #43710, #81768 ),
 ( #66073, #35104, #35605, #5637 ),
 ( #21346, #36094, #57953, #82264 ),
 ( #82758, #67063, #12238, #97971 ),
 ( #98474, #26982, #89879, #67555 ),
 ( #36583, #11749, #51322, #13738 ),
 ( #52323, #44709, #42727, #4152 ),
 ( #28471, #58448, #59436, #90377 ),
 ( #83258, #28972, #3658, #88891 ) ),
 .UNSPECIFIED., .F., .F., .F.,
 ( 4, 3, 3, 4 ),
 ( 4, 4 ),
 ( 0.0004766839783822019588, 0.1491231665100172521, 0.2234464077758347988, 0.2977696490416523178 ),
 ( 0.1495120545021637604, 0.1506138731775905903 ),
 .UNSPECIFIED. ) ;
#20694 = CARTESIAN_POINT ( 'NONE',  ( 6.499999999999992895, -1.784922709757266047E-15, 0.000000000000000000 ) ) ;
#20695 = CARTESIAN_POINT ( 'NONE',  ( -120.5228709571500900, -24.51254535375842636, 9.355368624242261788 ) ) ;
#20696 = CARTESIAN_POINT ( 'NONE',  ( -115.5228709571500758, -24.83602698348160231, 1.605859176311261960 ) ) ;
#20697 = CARTESIAN_POINT ( 'NONE',  ( -110.6241304692883034, -24.92564183028978775, 1.928384488918251982 ) ) ;
#20698 = CARTESIAN_POINT ( 'NONE',  ( 20.57945552106664877, -7.502658216658728563, -1.500000000000002220 ) ) ;
#20699 = DIRECTION ( 'NONE',  ( 0.000000000000000000, 0.000000000000000000, 1.000000000000000000 ) ) ;
#20700 = LINE ( 'NONE', #20201, #60612 ) ;
#20701 = CARTESIAN_POINT ( 'NONE',  ( -112.6228709571500843, -24.50216790748099527, 0.6166512839513660360 ) ) ;
#20702 = CARTESIAN_POINT ( 'NONE',  ( -58.53403895608763463, -24.65952944569304606, 1.056160979905697461 ) ) ;
#20703 = VERTEX_POINT ( 'NONE', #12107 ) ;
#20704 = PRODUCT ( 'Measuring Tape_Varsay\X2\0131\X0\lan', 'Measuring Tape_Varsay\X2\0131\X0\lan', '', ( #23519 ) ) ;
#20705 = CARTESIAN_POINT ( 'NONE',  ( 9.418145840992488971, -18.15903486995133065, 11.49999999999998934 ) ) ;
#20706 = EDGE_LOOP ( 'NONE', ( #47417, #30361, #25350, #87386, #41958, #30611, #1531 ) ) ;
#20707 = ORIENTED_EDGE ( 'NONE', *, *, #5704, .T. ) ;
#20708 = ORIENTED_EDGE ( 'NONE', *, *, #85849, .T. ) ;
#20709 = EDGE_LOOP ( 'NONE', ( #72221, #97837, #44228, #22161 ) ) ;
#20710 = CARTESIAN_POINT ( 'NONE',  ( 11.60186680256600233, 19.91347440808847935, -1.500000000000002220 ) ) ;
#20711 = CARTESIAN_POINT ( 'NONE',  ( -61.59282253940321539, -24.15543982623907127, -0.2315651400026656481 ) ) ;
#20712 = B_SPLINE_CURVE_WITH_KNOTS ( 'NONE', 3,
 ( #68862, #7450, #84576, #85577, #22167, #99780 ),
 .UNSPECIFIED., .F., .F.,
 ( 4, 2, 4 ),
 ( 0.000000000000000000, 0.001380764517854764966, 0.002761529035709529931 ),
 .UNSPECIFIED. ) ;
#20713 = CARTESIAN_POINT ( 'NONE',  ( 2.165584020960389822, 20.11889322763239107, -1.500000000000002220 ) ) ;
#20714 = ORIENTED_EDGE ( 'NONE', *, *, #58488, .F. ) ;
#20715 = CARTESIAN_POINT ( 'NONE',  ( -97.62287095715004170, -23.96127896941632685, -0.6493128931037805973 ) ) ;
#20716 = AXIS2_PLACEMENT_3D ( 'NONE', #30148, #61122, #8317 ) ;
#20717 = CARTESIAN_POINT ( 'NONE',  ( -41.33442610868027600, -25.31287256288777243, 5.287398422161111000 ) ) ;
#20718 = ADVANCED_FACE ( 'NONE', ( #58308 ), #25840, .T. ) ;
#20719 = CARTESIAN_POINT ( 'NONE',  ( -95.62721569424989809, -24.73486907724918282, 1.287355809206966128 ) ) ;
#20720 = CARTESIAN_POINT ( 'NONE',  ( -99.50802124428108186, -24.66019654487200086, 8.947790411086117501 ) ) ;
#20722 = ORIENTED_EDGE ( 'NONE', *, *, #33366, .F. ) ;
#20721 = CARTESIAN_POINT ( 'NONE',  ( 19.78805588120126302, 8.271231038663975355, 11.49999999999999645 ) ) ;
#20723 = DIRECTION ( 'NONE',  ( -3.773278334453079030E-23, 0.9999999999976377785, 2.173523156925979128E-06 ) ) ;
#20724 = ORIENTED_EDGE ( 'NONE', *, *, #48525, .T. ) ;
#20725 = CARTESIAN_POINT ( 'NONE',  ( 19.22371909900314435, 11.20011194808016342, -1.500000000000002220 ) ) ;
#20726 = CARTESIAN_POINT ( 'NONE',  ( 11.71144010791963730, -17.07555522294065753, 11.49999999999998934 ) ) ;
#20727 = EDGE_CURVE ( 'NONE', #76683, #82898, #10658, .T. ) ;
#20728 = AXIS2_PLACEMENT_3D ( 'NONE', #14234, #31979, #93872 ) ;
#20729 = VERTEX_POINT ( 'NONE', #49701 ) ;
#20730 = CARTESIAN_POINT ( 'NONE',  ( -28.52392022028078600, -24.49901761805231359, 1.056161677404373611 ) ) ;
#20731 = ORIENTED_EDGE ( 'NONE', *, *, #65957, .T. ) ;
#20732 = DIRECTION ( 'NONE',  ( 0.000000000000000000, -1.000000000000000000, 0.000000000000000000 ) ) ;
#20733 = AXIS2_PLACEMENT_3D ( 'NONE', #84284, #93903, #14768 ) ;
#20734 = ORIENTED_EDGE ( 'NONE', *, *, #61964, .F. ) ;
#20735 = CARTESIAN_POINT ( 'NONE',  ( 15.04517842881462819, -14.58609674458608829, -1.500000000000002220 ) ) ;
#20736 = CARTESIAN_POINT ( 'NONE',  ( 18.42579859434530931, 11.83097890990371148, 11.49999999999999645 ) ) ;
#20737 = CARTESIAN_POINT ( 'NONE',  ( -37.65706361072022901, -23.73791477778911485, 11.05961554403171121 ) ) ;
#20738 = CARTESIAN_POINT ( 'NONE',  ( -22.13300264024875119, -4.194623038110560032, -1.500000000000002220 ) ) ;
#20739 = CARTESIAN_POINT ( 'NONE',  ( 19.44712688777480736, 7.780496645421295376, 11.49999999999998934 ) ) ;
#20740 = CARTESIAN_POINT ( 'NONE',  ( 6.199338013146583393, -6.376774720514415407, 20.11757922567734980 ) ) ;
#20741 = DIRECTION ( 'NONE',  ( -3.773278334444165844E-23, 1.000000000000000000, 0.000000000000000000 ) ) ;
#20742 = CARTESIAN_POINT ( 'NONE',  ( -99.62287095715005592, -29.50250243563736774, 8.947779886222138046 ) ) ;
#20743 = EDGE_LOOP ( 'NONE', ( #93308, #44060, #10746, #67534 ) ) ;
#20744 = AXIS2_PLACEMENT_3D ( 'NONE', #8320, #47391, #93044 ) ;
#20745 = ORIENTED_EDGE ( 'NONE', *, *, #31659, .T. ) ;
#20746 = ORIENTED_EDGE ( 'NONE', *, *, #58990, .T. ) ;
#20747 = LINE ( 'NONE', #14132, #70911 ) ;
#20748 = CARTESIAN_POINT ( 'NONE',  ( -21.39523464106120088, -1.845724655749456433, -1.500000000000002220 ) ) ;
#20749 = CARTESIAN_POINT ( 'NONE',  ( -88.62287095715004170, -24.64898659630367916, 1.056161002820827921 ) ) ;
#20750 = ORIENTED_EDGE ( 'NONE', *, *, #30190, .T. ) ;
#20751 = CARTESIAN_POINT ( 'NONE',  ( -11.89019930860364482, -17.45089671868802128, 11.49999999999998934 ) ) ;
#20752 = CARTESIAN_POINT ( 'NONE',  ( -92.62287095715005592, -24.64965695001469115, 8.947790433994180503 ) ) ;
#20753 = CARTESIAN_POINT ( 'NONE',  ( 2.499999999999997335, 4.999999999999999112, 2.100000000000000089 ) ) ;
#20754 = CARTESIAN_POINT ( 'NONE',  ( -83.52214250679790553, -23.48786465467241058, 11.44779295918254469 ) ) ;
#20755 = CARTESIAN_POINT ( 'NONE',  ( 10.62437663934349530, 3.316774720514425567, -27.03002426119959978 ) ) ;
#20756 = CARTESIAN_POINT ( 'NONE',  ( -100.0362565971423976, -25.11991538313833416, 2.885717652640028330 ) ) ;
#20757 = CARTESIAN_POINT ( 'NONE',  ( -2.767897998228395551, 21.91458177938747909, -1.500000000000002220 ) ) ;
#20758 = DIRECTION ( 'NONE',  ( 0.000000000000000000, 2.173523156925980399E-06, -0.9999999999976378895 ) ) ;
#20759 = CARTESIAN_POINT ( 'NONE',  ( -3.103301570662693187, -6.376774720514418959, 20.14409848895067512 ) ) ;
#20760 = CARTESIAN_POINT ( 'NONE',  ( 10.46399479596398052, -2.894108053847758377, -27.03001098546561209 ) ) ;
#20761 = FACE_OUTER_BOUND ( 'NONE', #15873, .T. ) ;
#20762 = CARTESIAN_POINT ( 'NONE',  ( -12.45040968399260883, -14.89389333286084671, 11.49999999999998934 ) ) ;
#20763 = CARTESIAN_POINT ( 'NONE',  ( 2.936642053869352953, -21.15864249054145674, 11.49999999999998934 ) ) ;
#20764 = CARTESIAN_POINT ( 'NONE',  ( 9.402885806365684829, -0.3587747205144265483, 29.04108526060719342 ) ) ;
#20765 = CARTESIAN_POINT ( 'NONE',  ( -121.6228709571500417, -29.50248528299804818, 1.056150453629045360 ) ) ;
#20766 = CARTESIAN_POINT ( 'NONE',  ( -64.55954184534172668, -23.73791477778911840, 11.05961554403170766 ) ) ;
#20767 = CARTESIAN_POINT ( 'NONE',  ( -40.52287095715006870, -29.50247984919015209, -1.443849546365060466 ) ) ;
#20768 = CARTESIAN_POINT ( 'NONE',  ( 9.629844747126790949, -20.51516216672183290, -1.500000000000002220 ) ) ;
#20769 = B_SPLINE_SURFACE_WITH_KNOTS ( 'NONE', 3, 3, ( 
 ( #68391, #15094, #21691, #99323 ),
 ( #92215, #44553, #69385, #54180 ),
 ( #46060, #15587, #6489, #29818 ),
 ( #85104, #77480, #98824, #60291 ),
 ( #90725, #22688, #30823, #76479 ),
 ( #100304, #36932, #21198, #52165 ),
 ( #7981, #5983, #37933, #13585 ) ),
 .UNSPECIFIED., .F., .F., .F.,
 ( 4, 3, 4 ),
 ( 4, 4 ),
 ( 0.7945040050992241421, 0.8970133687736501216, 0.9995227324480761011 ),
 ( 0.4296031653624693414, 0.4308142232466789512 ),
 .UNSPECIFIED. ) ;
#20770 = ORIENTED_EDGE ( 'NONE', *, *, #64265, .T. ) ;
#20771 = CARTESIAN_POINT ( 'NONE',  ( -87.52287095715007581, -23.73934037231757088, 11.05740245334328620 ) ) ;
#20772 = CARTESIAN_POINT ( 'NONE',  ( -104.5562042904834072, -24.64965694238574656, 8.947790433994192938 ) ) ;
#20773 = CARTESIAN_POINT ( 'NONE',  ( 0.4224338394261131779, -19.80333402765648998, 11.49999999999999645 ) ) ;
#20774 = DIRECTION ( 'NONE',  ( -1.000000000000000000, 0.000000000000000000, -0.000000000000000000 ) ) ;
#20775 = EDGE_CURVE ( 'NONE', #39091, #36941, #75692, .T. ) ;
#20776 = DIRECTION ( 'NONE',  ( -3.773278334453079618E-23, 0.9999999999976377785, 2.173523156925979975E-06 ) ) ;
#20777 = ORIENTED_EDGE ( 'NONE', *, *, #91804, .T. ) ;
#20778 = CARTESIAN_POINT ( 'NONE',  ( -59.52287095715007581, -24.33832256527048088, 0.1851278514138623987 ) ) ;
#20779 = CARTESIAN_POINT ( 'NONE',  ( -29.79725469281722994, -25.26026879864525654, 4.359877333242863529 ) ) ;
#20780 = EDGE_CURVE ( 'NONE', #62896, #88037, #51186, .T. ) ;
#20781 = CARTESIAN_POINT ( 'NONE',  ( -100.6597906528727577, -25.17353340775167680, 7.087518319904864583 ) ) ;
#20782 = CARTESIAN_POINT ( 'NONE',  ( -20.67203406374276398, -6.343553224398504220, -1.500000000000002220 ) ) ;
#20783 = DIRECTION ( 'NONE',  ( 0.6451914333552730696, 0.000000000000000000, 0.7640209514960754067 ) ) ;
#20784 = AXIS2_PLACEMENT_3D ( 'NONE', #64902, #95811, #26310 ) ;
#20785 = CARTESIAN_POINT ( 'NONE',  ( -16.24122463664219396, 10.56255597858309869, -1.500000000000002220 ) ) ;
#20786 = EDGE_CURVE ( 'NONE', #41305, #54228, #59575, .T. ) ;
#20787 = LINE ( 'NONE', #97913, #35153 ) ;
#20788 = LINE ( 'NONE', #77070, #26383 ) ;
#20789 = CARTESIAN_POINT ( 'NONE',  ( -17.21045110277357182, -9.822940424218707278, -1.500000000000002220 ) ) ;
#20790 = ORIENTED_EDGE ( 'NONE', *, *, #74726, .F. ) ;
#20791 = EDGE_CURVE ( 'NONE', #99871, #90203, #42087, .T. ) ;
#20792 = CARTESIAN_POINT ( 'NONE',  ( 20.17645099164838030, 1.678240329834772115, 11.49999999999999645 ) ) ;
#20793 = DIRECTION ( 'NONE',  ( 0.000000000000000000, 1.000000000000000000, 0.000000000000000000 ) ) ;
#20794 = EDGE_CURVE ( 'NONE', #78762, #76987, #4015, .T. ) ;
#20795 = DIRECTION ( 'NONE',  ( -1.000000000000000000, -3.773278334444166432E-23, -8.201307841325785021E-29 ) ) ;
#20796 = VERTEX_POINT ( 'NONE', #74023 ) ;
#20797 = DIRECTION ( 'NONE',  ( -0.9940716917543757081, -0.000000000000000000, -0.1087265912856348465 ) ) ;
#20798 = CARTESIAN_POINT ( 'NONE',  ( 31.63524360068765162, 3.637569336689931543, 27.31569296206930630 ) ) ;
#20799 = DIRECTION ( 'NONE',  ( 1.000000000000000000, 0.000000000000000000, 0.000000000000000000 ) ) ;
#20800 = VECTOR ( 'NONE', #46775, 1000.000000000000000 ) ;
#20801 = CARTESIAN_POINT ( 'NONE',  ( 13.91401389203221406, -5.965225279485572685, 158.0376437107427137 ) ) ;
#20802 = B_SPLINE_CURVE_WITH_KNOTS ( 'NONE', 3,
 ( #46673, #22306, #84212, #7097 ),
 .UNSPECIFIED., .F., .F.,
 ( 4, 4 ),
 ( 0.7910648800674725534, 0.8000713113395880871 ),
 .UNSPECIFIED. ) ;
#20803 = LINE ( 'NONE', #6588, #88365 ) ;
#20804 = CARTESIAN_POINT ( 'NONE',  ( -7.287290609967129740, 18.71191762695291771, 11.49999999999998934 ) ) ;
#20805 = EDGE_CURVE ( 'NONE', #98963, #66356, #58797, .T. ) ;
#20806 = FACE_OUTER_BOUND ( 'NONE', #22152, .T. ) ;
#20807 = VERTEX_POINT ( 'NONE', #64937 ) ;
#20808 = CIRCLE ( 'NONE', #92085, 1.399999999999999911 ) ;
#20809 = CARTESIAN_POINT ( 'NONE',  ( 9.198035947750891950, -20.93187084735588144, 11.49999999999999645 ) ) ;
#20810 = CARTESIAN_POINT ( 'NONE',  ( -0.02075734969026423599, 5.356774720514425603, -0.08597719988137648983 ) ) ;
#20811 = CARTESIAN_POINT ( 'NONE',  ( -65.52287095715006160, -29.50248789122583659, 2.256150453626215580 ) ) ;
#20812 = CARTESIAN_POINT ( 'NONE',  ( -53.58953762381673158, -23.47593901973091235, -1.443836447539009749 ) ) ;
#20813 = CARTESIAN_POINT ( 'NONE',  ( -53.01255352321339842, 4.132774720514426292, 35.59556822165056644 ) ) ;
#20814 = B_SPLINE_CURVE_WITH_KNOTS ( 'NONE', 3,
 ( #95668, #73336, #34768, #96660, #25649, #27157, #2329, #88060 ),
 .UNSPECIFIED., .F., .F.,
 ( 4, 2, 2, 4 ),
 ( 6.384118695052880424E-06, 0.002007151183515480143, 0.003007534715925692069, 0.004007918248335903995 ),
 .UNSPECIFIED. ) ;
#20815 = CARTESIAN_POINT ( 'NONE',  ( -118.6228709571500559, -23.73934037231758154, 11.05740245334328442 ) ) ;
#20816 = CARTESIAN_POINT ( 'NONE',  ( -21.57557905285345612, -6.117077608415351087, 11.49999999999999645 ) ) ;
#20817 = CARTESIAN_POINT ( 'NONE',  ( 6.184520403203634942, 6.376774720514426953, -25.32021290018218451 ) ) ;
#20818 = ORIENTED_EDGE ( 'NONE', *, *, #26672, .F. ) ;
#20819 = CARTESIAN_POINT ( 'NONE',  ( -13.67433444753018534, -15.09191755960682890, 11.49999999999998934 ) ) ;
#20820 = ORIENTED_EDGE ( 'NONE', *, *, #665, .T. ) ;
#20821 = EDGE_CURVE ( 'NONE', #33585, #25851, #83243, .T. ) ;
#20822 = CARTESIAN_POINT ( 'NONE',  ( 19.00551534866085746, 12.86435971046890359, -1.500000000000002220 ) ) ;
#20823 = LINE ( 'NONE', #29943, #16079 ) ;
#20824 = ORIENTED_EDGE ( 'NONE', *, *, #84965, .F. ) ;
#20825 = PLANE ( 'NONE',  #75213 ) ;
#20827 = EDGE_CURVE ( 'NONE', #51970, #68195, #51456, .T. ) ;
#20826 = CARTESIAN_POINT ( 'NONE',  ( -77.58171905157765025, -24.66019654487200441, 8.947790411086108620 ) ) ;
#20828 = DIRECTION ( 'NONE',  ( -3.773278334453079618E-23, 0.9999999999976377785, 2.173523156925978705E-06 ) ) ;
#20830 = ORIENTED_EDGE ( 'NONE', *, *, #34131, .F. ) ;
#20829 = CARTESIAN_POINT ( 'NONE',  ( 20.79131504077403747, 4.132458064796619368, 11.49999999999999645 ) ) ;
#20831 = ORIENTED_EDGE ( 'NONE', *, *, #23185, .F. ) ;
#20832 = CARTESIAN_POINT ( 'NONE',  ( -20.56242917251232782, -8.299981740788712870, 11.49999999999998934 ) ) ;
#20833 = CARTESIAN_POINT ( 'NONE',  ( 20.22723401096548201, -3.897675682603606084, -1.500000000000002220 ) ) ;
#20834 = VERTEX_POINT ( 'NONE', #49202 ) ;
#20835 = VERTEX_POINT ( 'NONE', #95854 ) ;
#20836 = DIRECTION ( 'NONE',  ( 0.000000000000000000, 1.000000000000000000, 0.000000000000000000 ) ) ;
#20837 = EDGE_CURVE ( 'NONE', #49749, #53188, #67634, .T. ) ;
#20838 = LINE ( 'NONE', #77122, #95548 ) ;
#20839 = ORIENTED_EDGE ( 'NONE', *, *, #62859, .F. ) ;
#20840 = ORIENTED_EDGE ( 'NONE', *, *, #48438, .F. ) ;
#20841 = AXIS2_PLACEMENT_3D ( 'NONE', #42337, #88493, #86979 ) ;
#20842 = VERTEX_POINT ( 'NONE', #57320 ) ;
#20843 = DIRECTION ( 'NONE',  ( 0.000000000000000000, -1.000000000000000000, 0.000000000000000000 ) ) ;
#20844 = CARTESIAN_POINT ( 'NONE',  ( -20.27875734969026311, -4.543225279485573864, 21.75402280011862644 ) ) ;
#20845 = CYLINDRICAL_SURFACE ( 'NONE', #71446, 1.836000000000000743 ) ;
#20846 = CARTESIAN_POINT ( 'NONE',  ( 16.28047541435887879, -12.87082401369967677, -1.500000000000002220 ) ) ;
#20848 = EDGE_CURVE ( 'NONE', #7941, #66316, #100311, .T. ) ;
#20847 = CARTESIAN_POINT ( 'NONE',  ( -4.559408409702599307, -21.23122434433648209, 11.49999999999999645 ) ) ;
#20849 = ORIENTED_EDGE ( 'NONE', *, *, #69011, .T. ) ;
#20850 = CARTESIAN_POINT ( 'NONE',  ( -51.84906229995659288, -25.19414663990379921, 6.647105277450162220 ) ) ;
#20851 = CARTESIAN_POINT ( 'NONE',  ( -52.52287095715008292, -23.94994826722564341, -0.6494450866342716955 ) ) ;
#20852 = CARTESIAN_POINT ( 'NONE',  ( -115.5589192835139727, -23.48783264082477018, -1.443836473390087916 ) ) ;
#20853 = CARTESIAN_POINT ( 'NONE',  ( -21.98280116189361877, -4.439423430357301470, -1.500000000000002220 ) ) ;
#20854 = AXIS2_PLACEMENT_3D ( 'NONE', #74890, #98225, #6884 ) ;
#20855 = B_SPLINE_CURVE_WITH_KNOTS ( 'NONE', 3,
 ( #63580, #40224, #71177, #48343 ),
 .UNSPECIFIED., .F., .F.,
 ( 4, 4 ),
 ( 0.7703360025610563877, 0.7793424338331719214 ),
 .UNSPECIFIED. ) ;
#20856 = CARTESIAN_POINT ( 'NONE',  ( -51.19090461678316473, -25.31296676361253617, 4.328065606197115223 ) ) ;
#20857 = CARTESIAN_POINT ( 'NONE',  ( -65.53457423475654764, -24.83618233451449697, 1.606449574219540155 ) ) ;
#20858 = VERTEX_POINT ( 'NONE', #43079 ) ;
#20859 = CARTESIAN_POINT ( 'NONE',  ( -59.52287095715006160, -24.64965694238407323, 8.947790433994201820 ) ) ;
#20860 = CARTESIAN_POINT ( 'NONE',  ( -50.78505292327133702, -25.11974106722812650, 2.884744560678632830 ) ) ;
#20861 = VERTEX_POINT ( 'NONE', #91234 ) ;
#20862 = VECTOR ( 'NONE', #32676, 1000.000000000000000 ) ;
#20863 = VERTEX_POINT ( 'NONE', #7002 ) ;
#20864 = DIRECTION ( 'NONE',  ( 1.000000000000000000, 3.773278334444166432E-23, 8.201307841325785021E-29 ) ) ;
#20865 = CC_DESIGN_PERSON_AND_ORGANIZATION_ASSIGNMENT ( #4706, #28528, ( #94066 ) ) ;
#20866 = VERTEX_POINT ( 'NONE', #5501 ) ;
#20867 = CARTESIAN_POINT ( 'NONE',  ( 17.02398533174402218, 12.79255474601471043, -1.500000000000002220 ) ) ;
#20868 = EDGE_LOOP ( 'NONE', ( #60796, #3785 ) ) ;
#20869 = CARTESIAN_POINT ( 'NONE',  ( -6.487934372591614540, -5.876774720514411854, 19.49432735726520605 ) ) ;
#20870 = CARTESIAN_POINT ( 'NONE',  ( 21.45948982579844255, -4.128456637845983934, -1.500000000000002220 ) ) ;
#20871 = CARTESIAN_POINT ( 'NONE',  ( -38.52287095715004739, -23.95044443724991368, 10.65354141964649237 ) ) ;
#20872 = CARTESIAN_POINT ( 'NONE',  ( 22.16846167567618053, -4.910139430472912458, -1.500000000000002220 ) ) ;
#20873 = VECTOR ( 'NONE', #53538, 999.9999999999998863 ) ;
#20874 = CARTESIAN_POINT ( 'NONE',  ( -41.09701627025020088, -25.18430914849951918, 3.494173821712560635 ) ) ;
#20875 = CARTESIAN_POINT ( 'NONE',  ( -123.6228709571500559, -24.64965695001469115, 8.947790433994175174 ) ) ;
#20876 = CARTESIAN_POINT ( 'NONE',  ( -8.322136096487577461, -20.27582920440508829, -1.500000000000002220 ) ) ;
#20877 = CARTESIAN_POINT ( 'NONE',  ( -24.97666371003640506, -0.3587747205143964613, -15.72894043976419454 ) ) ;
#20878 = ORIENTED_EDGE ( 'NONE', *, *, #98727, .F. ) ;
#20879 = CARTESIAN_POINT ( 'NONE',  ( -40.25461668630514112, -25.29393289446231918, 5.534671799676078585 ) ) ;
#20880 = ORIENTED_EDGE ( 'NONE', *, *, #62740, .F. ) ;
#20881 = CARTESIAN_POINT ( 'NONE',  ( 9.278253834636473130, -6.376774720514426953, 21.78128695274316229 ) ) ;
#20882 = CARTESIAN_POINT ( 'NONE',  ( 7.662324775236977636, 31.59999999999999787, 2.100000000000000089 ) ) ;
#20883 = CARTESIAN_POINT ( 'NONE',  ( -0.1051616404667209126, -21.68859992388199487, -0.4716817114508950470 ) ) ;
#20884 = CARTESIAN_POINT ( 'NONE',  ( 16.87399902462237478, -12.92443306546820736, -1.500000000000002220 ) ) ;
#20885 = CARTESIAN_POINT ( 'NONE',  ( -112.5569623344011632, -23.73766607897671577, -1.055555164236427368 ) ) ;
#20886 = CARTESIAN_POINT ( 'NONE',  ( -26.09735693242928534, -24.97064964884102167, 4.864565919031297980 ) ) ;
#20887 = CARTESIAN_POINT ( 'NONE',  ( -85.60742529143259105, -23.48783264082476308, -1.443836473390099018 ) ) ;
#20888 = CARTESIAN_POINT ( 'NONE',  ( -33.57064321401880846, -23.48783264082477729, -1.443836473390078146 ) ) ;
#20889 = AXIS2_PLACEMENT_3D ( 'NONE', #28784, #5444, #76936 ) ;
#20890 = B_SPLINE_CURVE_WITH_KNOTS ( 'NONE', 3,
 ( #2421, #89646, #41478, #65834 ),
 .UNSPECIFIED., .F., .F.,
 ( 4, 4 ),
 ( 0.000000000000000000, 9.999999999998897304E-05 ),
 .UNSPECIFIED. ) ;
#20891 = CARTESIAN_POINT ( 'NONE',  ( -79.62287095715005592, -24.64965695001468404, 8.947790433994182280 ) ) ;
#20892 = VERTEX_POINT ( 'NONE', #84121 ) ;
#20893 = B_SPLINE_CURVE_WITH_KNOTS ( 'NONE', 3,
 ( #52880, #7695, #37646, #69604 ),
 .UNSPECIFIED., .F., .F.,
 ( 4, 4 ),
 ( 0.1498929593708818175, 0.1588993906429972958 ),
 .UNSPECIFIED. ) ;
#20894 = CARTESIAN_POINT ( 'NONE',  ( 14.87128047407919951, 12.67365258641725312, 11.49999999999999645 ) ) ;
#20895 = CARTESIAN_POINT ( 'NONE',  ( -108.5228709571500758, -23.95044443724992789, 10.65354141964648882 ) ) ;
#20896 = EDGE_CURVE ( 'NONE', #11988, #85219, #85777, .T. ) ;
#20897 = DIRECTION ( 'NONE',  ( 0.000000000000000000, 0.000000000000000000, -1.000000000000000000 ) ) ;
#20898 = ORIENTED_EDGE ( 'NONE', *, *, #87824, .T. ) ;
#20899 = DIRECTION ( 'NONE',  ( -3.773278334444167608E-23, 1.000000000000000000, 0.000000000000000000 ) ) ;
#20900 = CARTESIAN_POINT ( 'NONE',  ( -99.19463651313202490, -25.31270078316470773, 5.270598708289442769 ) ) ;
#20901 = CARTESIAN_POINT ( 'NONE',  ( -0.02075734969026423599, -0.3587747205144213303, -0.08597719988137648983 ) ) ;
#20902 = CARTESIAN_POINT ( 'NONE',  ( -50.26656247056430260, -25.12363382914034560, 7.097961812911407264 ) ) ;
#20903 = CARTESIAN_POINT ( 'NONE',  ( -0.8432318219891272726, -19.69000482574202238, 11.49999999999998934 ) ) ;
#20904 = EDGE_LOOP ( 'NONE', ( #41484, #36966, #49233, #63170 ) ) ;
#20905 = EDGE_CURVE ( 'NONE', #69249, #77603, #75002, .T. ) ;
#20906 = CARTESIAN_POINT ( 'NONE',  ( -44.62287095715004881, -29.50250243563736774, 8.947779886222148704 ) ) ;
#20907 = PLANE ( 'NONE',  #73924 ) ;
#20908 = EDGE_CURVE ( 'NONE', #21078, #12640, #25009, .T. ) ;
#20909 = DATE_AND_TIME ( #90434, #438 ) ;
#20910 = ORIENTED_EDGE ( 'NONE', *, *, #36020, .F. ) ;
#20911 = CARTESIAN_POINT ( 'NONE',  ( -72.52287095715007581, -24.65952944569304606, 1.056160979905697239 ) ) ;
#20912 = CARTESIAN_POINT ( 'NONE',  ( -87.58953762381671027, -24.64965694238406613, 8.947790433994653014 ) ) ;
#20913 = CARTESIAN_POINT ( 'NONE',  ( -50.52287095715006160, -29.50248528299804818, 1.056150453629033370 ) ) ;
#20914 = CARTESIAN_POINT ( 'NONE',  ( -116.5228709571500616, -24.64898659630368627, 1.056161002820833028 ) ) ;
#20915 = CARTESIAN_POINT ( 'NONE',  ( -7.318926569091948942, -6.376774720514417183, 20.09505574050193033 ) ) ;
#20916 = VECTOR ( 'NONE', #81496, 1000.000000000000114 ) ;
#20917 = AXIS2_PLACEMENT_3D ( 'NONE', #67273, #3382, #51544 ) ;
#20918 = DIRECTION ( 'NONE',  ( 0.000000000000000000, 0.000000000000000000, 1.000000000000000000 ) ) ;
#20919 = CARTESIAN_POINT ( 'NONE',  ( -107.6248367076318999, -24.51314013834315730, 0.6176544820404215042 ) ) ;
#20920 = CARTESIAN_POINT ( 'NONE',  ( 13.89251353435424363, -14.32104260081073832, 11.49999999999998934 ) ) ;
#20921 = ADVANCED_FACE ( 'NONE', ( #83619 ), #51688, .F. ) ;
#20922 = CARTESIAN_POINT ( 'NONE',  ( -41.62287095715004881, -24.51387760970722240, 9.387446482453418284 ) ) ;
#20923 = CARTESIAN_POINT ( 'NONE',  ( 2.100208336950355914, 2.204364238465233111E-16, -1.249999999999996003 ) ) ;
#20924 = EDGE_LOOP ( 'NONE', ( #63865, #14351, #33987, #45452 ) ) ;
#20925 = VECTOR ( 'NONE', #35228, 1000.000000000000000 ) ;
#20926 = DIRECTION ( 'NONE',  ( 0.7071067811865442421, 0.000000000000000000, 0.7071067811865507924 ) ) ;
#20927 = CARTESIAN_POINT ( 'NONE',  ( 6.875727764383598561, -6.376774720514435835, -25.57138887952572404 ) ) ;
#20928 = CIRCLE ( 'NONE', #24418, 2.249999999999998668 ) ;
#20929 = CARTESIAN_POINT ( 'NONE',  ( -106.6228709571500559, -23.47593901973091235, -1.443836447538999312 ) ) ;
#20930 = DIRECTION ( 'NONE',  ( 0.000000000000000000, 1.000000000000000000, 8.393823270855534040E-16 ) ) ;
#20931 = CARTESIAN_POINT ( 'NONE',  ( -127.1719664006464257, -25.27146806274451407, 5.923224605469175508 ) ) ;
#20932 = CARTESIAN_POINT ( 'NONE',  ( -39.61745222137281530, -23.48783264082476308, -1.443836473390098352 ) ) ;
#20933 = CIRCLE ( 'NONE', #38752, 1.000000000000000222 ) ;
#20934 = CARTESIAN_POINT ( 'NONE',  ( -27.99826093239865443, -25.26026290525073392, 1.648429554944246478 ) ) ;
#20935 = CARTESIAN_POINT ( 'NONE',  ( -1.358974358974357921, -5.876774720514419847, 20.75510817307693046 ) ) ;
#20936 = ORIENTED_EDGE ( 'NONE', *, *, #27894, .F. ) ;
#20937 = CARTESIAN_POINT ( 'NONE',  ( 5.550000000000004263, 0.000000000000000000, 0.000000000000000000 ) ) ;
#20938 = CARTESIAN_POINT ( 'NONE',  ( -127.5558937812824922, -23.96119346886880663, -0.6495511937832001426 ) ) ;
#20939 = ORIENTED_EDGE ( 'NONE', *, *, #18724, .F. ) ;
#20940 = CARTESIAN_POINT ( 'NONE',  ( -19.34540493331696354, 6.066486871809979142, 11.49999999999998934 ) ) ;
#20941 = CARTESIAN_POINT ( 'NONE',  ( -105.5895376238167103, -24.99156044556202971, 7.747789690856172307 ) ) ;
#20942 = CARTESIAN_POINT ( 'NONE',  ( -49.62287095715006302, -24.34917612406837861, 0.1852690917426592920 ) ) ;
#20943 = CARTESIAN_POINT ( 'NONE',  ( 10.57556460110582996, 0.7139560615726621151, -8.999999999999991118 ) ) ;
#20944 = VERTEX_POINT ( 'NONE', #37948 ) ;
#20946 = EDGE_CURVE ( 'NONE', #37715, #90955, #34731, .T. ) ;
#20945 = DIRECTION ( 'NONE',  ( 0.000000000000000000, 1.000000000000000000, 0.000000000000000000 ) ) ;
#20947 = DIRECTION ( 'NONE',  ( 0.000000000000000000, -1.000000000000000000, 0.000000000000000000 ) ) ;
#20948 = CARTESIAN_POINT ( 'NONE',  ( -1.290058840521481454, 20.04182742388497473, -1.500000000000002220 ) ) ;
#20949 = CARTESIAN_POINT ( 'NONE',  ( 20.48634023128459347, 4.603634630958829632, 11.49999999999999645 ) ) ;
#20950 = LINE ( 'NONE', #52419, #56753 ) ;
#20951 = CARTESIAN_POINT ( 'NONE',  ( -70.48846634784443665, -24.92592662359561118, 8.075495903017998245 ) ) ;
#20952 = CARTESIAN_POINT ( 'NONE',  ( -13.58966412916292299, 17.40808962483262690, 11.49999999999998934 ) ) ;
#20953 = CARTESIAN_POINT ( 'NONE',  ( -20.35906544237474236, -2.577633573104691322, -1.500000000000002220 ) ) ;
#20954 = CARTESIAN_POINT ( 'NONE',  ( -75.52287095715006160, -29.50248789122583659, 2.256150453626215580 ) ) ;
#20955 = EDGE_CURVE ( 'NONE', #36399, #77096, #61306, .T. ) ;
#20956 = CARTESIAN_POINT ( 'NONE',  ( -34.62287095715005592, -23.47593901973091235, -1.443836447539013301 ) ) ;
#20957 = DIRECTION ( 'NONE',  ( 7.960204194457801640E-17, 1.000000000000000000, 0.000000000000000000 ) ) ;
#20958 = ORIENTED_EDGE ( 'NONE', *, *, #39107, .T. ) ;
#20959 = DIRECTION ( 'NONE',  ( -0.1311553622875919756, 6.845827386180409975E-16, -0.9913618264504692190 ) ) ;
#20960 = B_SPLINE_SURFACE_WITH_KNOTS ( 'NONE', 3, 3, ( 
 ( #10559, #41520, #63879, #2967 ),
 ( #48648, #56261, #41024, #71977 ),
 ( #64384, #2459, #6443, #51627 ),
 ( #81579, #37399, #44005, #68347 ),
 ( #91666, #82068, #66369, #22145 ),
 ( #12050, #73963, #59744, #60744 ),
 ( #45019, #12554, #14038, #4461 ) ),
 .UNSPECIFIED., .F., .F., .F.,
 ( 4, 3, 4 ),
 ( 4, 4 ),
 ( 0.7945040050992234759, 0.8970133687736494554, 0.9995227324480753239 ),
 ( 0.2395548714580574556, 0.2406781904383525350 ),
 .UNSPECIFIED. ) ;
#20961 = CARTESIAN_POINT ( 'NONE',  ( -31.54521099866208189, -24.15543982623907127, -0.2315651400026576545 ) ) ;
#20962 = ORIENTED_EDGE ( 'NONE', *, *, #96566, .T. ) ;
#20963 = ORIENTED_EDGE ( 'NONE', *, *, #100352, .F. ) ;
#20964 = CARTESIAN_POINT ( 'NONE',  ( -83.52287095715006160, -24.65952944569304606, 1.056160979905698794 ) ) ;
#20965 = CARTESIAN_POINT ( 'NONE',  ( -80.62287095715007013, -23.47596703998600631, 11.44779298504227860 ) ) ;
#20966 = CARTESIAN_POINT ( 'NONE',  ( -29.49875734969026198, 5.965225279485572685, 0.1180228001186258285 ) ) ;
#20967 = CARTESIAN_POINT ( 'NONE',  ( -14.32454646668868747, 14.77526322620295929, -1.500000000000002220 ) ) ;
#20968 = CARTESIAN_POINT ( 'NONE',  ( -13.10987527212420645, -17.12674121770768920, 11.49999999999999645 ) ) ;
#20969 = EDGE_LOOP ( 'NONE', ( #51719, #4232, #13230, #46247 ) ) ;
#20970 = CARTESIAN_POINT ( 'NONE',  ( -59.52287095715006160, -23.47596703998600631, 11.44779298504228926 ) ) ;
#20971 = FACE_OUTER_BOUND ( 'NONE', #44259, .T. ) ;
#20972 = CARTESIAN_POINT ( 'NONE',  ( 22.31825301297700648, 1.237144038376295274, -1.500000000000002220 ) ) ;
#20973 = CARTESIAN_POINT ( 'NONE',  ( -80.05243144761681151, -25.12205794285693372, 7.021016987878912374 ) ) ;
#20974 = DIRECTION ( 'NONE',  ( 0.000000000000000000, 0.000000000000000000, 1.000000000000000000 ) ) ;
#20975 = VERTEX_POINT ( 'NONE', #44570 ) ;
#20976 = DIRECTION ( 'NONE',  ( -0.000000000000000000, -1.000000000000000000, -0.000000000000000000 ) ) ;
#20977 = CARTESIAN_POINT ( 'NONE',  ( -51.22110488517359528, -25.30467804217069272, 4.840842006535183373 ) ) ;
#20978 = CARTESIAN_POINT ( 'NONE',  ( 2.299058169534009100, 20.76012671103276475, -1.500000000000002220 ) ) ;
#20979 = EDGE_LOOP ( 'NONE', ( #41321, #68396, #86285, #42218, #47435, #72615, #45694, #4285, #24846, #92494, #75487 ) ) ;
#20980 = AXIS2_PLACEMENT_3D ( 'NONE', #48914, #11830, #18943 ) ;
#20981 = ADVANCED_FACE ( 'NONE', ( #15110 ), #52681, .T. ) ;
#20983 = ORIENTED_EDGE ( 'NONE', *, *, #47760, .F. ) ;
#20982 = CARTESIAN_POINT ( 'NONE',  ( -67.50091646733569917, -24.35071581493543746, 9.817618358456023486 ) ) ;
#20984 = ORIENTED_EDGE ( 'NONE', *, *, #75467, .F. ) ;
#20985 = CARTESIAN_POINT ( 'NONE',  ( -100.5894357946910418, -24.52399227489127398, 9.353111116836521077 ) ) ;
#20986 = CARTESIAN_POINT ( 'NONE',  ( 20.24497096899912307, 5.935080660949433096, -1.500000000000002220 ) ) ;
#20987 = VERTEX_POINT ( 'NONE', #22207 ) ;
#20988 = DIRECTION ( 'NONE',  ( 0.000000000000000000, -1.000000000000000000, 0.000000000000000000 ) ) ;
#20989 = FACE_OUTER_BOUND ( 'NONE', #42173, .T. ) ;
#20990 = CARTESIAN_POINT ( 'NONE',  ( -61.58953762381671737, -23.48786465467240347, 11.44779295918254824 ) ) ;
#20991 = AXIS2_PLACEMENT_3D ( 'NONE', #13978, #44954, #15969 ) ;
#20992 = CARTESIAN_POINT ( 'NONE',  ( -28.98875734969026396, -0.3587747205144265483, 10.11402280011862587 ) ) ;
#20993 = CARTESIAN_POINT ( 'NONE',  ( -50.22113196962826720, -25.11144614215787385, 2.838499443990665227 ) ) ;
#20994 = CARTESIAN_POINT ( 'NONE',  ( 6.244050601037331560, 20.82503750550150912, -1.500000000000002220 ) ) ;
#20995 = CARTESIAN_POINT ( 'NONE',  ( -79.70858743522369139, -25.08277761643740789, 7.371951261098620201 ) ) ;
#20997 = ORIENTED_EDGE ( 'NONE', *, *, #92733, .T. ) ;
#20996 = CARTESIAN_POINT ( 'NONE',  ( 7.190675130926929448, -21.12231643677837312, 11.49999999999999645 ) ) ;
#20998 = CARTESIAN_POINT ( 'NONE',  ( -33.52287095715006160, -24.65952944569303895, 1.056160979905690134 ) ) ;
#20999 = FACE_OUTER_BOUND ( 'NONE', #19250, .T. ) ;
#21000 = PLANE ( 'NONE',  #29433 ) ;
#21001 = VERTEX_POINT ( 'NONE', #14103 ) ;
#21002 = EDGE_CURVE ( 'NONE', #8368, #92960, #46076, .T. ) ;
#21003 = CIRCLE ( 'NONE', #97204, 129.7684398600581517 ) ;
#21004 = EDGE_CURVE ( 'NONE', #34952, #46589, #63877, .T. ) ;
#21005 = VERTEX_POINT ( 'NONE', #75498 ) ;
#21006 = ORIENTED_EDGE ( 'NONE', *, *, #46551, .T. ) ;
#21007 = EDGE_CURVE ( 'NONE', #57610, #58811, #14606, .T. ) ;
#21008 = AXIS2_PLACEMENT_3D ( 'NONE', #80708, #27425, #79698 ) ;
#21009 = FACE_OUTER_BOUND ( 'NONE', #88564, .T. ) ;
#21010 = CARTESIAN_POINT ( 'NONE',  ( 32.16024265030974050, -5.965225279485572685, 16.27760796525321751 ) ) ;
#21011 = CARTESIAN_POINT ( 'NONE',  ( -49.62287095715005592, -29.50248528299804818, 1.056150453629033370 ) ) ;
#21012 = CARTESIAN_POINT ( 'NONE',  ( -49.74369414166533687, -25.31543073408252909, 4.940877929217667663 ) ) ;
#21013 = VECTOR ( 'NONE', #24492, 1000.000000000000114 ) ;
#21014 = FACE_OUTER_BOUND ( 'NONE', #46222, .T. ) ;
#21015 = CARTESIAN_POINT ( 'NONE',  ( 8.499999999999989342, 18.74999999999999645, 2.100000000000000089 ) ) ;
#21016 = VERTEX_POINT ( 'NONE', #60307 ) ;
#21017 = CARTESIAN_POINT ( 'NONE',  ( 17.72857150710123619, 7.855407458714720903, 11.49999999999999645 ) ) ;
#21018 = DIRECTION ( 'NONE',  ( 0.000000000000000000, 0.000000000000000000, -1.000000000000000000 ) ) ;
#21019 = EDGE_CURVE ( 'NONE', #51364, #64821, #23717, .T. ) ;
#21020 = ORIENTED_EDGE ( 'NONE', *, *, #22599, .T. ) ;
#21021 = DIRECTION ( 'NONE',  ( 0.000000000000000000, 0.9999999999976377785, 2.173523156925979128E-06 ) ) ;
#21022 = CARTESIAN_POINT ( 'NONE',  ( 11.25623914429021788, 5.356774720514424715, -27.04805245727492036 ) ) ;
#21023 = DIRECTION ( 'NONE',  ( 3.773278334444167608E-23, -1.000000000000000000, 0.000000000000000000 ) ) ;
#21024 = LINE ( 'NONE', #53994, #24456 ) ;
#21025 = CARTESIAN_POINT ( 'NONE',  ( -19.37001648656083574, -3.113731218521536004, -1.500000000000002220 ) ) ;
#21026 = CARTESIAN_POINT ( 'NONE',  ( -46.63380027522481441, -24.34968618360932879, 0.1864209137778778391 ) ) ;
#21027 = VERTEX_POINT ( 'NONE', #48588 ) ;
#21028 = CARTESIAN_POINT ( 'NONE',  ( -21.01953065494444317, -4.859126342152997324, 11.49999999999998934 ) ) ;
#21029 = CARTESIAN_POINT ( 'NONE',  ( -33.60141092905455196, -23.96169478059712432, 10.65365249895719124 ) ) ;
#21030 = CARTESIAN_POINT ( 'NONE',  ( -61.64687923781919920, -25.20074463982482982, 3.409327697717700278 ) ) ;
#21031 = CARTESIAN_POINT ( 'NONE',  ( -100.6228709571500559, -23.48783264082478794, -1.443836473390061936 ) ) ;
#21032 = LINE ( 'NONE', #52003, #84450 ) ;
#21033 = CARTESIAN_POINT ( 'NONE',  ( 17.37538969058663696, -15.08583811485692117, -1.500000000000002220 ) ) ;
#21034 = EDGE_CURVE ( 'NONE', #33683, #74588, #386, .T. ) ;
#21035 = EDGE_CURVE ( 'NONE', #25854, #97022, #1187, .T. ) ;
#21036 = DATE_AND_TIME ( #36777, #84598 ) ;
#21037 = DIRECTION ( 'NONE',  ( -3.773278334453079030E-23, 0.9999999999976377785, 2.173523156925979128E-06 ) ) ;
#21038 = CARTESIAN_POINT ( 'NONE',  ( -50.10347978215904874, -25.18370859199909972, 3.285367768258824483 ) ) ;
#21039 = CARTESIAN_POINT ( 'NONE',  ( 6.436487395234643749, 19.08016507665710648, 11.49999999999999645 ) ) ;
#21040 = FACE_OUTER_BOUND ( 'NONE', #96218, .T. ) ;
#21041 = CARTESIAN_POINT ( 'NONE',  ( -32.56126148258746156, -23.73791477778911485, 11.05961554403171299 ) ) ;
#21042 = CARTESIAN_POINT ( 'NONE',  ( -115.6228709571500559, -29.50250786944525672, 11.44777988621622811 ) ) ;
#21043 = CYLINDRICAL_SURFACE ( 'NONE', #48888, 1.399999999999999911 ) ;
#21044 = CARTESIAN_POINT ( 'NONE',  ( -122.5228709571500900, -24.35013146730204170, 9.818937971375095941 ) ) ;
#21045 = CARTESIAN_POINT ( 'NONE',  ( -11.18921147948170614, -16.41150865552512883, -1.500000000000002220 ) ) ;
#21046 = ADVANCED_FACE ( 'NONE', ( #94733 ), #58857, .T. ) ;
#21047 = CARTESIAN_POINT ( 'NONE',  ( -113.5932511717749236, -23.73766607897670156, -1.055555164236448240 ) ) ;
#21048 = CARTESIAN_POINT ( 'NONE',  ( -3.504374479207110316, 19.46862825742285708, -1.500000000000002220 ) ) ;
#21049 = CARTESIAN_POINT ( 'NONE',  ( -126.6248985653323160, -23.73791477778912551, 11.05961554403169878 ) ) ;
#21050 = EDGE_CURVE ( 'NONE', #14844, #65225, #86125, .T. ) ;
#21051 = CARTESIAN_POINT ( 'NONE',  ( -0.9827876235267493099, -6.376774720514415407, 19.81240905262004404 ) ) ;
#21052 = CARTESIAN_POINT ( 'NONE',  ( -37.52287095715007581, -24.34917612407031129, 0.1852690917476942090 ) ) ;
#21053 = CARTESIAN_POINT ( 'NONE',  ( 15.58315679939408582, 13.61395703526229894, 11.49999999999999645 ) ) ;
#21054 = CARTESIAN_POINT ( 'NONE',  ( 11.62916340711181284, 0.3587747205144265483, 28.75961759920349792 ) ) ;
#21055 = AXIS2_PLACEMENT_3D ( 'NONE', #42346, #36209, #59552 ) ;
#21056 = LINE ( 'NONE', #68247, #73997 ) ;
#21057 = CARTESIAN_POINT ( 'NONE',  ( -49.86018645952977835, -25.25138696836355834, 5.308912666256677682 ) ) ;
#21058 = CARTESIAN_POINT ( 'NONE',  ( -22.42851769774927817, -3.676000928666301792, 11.49999999999999645 ) ) ;
#21059 = EDGE_LOOP ( 'NONE', ( #48443, #5707, #30816, #45453 ) ) ;
#21060 = CARTESIAN_POINT ( 'NONE',  ( -46.62287095715004170, -24.35013146730203815, 9.818937971375113705 ) ) ;
#21061 = CARTESIAN_POINT ( 'NONE',  ( -62.62287095715004881, -23.47593901973091235, -1.443836447539007972 ) ) ;
#21062 = AXIS2_PLACEMENT_3D ( 'NONE', #19844, #73651, #96483 ) ;
#21063 = CARTESIAN_POINT ( 'NONE',  ( 8.071512145086503054, -1.000000000000000000, -3.746884140868835367 ) ) ;
#21064 = AXIS2_PLACEMENT_3D ( 'NONE', #2620, #64541, #95451 ) ;
#21065 = DIRECTION ( 'NONE',  ( -0.000000000000000000, 1.000000000000000000, -0.000000000000000000 ) ) ;
#21066 = AXIS2_PLACEMENT_3D ( 'NONE', #88677, #74439, #4932 ) ;
#21067 = EDGE_LOOP ( 'NONE', ( #28742, #22506 ) ) ;
#21068 = ORIENTED_EDGE ( 'NONE', *, *, #21138, .T. ) ;
#21069 = EDGE_CURVE ( 'NONE', #4176, #60428, #32844, .T. ) ;
#21070 = CARTESIAN_POINT ( 'NONE',  ( -98.58953762381673869, -23.47596703998600631, 11.44779298504227683 ) ) ;
#21071 = CARTESIAN_POINT ( 'NONE',  ( 22.56601425305882813, -3.627385684441148506, -1.500000000000002220 ) ) ;
#21072 = CARTESIAN_POINT ( 'NONE',  ( -29.48781380955602316, -24.26270740365838208, 0.1864212292069160337 ) ) ;
#21073 = VECTOR ( 'NONE', #43002, 1000.000000000000114 ) ;
#21074 = CARTESIAN_POINT ( 'NONE',  ( 10.28227983848843152, -18.94921665015282031, -1.500000000000002220 ) ) ;
#21075 = CARTESIAN_POINT ( 'NONE',  ( 30.09341516180546350, 1.477225279485574028, -13.09311774897855862 ) ) ;
#21076 = CARTESIAN_POINT ( 'NONE',  ( -51.62287095715005592, -29.50250243563736774, 8.947779886222146928 ) ) ;
#21077 = CARTESIAN_POINT ( 'NONE',  ( -14.53490578827140212, -17.26895500059623956, 11.49999999999999645 ) ) ;
#21078 = VERTEX_POINT ( 'NONE', #93227 ) ;
#21079 = CIRCLE ( 'NONE', #26011, 6.594667762285749468 ) ;
#21080 = CARTESIAN_POINT ( 'NONE',  ( -27.97282668350885615, -24.81073594632751522, 2.304836069181902314 ) ) ;
#21081 = CARTESIAN_POINT ( 'NONE',  ( -17.28599015371049674, 13.57978550619682956, 11.49999999999998934 ) ) ;
#21083 = CARTESIAN_POINT ( 'NONE',  ( -105.6235594712198775, -25.00182538069147142, 7.747789668545044250 ) ) ;
#21082 = CIRCLE ( 'NONE', #37255, 0.8160000000000007248 ) ;
#21084 = CARTESIAN_POINT ( 'NONE',  ( -28.94649234366282187, -24.79700135719347642, 6.769413541375830512 ) ) ;
#21086 = ORIENTED_EDGE ( 'NONE', *, *, #9511, .F. ) ;
#21085 = EDGE_CURVE ( 'NONE', #57610, #63805, #21400, .T. ) ;
#21087 = DIRECTION ( 'NONE',  ( 0.000000000000000000, 0.000000000000000000, -1.000000000000000000 ) ) ;
#21088 = CARTESIAN_POINT ( 'NONE',  ( -90.52212987707727621, -23.48786465467241769, 11.44779295918255180 ) ) ;
#21089 = ORIENTED_EDGE ( 'NONE', *, *, #97883, .T. ) ;
#21090 = CARTESIAN_POINT ( 'NONE',  ( -36.52287095715009002, -24.66019654487199730, 8.947790411086124607 ) ) ;
#21091 = ORIENTED_EDGE ( 'NONE', *, *, #1690, .T. ) ;
#21092 = VERTEX_POINT ( 'NONE', #8999 ) ;
#21093 = CARTESIAN_POINT ( 'NONE',  ( 0.000000000000000000, -6.943225279485572443, 0.000000000000000000 ) ) ;
#21094 = LINE ( 'NONE', #83492, #69742 ) ;
#21095 = CARTESIAN_POINT ( 'NONE',  ( -36.64923509539228519, -23.96119346886880663, -0.6495511937832127991 ) ) ;
#21096 = CARTESIAN_POINT ( 'NONE',  ( -19.37329759448073574, 6.469241145865432863, -1.500000000000002220 ) ) ;
#21097 = ORIENTED_EDGE ( 'NONE', *, *, #31906, .T. ) ;
#21098 = CARTESIAN_POINT ( 'NONE',  ( -3.035630128403670192, -5.876774720514412742, 19.71630089903357685 ) ) ;
#21099 = CARTESIAN_POINT ( 'NONE',  ( -92.52287095715006160, -24.35013146730203815, 9.818937971375097717 ) ) ;
#21100 = PLANE ( 'NONE',  #1084 ) ;
#21101 = CARTESIAN_POINT ( 'NONE',  ( 21.57151214508649772, 3.625915217019311583E-15, -1.699999999999999956 ) ) ;
#21102 = ORIENTED_EDGE ( 'NONE', *, *, #98209, .F. ) ;
#21103 = DIRECTION ( 'NONE',  ( 1.226388327005079762E-16, 0.000000000000000000, -1.000000000000000000 ) ) ;
#21104 = FACE_OUTER_BOUND ( 'NONE', #48236, .T. ) ;
#21105 = CARTESIAN_POINT ( 'NONE',  ( 11.56195852851363526, -17.29799701895051811, -1.500000000000002220 ) ) ;
#21106 = VERTEX_POINT ( 'NONE', #39952 ) ;
#21108 = ORIENTED_EDGE ( 'NONE', *, *, #72008, .F. ) ;
#21107 = DIRECTION ( 'NONE',  ( 0.000000000000000000, 1.000000000000000000, 0.000000000000000000 ) ) ;
#21109 = EDGE_CURVE ( 'NONE', #27009, #43974, #14220, .T. ) ;
#21110 = DIRECTION ( 'NONE',  ( 0.000000000000000000, 0.000000000000000000, 1.000000000000000000 ) ) ;
#21111 = DIRECTION ( 'NONE',  ( 0.000000000000000000, 0.9999999999976377785, 2.173523156925979128E-06 ) ) ;
#21112 = ORIENTED_EDGE ( 'NONE', *, *, #5680, .T. ) ;
#21113 = ORIENTED_EDGE ( 'NONE', *, *, #74314, .F. ) ;
#21114 = DIRECTION ( 'NONE',  ( -3.773278334453079618E-23, 0.9999999999976377785, 2.173523156925979975E-06 ) ) ;
#21115 = CARTESIAN_POINT ( 'NONE',  ( -119.4728709571500360, -25.30558663486607429, 5.000950657679038791 ) ) ;
#21116 = DIRECTION ( 'NONE',  ( 0.000000000000000000, -1.000000000000000000, 0.000000000000000000 ) ) ;
#21117 = CARTESIAN_POINT ( 'NONE',  ( -95.52287095715006160, -23.47596703998600631, 11.44779298504228215 ) ) ;
#21119 = ORIENTED_EDGE ( 'NONE', *, *, #78074, .T. ) ;
#21118 = CARTESIAN_POINT ( 'NONE',  ( -14.73459587841175633, -16.56598928932902837, 11.49999999999999645 ) ) ;
#21120 = CARTESIAN_POINT ( 'NONE',  ( -62.52287095715006160, -29.50250243563736774, 8.947779886222145151 ) ) ;
#21121 = CARTESIAN_POINT ( 'NONE',  ( 6.494847429386178206, -21.66115869805930672, -1.500000000000002220 ) ) ;
#21122 = EDGE_CURVE ( 'NONE', #71932, #25228, #61172, .T. ) ;
#21123 = EDGE_CURVE ( 'NONE', #64548, #24863, #1900, .T. ) ;
#21124 = EDGE_CURVE ( 'NONE', #37824, #46066, #98874, .T. ) ;
#21126 = ORIENTED_EDGE ( 'NONE', *, *, #85164, .F. ) ;
#21125 = CARTESIAN_POINT ( 'NONE',  ( -46.52287095715004028, -24.66019654487199375, 8.947790411086122830 ) ) ;
#21127 = ORIENTED_EDGE ( 'NONE', *, *, #11289, .F. ) ;
#21128 = EDGE_CURVE ( 'NONE', #2790, #32607, #58679, .T. ) ;
#21129 = B_SPLINE_CURVE_WITH_KNOTS ( 'NONE', 3,
 ( #99450, #28444, #83234, #13717, #68028, #72411 ),
 .UNSPECIFIED., .F., .F.,
 ( 4, 2, 4 ),
 ( 0.000000000000000000, 0.001380901958385395483, 0.002761803916770790967 ),
 .UNSPECIFIED. ) ;
#21130 = FACE_OUTER_BOUND ( 'NONE', #95023, .T. ) ;
#21131 = VECTOR ( 'NONE', #68283, 1000.000000000000114 ) ;
#21132 = CARTESIAN_POINT ( 'NONE',  ( -19.30929855918770954, 5.666966705251045511, 11.49999999999998934 ) ) ;
#21133 = CYLINDRICAL_SURFACE ( 'NONE', #31096, 1.699999999999994849 ) ;
#21134 = EDGE_LOOP ( 'NONE', ( #36755, #4636, #42983, #21163 ) ) ;
#21135 = DIRECTION ( 'NONE',  ( 0.000000000000000000, -1.000000000000000000, 0.000000000000000000 ) ) ;
#21136 = CARTESIAN_POINT ( 'NONE',  ( -14.60993195340527251, 16.82711592829100411, -1.500000000000002220 ) ) ;
#21137 = ADVANCED_FACE ( 'NONE', ( #87634 ), #10499, .F. ) ;
#21138 = EDGE_CURVE ( 'NONE', #89278, #25123, #89627, .T. ) ;
#21139 = ORIENTED_EDGE ( 'NONE', *, *, #9737, .F. ) ;
#21140 = LINE ( 'NONE', #50612, #77278 ) ;
#21141 = CARTESIAN_POINT ( 'NONE',  ( -81.57013478349688285, -25.12715095569221901, 7.081260212053098080 ) ) ;
#21142 = DIRECTION ( 'NONE',  ( -3.773278334453080206E-23, 0.9999999999976377785, 2.173523156925979975E-06 ) ) ;
#21143 = CARTESIAN_POINT ( 'NONE',  ( -84.52287095715006160, -24.65952944569304606, 1.056160979905698794 ) ) ;
#21144 = CARTESIAN_POINT ( 'NONE',  ( -73.62287095715005592, -24.64965695001468404, 8.947790433994184056 ) ) ;
#21145 = EDGE_CURVE ( 'NONE', #83889, #11321, #22666, .T. ) ;
#21146 = CARTESIAN_POINT ( 'NONE',  ( 1.133552453683672745, -19.47370032599940615, -1.500000000000002220 ) ) ;
#21147 = AXIS2_PLACEMENT_3D ( 'NONE', #92862, #23339, #15742 ) ;
#21148 = CARTESIAN_POINT ( 'NONE',  ( -7.042111407433782055, -20.27750348750624099, -1.500000000000002220 ) ) ;
#21149 = CARTESIAN_POINT ( 'NONE',  ( -2.457093156980370452, -6.376774720514411854, 19.51167604195716976 ) ) ;
#21150 = CARTESIAN_POINT ( 'NONE',  ( -123.5228709571500616, -29.50250786944525672, 11.44777988621622811 ) ) ;
#21151 = DIRECTION ( 'NONE',  ( 0.000000000000000000, -1.000000000000000000, 0.000000000000000000 ) ) ;
#21152 = CARTESIAN_POINT ( 'NONE',  ( 12.37853024107498534, -19.16169124346054176, -1.500000000000002220 ) ) ;
#21153 = ADVANCED_FACE ( 'NONE', ( #11998 ), #72591, .T. ) ;
#21154 = VECTOR ( 'NONE', #31395, 1000.000000000000000 ) ;
#21155 = CARTESIAN_POINT ( 'NONE',  ( 0.000000000000000000, 0.000000000000000000, 0.000000000000000000 ) ) ;
#21156 = AXIS2_PLACEMENT_3D ( 'NONE', #72477, #12053, #11067 ) ;
#21157 = LINE ( 'NONE', #97299, #40210 ) ;
#21158 = CARTESIAN_POINT ( 'NONE',  ( 8.071512145086501278, -1.000000000000008882, -3.746884140868835367 ) ) ;
#21159 = CARTESIAN_POINT ( 'NONE',  ( 16.79232260237064978, 10.84791536263152523, 11.49999999999999645 ) ) ;
#21160 = CARTESIAN_POINT ( 'NONE',  ( -111.6228709571500559, -23.47593901973091235, -1.443836447538999312 ) ) ;
#21161 = CARTESIAN_POINT ( 'NONE',  ( -74.53890682171518733, -24.66019654487200441, 8.947790411086105067 ) ) ;
#21162 = CARTESIAN_POINT ( 'NONE',  ( -29.52287095715006160, -29.50248298729119867, -6.412432996800796609E-05 ) ) ;
#21163 = ORIENTED_EDGE ( 'NONE', *, *, #80716, .F. ) ;
#21164 = CARTESIAN_POINT ( 'NONE',  ( -57.52287095715008292, -23.47593901973090524, -1.443836447538997092 ) ) ;
#21165 = CARTESIAN_POINT ( 'NONE',  ( 30.00738719773715601, -4.772774720514425972, -9.049252915307084422 ) ) ;
#21166 = EDGE_CURVE ( 'NONE', #31278, #45090, #43183, .T. ) ;
#21167 = CARTESIAN_POINT ( 'NONE',  ( 21.56942612084361599, 2.798134137018522427, -1.500000000000002220 ) ) ;
#21168 = CARTESIAN_POINT ( 'NONE',  ( -4.977357939505175466, -6.376774720514410077, 19.14913681718893557 ) ) ;
#21169 = CARTESIAN_POINT ( 'NONE',  ( 10.47639735327893362, 16.54961352017854637, -1.500000000000002220 ) ) ;
#21170 = DIRECTION ( 'NONE',  ( -1.000000000000000000, 0.000000000000000000, 0.000000000000000000 ) ) ;
#21171 = ADVANCED_FACE ( 'NONE', ( #52566 ), #43951, .F. ) ;
#21172 = EDGE_CURVE ( 'NONE', #48269, #73030, #29222, .T. ) ;
#21174 = ORIENTED_EDGE ( 'NONE', *, *, #87828, .F. ) ;
#21173 = B_SPLINE_CURVE_WITH_KNOTS ( 'NONE', 3,
 ( #41001, #72453, #19147, #73944, #71958, #2439, #4441, #50607 ),
 .UNSPECIFIED., .F., .F.,
 ( 4, 2, 2, 4 ),
 ( -0.001224554619866347364, -0.0002241820295893646661, 0.0007761905606876180318, 0.002776935741241578874 ),
 .UNSPECIFIED. ) ;
#21175 = CONTEXT_DEPENDENT_SHAPE_REPRESENTATION ( #82251, #59630 ) ;
#21176 = CARTESIAN_POINT ( 'NONE',  ( 5.949073730962466833, -6.475225279485573360, -27.94053387008862188 ) ) ;
#21177 = CARTESIAN_POINT ( 'NONE',  ( 2.677468215678941110, -5.876774720514418959, 20.83735685176740304 ) ) ;
#21178 = CARTESIAN_POINT ( 'NONE',  ( 15.48611046165106941, -13.43736321338083783, 11.49999999999999645 ) ) ;
#21179 = DIRECTION ( 'NONE',  ( 0.000000000000000000, -1.000000000000000000, 0.000000000000000000 ) ) ;
#21180 = CARTESIAN_POINT ( 'NONE',  ( -54.22287095715006444, -23.47596703998600276, 11.44779298504227683 ) ) ;
#21181 = ORIENTED_EDGE ( 'NONE', *, *, #80161, .F. ) ;
#21182 = CARTESIAN_POINT ( 'NONE',  ( 8.071512145086503054, -2.028487854913503696, 6.500000000000000000 ) ) ;
#21183 = CARTESIAN_POINT ( 'NONE',  ( -39.67258447180102365, -25.28892493200908476, 3.621101239112743730 ) ) ;
#21184 = DIRECTION ( 'NONE',  ( -1.000000000000000000, 2.209838822900391329E-16, 0.000000000000000000 ) ) ;
#21185 = DIRECTION ( 'NONE',  ( -0.000000000000000000, 1.000000000000000000, -0.000000000000000000 ) ) ;
#21186 = VERTEX_POINT ( 'NONE', #12987 ) ;
#21187 = LINE ( 'NONE', #36920, #31766 ) ;
#21188 = CARTESIAN_POINT ( 'NONE',  ( -1.973530150111237003, 22.95712487800313539, 11.49999999999999645 ) ) ;
#21189 = CARTESIAN_POINT ( 'NONE',  ( -2.506051680461856890, -22.62920675306992280, 11.49999999999998934 ) ) ;
#21190 = LINE ( 'NONE', #75470, #38904 ) ;
#21191 = CARTESIAN_POINT ( 'NONE',  ( -116.6228709571500417, -23.48786465467241769, 11.44779295918253759 ) ) ;
#21192 = CARTESIAN_POINT ( 'NONE',  ( -49.76601615100549481, -25.22051099802980900, 3.484103503325944207 ) ) ;
#21193 = CARTESIAN_POINT ( 'NONE',  ( -115.5228709571500616, -23.48783264082477018, -1.443836473390083475 ) ) ;
#21194 = CARTESIAN_POINT ( 'NONE',  ( -99.16166289166535819, -25.30157770236289139, 5.311370747789966984 ) ) ;
#21195 = VECTOR ( 'NONE', #88024, 1000.000000000000114 ) ;
#21196 = CARTESIAN_POINT ( 'NONE',  ( 20.57945552106664877, -7.502658216658728563, 11.49999999999998934 ) ) ;
#21197 = CARTESIAN_POINT ( 'NONE',  ( 6.698292889820671725, -5.876774720514424288, 21.80822233811499444 ) ) ;
#21198 = CARTESIAN_POINT ( 'NONE',  ( -87.55830585607125727, -23.73791477778911840, 11.05961554403170588 ) ) ;
#21199 = CARTESIAN_POINT ( 'NONE',  ( -77.62287095715005592, -24.34917612406838217, 0.1852690917426639272 ) ) ;
#21200 = CARTESIAN_POINT ( 'NONE',  ( -5.366453405989236813, 5.449678256205721784E-16, -4.450000000000000178 ) ) ;
#21201 = DIRECTION ( 'NONE',  ( -1.000000000000000000, -3.773278334444166432E-23, -8.201307841325785021E-29 ) ) ;
#21202 = CARTESIAN_POINT ( 'NONE',  ( -86.62287095715005592, -23.72773821059536559, 11.05748984161097681 ) ) ;
#21203 = ORIENTED_EDGE ( 'NONE', *, *, #37967, .T. ) ;
#21204 = CARTESIAN_POINT ( 'NONE',  ( 1.945971545120378288, -20.36639758168144709, 11.49999999999998934 ) ) ;
#21205 = ORIENTED_EDGE ( 'NONE', *, *, #36840, .F. ) ;
#21206 = ORIENTED_EDGE ( 'NONE', *, *, #95520, .T. ) ;
#21207 = ORIENTED_EDGE ( 'NONE', *, *, #94814, .F. ) ;
#21208 = ORIENTED_EDGE ( 'NONE', *, *, #35484, .T. ) ;
#21209 = B_SPLINE_CURVE_WITH_KNOTS ( 'NONE', 3,
 ( #53156, #14572, #97810, #59262 ),
 .UNSPECIFIED., .F., .F.,
 ( 4, 4 ),
 ( 0.000000000000000000, 1.000000000000000000 ),
 .UNSPECIFIED. ) ;
#21210 = CARTESIAN_POINT ( 'NONE',  ( -19.45891602060003578, 12.32625358835968576, -1.500000000000002220 ) ) ;
#21211 = FACE_OUTER_BOUND ( 'NONE', #3511, .T. ) ;
#21212 = CARTESIAN_POINT ( 'NONE',  ( -6.636546740042271963, -19.09123619949631134, -1.500000000000002220 ) ) ;
#21213 = ORIENTED_EDGE ( 'NONE', *, *, #6016, .T. ) ;
#21214 = DIRECTION ( 'NONE',  ( 0.000000000000000000, 0.000000000000000000, 1.000000000000000000 ) ) ;
#21215 = DIRECTION ( 'NONE',  ( 0.000000000000000000, 2.173523156925980399E-06, -0.9999999999976378895 ) ) ;
#21217 = CARTESIAN_POINT ( 'NONE',  ( -31.62287095715005236, -24.64965695001467694, 8.947790433994189385 ) ) ;
#21216 = VECTOR ( 'NONE', #84915, 1000.000000000000114 ) ;
#21218 = CARTESIAN_POINT ( 'NONE',  ( -70.62545212654819693, -24.92564183028979130, 1.928384488918253536 ) ) ;
#21220 = ORIENTED_EDGE ( 'NONE', *, *, #24231, .F. ) ;
#21219 = CARTESIAN_POINT ( 'NONE',  ( 13.27131465344908001, -16.79725507166503462, 11.49999999999999645 ) ) ;
#21221 = DIRECTION ( 'NONE',  ( 0.000000000000000000, 0.000000000000000000, -1.000000000000000000 ) ) ;
#21222 = ORIENTED_EDGE ( 'NONE', *, *, #97697, .T. ) ;
#21223 = CARTESIAN_POINT ( 'NONE',  ( -19.01758589260300525, -8.224767016273846210, 11.49999999999998934 ) ) ;
#21224 = EDGE_LOOP ( 'NONE', ( #47583, #69045, #21699, #16515 ) ) ;
#21225 = DIRECTION ( 'NONE',  ( -3.773278334453079618E-23, 0.9999999999976377785, 2.173523156925979975E-06 ) ) ;
#21226 = ORIENTED_EDGE ( 'NONE', *, *, #79158, .F. ) ;
#21227 = EDGE_CURVE ( 'NONE', #991, #57091, #45692, .T. ) ;
#21228 = CARTESIAN_POINT ( 'NONE',  ( 0.1553305729023591875, 1.423459158329793306, 1.743234701965566823E-16 ) ) ;
#21229 = ORIENTED_EDGE ( 'NONE', *, *, #95946, .T. ) ;
#21230 = EDGE_CURVE ( 'NONE', #23609, #59016, #6877, .T. ) ;
#21231 = CARTESIAN_POINT ( 'NONE',  ( -20.92093621315066443, -1.481899440790641842, -1.500000000000002220 ) ) ;
#21232 = CARTESIAN_POINT ( 'NONE',  ( 10.99670386783381737, -19.00842362925918749, 11.49999999999999645 ) ) ;
#21233 = EDGE_CURVE ( 'NONE', #99101, #48827, #23868, .T. ) ;
#21234 = CARTESIAN_POINT ( 'NONE',  ( -37.53880256316359976, -24.35071581493542325, 9.817618358456030592 ) ) ;
#21235 = CARTESIAN_POINT ( 'NONE',  ( 14.28312119630281174, -17.39864199977734671, 11.49999999999998934 ) ) ;
#21236 = EDGE_CURVE ( 'NONE', #76877, #2242, #74399, .T. ) ;
#21237 = CARTESIAN_POINT ( 'NONE',  ( -20.70934228997045068, 3.328930095467914185, 11.49999999999998934 ) ) ;
#21238 = CARTESIAN_POINT ( 'NONE',  ( 5.642655980204820843, -5.876774720514418071, 20.71586687040766961 ) ) ;
#21239 = EDGE_CURVE ( 'NONE', #82905, #34088, #78385, .T. ) ;
#21240 = CARTESIAN_POINT ( 'NONE',  ( -29.62287095715004881, -23.40875089534885589, 11.44779299594469713 ) ) ;
#21241 = CARTESIAN_POINT ( 'NONE',  ( -53.58953762381671737, -23.48786465467241058, 11.44779295918255002 ) ) ;
#21242 = VERTEX_POINT ( 'NONE', #82013 ) ;
#21243 = VERTEX_POINT ( 'NONE', #84001 ) ;
#21244 = ORIENTED_EDGE ( 'NONE', *, *, #44403, .F. ) ;
#21245 = CARTESIAN_POINT ( 'NONE',  ( -42.62287095715004881, -24.65952944569303895, 1.056160979905691688 ) ) ;
#21246 = CARTESIAN_POINT ( 'NONE',  ( -8.581294335678165908, -19.67629172487136557, -1.500000000000002220 ) ) ;
#21247 = CARTESIAN_POINT ( 'NONE',  ( 5.314386400780318986, 0.3587747205143965723, -28.55951656536880989 ) ) ;
#21248 = ORIENTED_EDGE ( 'NONE', *, *, #85743, .F. ) ;
#21249 = CARTESIAN_POINT ( 'NONE',  ( -11.89019930860364482, -17.45089671868802128, -1.500000000000002220 ) ) ;
#21250 = DIRECTION ( 'NONE',  ( 0.000000000000000000, 0.000000000000000000, -1.000000000000000000 ) ) ;
#21251 = CARTESIAN_POINT ( 'NONE',  ( -64.54381262529305729, -24.34968618360933235, 0.1864209137778785330 ) ) ;
#21252 = CARTESIAN_POINT ( 'NONE',  ( -83.50989887316418958, -24.15620529776628089, 10.23563542870660470 ) ) ;
#21253 = CARTESIAN_POINT ( 'NONE',  ( 5.097264368844749427, -6.475225279485576024, -27.56135813788841560 ) ) ;
#21254 = LINE ( 'NONE', #13642, #61658 ) ;
#21255 = CARTESIAN_POINT ( 'NONE',  ( -4.051365815588555463, -21.74199345402511696, -1.500000000000002220 ) ) ;
#21256 = CARTESIAN_POINT ( 'NONE',  ( -110.9909297185884327, -25.14264188228929697, 6.986250900936915365 ) ) ;
#21257 = EDGE_CURVE ( 'NONE', #82699, #33683, #96794, .T. ) ;
#21258 = CARTESIAN_POINT ( 'NONE',  ( -56.52287095715006160, -23.95044443724991723, 10.65354141964649592 ) ) ;
#21259 = CARTESIAN_POINT ( 'NONE',  ( -67.62287095715005592, -29.50250786944525672, 11.44777988621623699 ) ) ;
#21260 = CARTESIAN_POINT ( 'NONE',  ( -83.52287095715006160, -23.47593901973090524, -1.443836447538996648 ) ) ;
#21261 = CARTESIAN_POINT ( 'NONE',  ( -100.5143560509806377, -24.15503026093913874, -0.2815557561904538653 ) ) ;
#21262 = EDGE_CURVE ( 'NONE', #68431, #48449, #32402, .T. ) ;
#21263 = CARTESIAN_POINT ( 'NONE',  ( -11.04204518803028456, 15.98388583709530941, -1.500000000000002220 ) ) ;
#21264 = CARTESIAN_POINT ( 'NONE',  ( 15.12546962493697933, 15.13007008128210096, 11.49999999999998934 ) ) ;
#21265 = CARTESIAN_POINT ( 'NONE',  ( -69.89335126754821204, -25.05732033941839987, 7.496320311188993557 ) ) ;
#21266 = LINE ( 'NONE', #30388, #51175 ) ;
#21267 = AXIS2_PLACEMENT_3D ( 'NONE', #23507, #7802, #84426 ) ;
#21268 = DIRECTION ( 'NONE',  ( 0.000000000000000000, -1.000000000000000000, 0.000000000000000000 ) ) ;
#21269 = CARTESIAN_POINT ( 'NONE',  ( -29.49875734969026198, 0.3587747205144262708, 0.1180228001186258285 ) ) ;
#21270 = CARTESIAN_POINT ( 'NONE',  ( -8.787219534579676861, -20.84281209399103929, -1.500000000000002220 ) ) ;
#21271 = ORIENTED_EDGE ( 'NONE', *, *, #39975, .T. ) ;
#21272 = DIRECTION ( 'NONE',  ( 0.000000000000000000, 0.000000000000000000, -1.000000000000000000 ) ) ;
#21273 = LINE ( 'NONE', #13660, #39489 ) ;
#21274 = CARTESIAN_POINT ( 'NONE',  ( -17.59554656748941071, 9.132484154288260214, 11.49999999999999645 ) ) ;
#21275 = CARTESIAN_POINT ( 'NONE',  ( -108.6228709571500559, -24.64898659630368627, 1.056161002820831474 ) ) ;
#21276 = B_SPLINE_CURVE_WITH_KNOTS ( 'NONE', 3,
 ( #83162, #67962, #90789, #21258, #5050, #44616 ),
 .UNSPECIFIED., .F., .F.,
 ( 4, 2, 4 ),
 ( 0.000000000000000000, 0.001380901958385387027, 0.002761803916770774053 ),
 .UNSPECIFIED. ) ;
#21277 = B_SPLINE_CURVE_WITH_KNOTS ( 'NONE', 3,
 ( #78714, #79233, #9731, #40687, #33072, #94964 ),
 .UNSPECIFIED., .F., .F.,
 ( 4, 2, 4 ),
 ( 6.391158118970788496E-06, 0.001387004593080789615, 0.002767618028042608501 ),
 .UNSPECIFIED. ) ;
#21278 = CARTESIAN_POINT ( 'NONE',  ( -119.5228709571500758, -24.51283580621365488, 0.6167428607019762588 ) ) ;
#21279 = ORIENTED_EDGE ( 'NONE', *, *, #62501, .F. ) ;
#21280 = CARTESIAN_POINT ( 'NONE',  ( -5.895658455092926076, -6.376774720514418959, 20.50445910983877340 ) ) ;
#21281 = CARTESIAN_POINT ( 'NONE',  ( -79.62287095715005592, -23.48783264082478794, -1.443836473390065489 ) ) ;
#21282 = CARTESIAN_POINT ( 'NONE',  ( -92.52287095715006160, -24.64898659630529210, 1.056161002820827921 ) ) ;
#21283 = CARTESIAN_POINT ( 'NONE',  ( 2.319523670979641849, -21.48760272935114557, 11.49999999999998934 ) ) ;
#21284 = CARTESIAN_POINT ( 'NONE',  ( -27.68651082257923335, -24.79949475646172630, 7.605672536963987262 ) ) ;
#21285 = CARTESIAN_POINT ( 'NONE',  ( -66.52287095715003318, -23.73934037231755667, 11.05740245334329153 ) ) ;
#21286 = CARTESIAN_POINT ( 'NONE',  ( -28.49194798280534968, 0.3587747205144265483, 28.38521343323375490 ) ) ;
#21287 = CARTESIAN_POINT ( 'NONE',  ( -51.62287095715005592, -29.50250786944525672, 11.44777988621624054 ) ) ;
#21288 = EDGE_CURVE ( 'NONE', #15989, #98229, #53054, .T. ) ;
#21289 = CARTESIAN_POINT ( 'NONE',  ( -19.78623529325263775, -1.157695164950638844, -1.500000000000002220 ) ) ;
#21290 = AXIS2_PLACEMENT_3D ( 'NONE', #19286, #57882, #35533 ) ;
#21291 = ORIENTED_EDGE ( 'NONE', *, *, #30050, .T. ) ;
#21292 = SECURITY_CLASSIFICATION ( '', '', #77927 ) ;
#21293 = CARTESIAN_POINT ( 'NONE',  ( 10.94010344783756672, -17.16519937159427656, 11.49999999999999645 ) ) ;
#21294 = CARTESIAN_POINT ( 'NONE',  ( 22.02124265030973760, 7.743225279485574042, 16.20402280011862217 ) ) ;
#21295 = ADVANCED_FACE ( 'NONE', ( #70780 ), #48253, .T. ) ;
#21296 = CARTESIAN_POINT ( 'NONE',  ( 33.00535138976576377, -3.570691370340801640, -12.97242311383999791 ) ) ;
#21297 = ORIENTED_EDGE ( 'NONE', *, *, #93861, .T. ) ;
#21298 = FACE_OUTER_BOUND ( 'NONE', #61722, .T. ) ;
#21299 = CARTESIAN_POINT ( 'NONE',  ( -102.5895376238166961, -23.48783264082478794, -1.443836473390062158 ) ) ;
#21300 = DIRECTION ( 'NONE',  ( 0.000000000000000000, -2.173523156925980399E-06, 0.9999999999976378895 ) ) ;
#21301 = DIRECTION ( 'NONE',  ( -3.773278334453079030E-23, 0.9999999999976377785, 2.173523156925979128E-06 ) ) ;
#21302 = LINE ( 'NONE', #51273, #10653 ) ;
#21303 = CARTESIAN_POINT ( 'NONE',  ( 4.397486433803790007, -19.56896378179033036, -1.500000000000002220 ) ) ;
#21304 = DIRECTION ( 'NONE',  ( -3.773278334453079618E-23, 0.9999999999976377785, 2.173523156925979975E-06 ) ) ;
#21305 = ORIENTED_EDGE ( 'NONE', *, *, #74947, .T. ) ;
#21306 = CARTESIAN_POINT ( 'NONE',  ( -73.62287095715007013, -23.47596703998600276, 11.44779298504227860 ) ) ;
#21307 = CARTESIAN_POINT ( 'NONE',  ( 2.581029390964978187, -22.66945732913600509, 11.49999999999999645 ) ) ;
#21308 = CARTESIAN_POINT ( 'NONE',  ( -30.47287095715008576, -25.09213182968271028, 2.762438726437805858 ) ) ;
#21309 = PLANE ( 'NONE',  #41315 ) ;
#21310 = CARTESIAN_POINT ( 'NONE',  ( -90.52287095715006160, -23.47596703998600631, 11.44779298504228393 ) ) ;
#21311 = B_SPLINE_CURVE_WITH_KNOTS ( 'NONE', 3,
 ( #76540, #99874, #75049, #69946, #32387, #31387 ),
 .UNSPECIFIED., .F., .F.,
 ( 4, 2, 4 ),
 ( 1.570755371633915156E-05, 0.001396183895866088620, 0.002776660238015838181 ),
 .UNSPECIFIED. ) ;
#21312 = CARTESIAN_POINT ( 'NONE',  ( 30.54440242517687665, 0.2147811518489142757, 23.45430928465146891 ) ) ;
#21313 = CARTESIAN_POINT ( 'NONE',  ( -43.52287095715006160, -24.64965694238406613, 8.947790433994205372 ) ) ;
#21314 = AXIS2_PLACEMENT_3D ( 'NONE', #288, #39352, #84024 ) ;
#21315 = CARTESIAN_POINT ( 'NONE',  ( -50.78043790469551055, -25.30419751004783890, 5.186272124421679841 ) ) ;
#21316 = ORIENTED_EDGE ( 'NONE', *, *, #4536, .F. ) ;
#21317 = CARTESIAN_POINT ( 'NONE',  ( -2.495337616714382367, -20.20711602426958819, -1.500000000000002220 ) ) ;
#21318 = ORIENTED_EDGE ( 'NONE', *, *, #52014, .T. ) ;
#21319 = CARTESIAN_POINT ( 'NONE',  ( 17.43399715339889511, -14.94103553264482720, 11.49999999999998934 ) ) ;
#21320 = CARTESIAN_POINT ( 'NONE',  ( -53.52287095715009002, -24.51387760970724727, 9.387446482453409402 ) ) ;
#21321 = ORIENTED_EDGE ( 'NONE', *, *, #97312, .T. ) ;
#21322 = LINE ( 'NONE', #30451, #25020 ) ;
#21323 = CARTESIAN_POINT ( 'NONE',  ( -94.52287095715011844, -23.48783264082477373, -1.443836473390087027 ) ) ;
#21324 = FACE_OUTER_BOUND ( 'NONE', #19706, .T. ) ;
#21326 = ORIENTED_EDGE ( 'NONE', *, *, #62064, .T. ) ;
#21325 = CARTESIAN_POINT ( 'NONE',  ( -0.06837171988653999166, -21.26218376953697486, 11.49999999999999645 ) ) ;
#21327 = VERTEX_POINT ( 'NONE', #62179 ) ;
#21328 = CARTESIAN_POINT ( 'NONE',  ( 7.527104757430762128, -20.84474501729809859, -1.500000000000002220 ) ) ;
#21329 = VECTOR ( 'NONE', #70855, 1000.000000000000000 ) ;
#21330 = CARTESIAN_POINT ( 'NONE',  ( -3.146292006899429783, -20.37002610441940220, -1.500000000000002220 ) ) ;
#21331 = ORIENTED_EDGE ( 'NONE', *, *, #29669, .F. ) ;
#21332 = EDGE_LOOP ( 'NONE', ( #84162, #58787, #60405, #86269 ) ) ;
#21333 = DIRECTION ( 'NONE',  ( -0.000000000000000000, 1.000000000000000000, -0.000000000000000000 ) ) ;
#21334 = CARTESIAN_POINT ( 'NONE',  ( -56.62287095715005592, -24.65952944569304250, 1.056160979905693464 ) ) ;
#21335 = ORIENTED_EDGE ( 'NONE', *, *, #96959, .T. ) ;
#21336 = EDGE_CURVE ( 'NONE', #11878, #10895, #68703, .T. ) ;
#21337 = ORIENTED_EDGE ( 'NONE', *, *, #6609, .F. ) ;
#21338 = DIRECTION ( 'NONE',  ( -3.773278334453079030E-23, 0.9999999999976377785, 2.173523156925979128E-06 ) ) ;
#21339 = CARTESIAN_POINT ( 'NONE',  ( -41.48644761199398090, -24.51419770103157347, 9.386484678747180510 ) ) ;
#21340 = CARTESIAN_POINT ( 'NONE',  ( -94.58953762381671027, -24.64965694238575011, 8.947790433994196491 ) ) ;
#21341 = CARTESIAN_POINT ( 'NONE',  ( -11.59579830748209517, 17.24510332420730663, -1.500000000000002220 ) ) ;
#21342 = CARTESIAN_POINT ( 'NONE',  ( 5.219777686717518961, -21.12652377152128480, 11.49999999999999645 ) ) ;
#21343 = EDGE_CURVE ( 'NONE', #83129, #11050, #30715, .T. ) ;
#21344 = DIRECTION ( 'NONE',  ( 0.000000000000000000, -2.173523156925980399E-06, 0.9999999999976378895 ) ) ;
#21345 = DIRECTION ( 'NONE',  ( -1.000000000000000000, 0.000000000000000000, -0.000000000000000000 ) ) ;
#21346 = CARTESIAN_POINT ( 'NONE',  ( -115.6270136601075649, -24.40034930558991277, 0.3402023900116066257 ) ) ;
#21347 = CARTESIAN_POINT ( 'NONE',  ( -8.519796113377745783, 20.75715399588506926, -1.500000000000002220 ) ) ;
#21348 = EDGE_CURVE ( 'NONE', #37593, #94215, #30364, .T. ) ;
#21349 = CARTESIAN_POINT ( 'NONE',  ( -31.24388727629348494, -24.86441894802673147, 8.247789967202360017 ) ) ;
#21350 = VERTEX_POINT ( 'NONE', #61684 ) ;
#21351 = CARTESIAN_POINT ( 'NONE',  ( -59.52287095715006870, -24.33927499327855060, 9.819080762295822495 ) ) ;
#21352 = AXIS2_PLACEMENT_3D ( 'NONE', #41783, #79318, #73711 ) ;
#21353 = CARTESIAN_POINT ( 'NONE',  ( -51.69717015115858061, -25.25631740715194340, 3.906071115062512700 ) ) ;
#21354 = EDGE_CURVE ( 'NONE', #17901, #34861, #100013, .T. ) ;
#21355 = LOCAL_TIME ( 0, 54, 15.00000000000000000, #324 ) ;
#21356 = VERTEX_POINT ( 'NONE', #46946 ) ;
#21357 = EDGE_CURVE ( 'NONE', #5922, #97920, #41763, .T. ) ;
#21358 = ORIENTED_EDGE ( 'NONE', *, *, #5776, .T. ) ;
#21359 = CARTESIAN_POINT ( 'NONE',  ( -46.50653488599488128, -23.96169478059712432, 10.65365249895718414 ) ) ;
#21360 = ORIENTED_EDGE ( 'NONE', *, *, #71946, .F. ) ;
#21361 = CARTESIAN_POINT ( 'NONE',  ( -11.06822068739258391, -18.21809710261049275, -1.500000000000002220 ) ) ;
#21362 = ORIENTED_EDGE ( 'NONE', *, *, #28364, .T. ) ;
#21363 = CARTESIAN_POINT ( 'NONE',  ( -117.5228709571500758, -23.47596703998600631, 11.44779298504227860 ) ) ;
#21364 = CARTESIAN_POINT ( 'NONE',  ( 4.297136154115697160, 20.59472113332480703, -1.500000000000002220 ) ) ;
#21365 = LINE ( 'NONE', #89400, #31907 ) ;
#21366 = CARTESIAN_POINT ( 'NONE',  ( -11.11902432501355342, 19.77583997595719367, -1.500000000000002220 ) ) ;
#21367 = CARTESIAN_POINT ( 'NONE',  ( -110.4731799116023154, -25.19577767130133950, 3.299187155915005665 ) ) ;
#21368 = CARTESIAN_POINT ( 'NONE',  ( 5.399550031317772891, 1.324225279485572893, -28.54570968858208246 ) ) ;
#21369 = CARTESIAN_POINT ( 'NONE',  ( 17.35060923807083810, -13.37414737355047656, -1.500000000000002220 ) ) ;
#21370 = DIRECTION ( 'NONE',  ( 0.000000000000000000, 2.173523156925980399E-06, -0.9999999999976378895 ) ) ;
#21371 = ORIENTED_EDGE ( 'NONE', *, *, #44763, .T. ) ;
#21372 = CARTESIAN_POINT ( 'NONE',  ( 29.60442047479375205, -4.849628492681046232, 28.81422082199668466 ) ) ;
#21373 = CARTESIAN_POINT ( 'NONE',  ( -120.5228709571500474, -24.62226745350441703, 0.9660975649729574011 ) ) ;
#21374 = DIRECTION ( 'NONE',  ( 0.000000000000000000, 0.000000000000000000, -1.000000000000000000 ) ) ;
#21375 = CARTESIAN_POINT ( 'NONE',  ( -30.59901082992093535, -24.82988274811088658, 8.370978854367630007 ) ) ;
#21376 = CARTESIAN_POINT ( 'NONE',  ( 21.17668642892995834, 2.279540523802085605, 11.49999999999998934 ) ) ;
#21377 = CARTESIAN_POINT ( 'NONE',  ( -55.62287095715007723, -24.15516710230292929, 10.28746687063725851 ) ) ;
#21378 = CARTESIAN_POINT ( 'NONE',  ( -54.52287095715005449, -23.47593901973090169, -1.443836447538997092 ) ) ;
#21379 = CARTESIAN_POINT ( 'NONE',  ( -85.49848347818377192, -24.83618233451451118, 1.606449574219533272 ) ) ;
#21380 = CARTESIAN_POINT ( 'NONE',  ( -33.50411885267913448, -23.96119346886880308, -0.6495511937832006977 ) ) ;
#21381 = VECTOR ( 'NONE', #39366, 1000.000000000000227 ) ;
#21382 = DIRECTION ( 'NONE',  ( 1.000000000000000000, -0.000000000000000000, -0.000000000000000000 ) ) ;
#21383 = ORIENTED_EDGE ( 'NONE', *, *, #33756, .F. ) ;
#21384 = CARTESIAN_POINT ( 'NONE',  ( -99.51322475060698025, -25.09877457005609358, 7.289752353020987563 ) ) ;
#21385 = CARTESIAN_POINT ( 'NONE',  ( -15.96901387740391343, -11.39031854172415947, 11.49999999999999645 ) ) ;
#21386 = CARTESIAN_POINT ( 'NONE',  ( -75.55620429048337883, -24.99156044556202261, 7.747789690856173195 ) ) ;
#21387 = DIRECTION ( 'NONE',  ( 1.000000000000000000, 3.773278334444167608E-23, 8.201307833595939069E-29 ) ) ;
#21388 = ORIENTED_EDGE ( 'NONE', *, *, #86529, .F. ) ;
#21389 = CARTESIAN_POINT ( 'NONE',  ( -70.27422298781921484, -25.30465073045868252, 4.851635164186505200 ) ) ;
#21390 = CARTESIAN_POINT ( 'NONE',  ( -99.29687923781919778, -25.25095983749288919, 6.149712203964893042 ) ) ;
#21391 = DIRECTION ( 'NONE',  ( -2.910297583984928910E-15, -1.000000000000000000, 3.056206645085457922E-15 ) ) ;
#21392 = DIRECTION ( 'NONE',  ( 0.000000000000000000, 0.000000000000000000, -1.000000000000000000 ) ) ;
#21393 = CARTESIAN_POINT ( 'NONE',  ( -5.312243195520525596, -18.98051080891723430, -1.500000000000002220 ) ) ;
#21394 = ORIENTED_EDGE ( 'NONE', *, *, #88072, .T. ) ;
#21395 = VECTOR ( 'NONE', #9944, 1000.000000000000000 ) ;
#21396 = VECTOR ( 'NONE', #41794, 1000.000000000000000 ) ;
#21397 = LINE ( 'NONE', #98527, #90966 ) ;
#21398 = FACE_OUTER_BOUND ( 'NONE', #52484, .T. ) ;
#21399 = EDGE_CURVE ( 'NONE', #66223, #30337, #100195, .T. ) ;
#21400 = B_SPLINE_CURVE_WITH_KNOTS ( 'NONE', 3,
 ( #31845, #16601, #47579, #78498 ),
 .UNSPECIFIED., .F., .F.,
 ( 4, 4 ),
 ( 0.000000000000000000, 9.999999999998897304E-05 ),
 .UNSPECIFIED. ) ;
#21401 = DATE_AND_TIME ( #67120, #53833 ) ;
#21402 = EDGE_CURVE ( 'NONE', #72334, #81022, #91687, .T. ) ;
#21403 = ORIENTED_EDGE ( 'NONE', *, *, #44768, .F. ) ;
#21404 = CARTESIAN_POINT ( 'NONE',  ( -27.96875734969026084, -6.475225279485573360, 0.7300228001186309656 ) ) ;
#21405 = CARTESIAN_POINT ( 'NONE',  ( -1.456683411003494966, -6.376774720514415407, 19.95737465391042775 ) ) ;
#21406 = CARTESIAN_POINT ( 'NONE',  ( -55.62373610541767732, -25.00158670708910336, 2.256160236439221034 ) ) ;
#21407 = CARTESIAN_POINT ( 'NONE',  ( -118.5200172836564434, -23.96119346886881019, -0.6495511937832023630 ) ) ;
#21408 = CARTESIAN_POINT ( 'NONE',  ( -7.326695514711824231, -6.376774720514417183, 20.26757654895259719 ) ) ;
#21409 = PLANE ( 'NONE',  #345 ) ;
#21410 = LINE ( 'NONE', #28536, #81845 ) ;
#21411 = CARTESIAN_POINT ( 'NONE',  ( -11.50144725928494438, 16.33591932373696665, 11.49999999999998934 ) ) ;
#21412 = DIRECTION ( 'NONE',  ( 1.000000000000000000, 0.000000000000000000, 0.000000000000000000 ) ) ;
#21413 = CARTESIAN_POINT ( 'NONE',  ( -45.57314203077795156, -25.00182538069146787, 7.747789668545045139 ) ) ;
#21414 = ORIENTED_EDGE ( 'NONE', *, *, #55153, .F. ) ;
#21415 = DIRECTION ( 'NONE',  ( 4.472869286569333237E-16, -1.000000000000000000, -7.102795889480452575E-16 ) ) ;
#21416 = CARTESIAN_POINT ( 'NONE',  ( 4.639188450898540594, -6.376774720514418959, 20.39229233339611014 ) ) ;
#21417 = CIRCLE ( 'NONE', #356, 3.500000000000000000 ) ;
#21419 = CARTESIAN_POINT ( 'NONE',  ( -66.52287095715006160, -24.65952944569304606, 1.056160979905697239 ) ) ;
#21418 = PRODUCT_DEFINITION_FORMATION_WITH_SPECIFIED_SOURCE ( 'ANY', '', #2853, .NOT_KNOWN. ) ;
#21420 = CARTESIAN_POINT ( 'NONE',  ( -98.62287095715005592, -29.50250243563736774, 8.947779886222138046 ) ) ;
#21421 = LINE ( 'NONE', #82831, #62401 ) ;
#21422 = CARTESIAN_POINT ( 'NONE',  ( -81.62360513611031365, -24.65952944569304961, 1.056160979905703901 ) ) ;
#21423 = CARTESIAN_POINT ( 'NONE',  ( 3.180076745125955284, 6.376774720514426953, -28.87659520466658236 ) ) ;
#21424 = CC_DESIGN_PERSON_AND_ORGANIZATION_ASSIGNMENT ( #10450, #64779, ( #37589 ) ) ;
#21425 = CARTESIAN_POINT ( 'NONE',  ( -1.380763273332680896, -5.876774720514418071, 20.28973052848695602 ) ) ;
#21426 = LINE ( 'NONE', #90459, #18751 ) ;
#21427 = CARTESIAN_POINT ( 'NONE',  ( -127.6234793005920380, -24.65952944569305316, 1.056160979905708341 ) ) ;
#21428 = ORIENTED_EDGE ( 'NONE', *, *, #90335, .T. ) ;
#21429 = CARTESIAN_POINT ( 'NONE',  ( -0.6865706486018943178, -20.24796467851281179, 11.49999999999998934 ) ) ;
#21430 = VECTOR ( 'NONE', #33870, 1000.000000000000114 ) ;
#21431 = CARTESIAN_POINT ( 'NONE',  ( -108.6228709571500559, -29.50250786944525672, 11.44777988621622988 ) ) ;
#21432 = CARTESIAN_POINT ( 'NONE',  ( 21.29813515305326632, 4.383221189982441146, -16.78466049732684695 ) ) ;
#21433 = LINE ( 'NONE', #82844, #91367 ) ;
#21434 = ORIENTED_EDGE ( 'NONE', *, *, #67093, .F. ) ;
#21435 = LINE ( 'NONE', #91960, #89028 ) ;
#21436 = PLANE ( 'NONE',  #8127 ) ;
#21437 = CARTESIAN_POINT ( 'NONE',  ( 7.329891291799937925, -18.66831812819665970, -1.500000000000002220 ) ) ;
#21438 = CARTESIAN_POINT ( 'NONE',  ( 1.943494986365726485, -21.02143711168614004, 11.49999999999999645 ) ) ;
#21439 = PLANE ( 'NONE',  #45369 ) ;
#21440 = CARTESIAN_POINT ( 'NONE',  ( -70.60486560330774353, -23.85049219812685806, 10.88485053497527311 ) ) ;
#21441 = CARTESIAN_POINT ( 'NONE',  ( -20.36895902721504825, -8.506870616244709637, 11.49999999999998934 ) ) ;
#21442 = CARTESIAN_POINT ( 'NONE',  ( -0.1859688948871585645, 20.53422428922035081, 11.49999999999998934 ) ) ;
#21443 = DIRECTION ( 'NONE',  ( -3.773278334453080206E-23, 0.9999999999976377785, 2.173523156925979975E-06 ) ) ;
#21444 = VECTOR ( 'NONE', #67222, 1000.000000000000000 ) ;
#21445 = CARTESIAN_POINT ( 'NONE',  ( -4.141025641025642301, -6.376774720514411854, 19.63681891025641235 ) ) ;
#21446 = CARTESIAN_POINT ( 'NONE',  ( -47.62287095715004881, -29.50250243563736774, 8.947779886222146928 ) ) ;
#21447 = ORIENTED_EDGE ( 'NONE', *, *, #93486, .T. ) ;
#21448 = CARTESIAN_POINT ( 'NONE',  ( 4.712727796232543120, -5.356774720514425603, -25.55789472434992859 ) ) ;
#21449 = CARTESIAN_POINT ( 'NONE',  ( -117.5228709571500758, -24.64898659630368272, 1.056161002820833028 ) ) ;
#21450 = VERTEX_POINT ( 'NONE', #71786 ) ;
#21451 = B_SPLINE_CURVE_WITH_KNOTS ( 'NONE', 3,
 ( #88756, #98340, #27349, #59300, #52186, #59810 ),
 .UNSPECIFIED., .F., .F.,
 ( 4, 2, 4 ),
 ( 6.391158118967745954E-06, 0.001387004593080786363, 0.002767618028042605031 ),
 .UNSPECIFIED. ) ;
#21452 = B_SPLINE_CURVE_WITH_KNOTS ( 'NONE', 3,
 ( #30559, #39170, #23944, #77718 ),
 .UNSPECIFIED., .F., .F.,
 ( 4, 4 ),
 ( 1.492656813173654180E-05, 0.002483556359836170454 ),
 .UNSPECIFIED. ) ;
#21453 = ORIENTED_EDGE ( 'NONE', *, *, #2020, .T. ) ;
#21454 = LINE ( 'NONE', #23444, #72952 ) ;
#21455 = PLANE ( 'NONE',  #42176 ) ;
#21456 = CARTESIAN_POINT ( 'NONE',  ( -76.58806799865949699, -24.34968618360934300, 0.1864209137778859160 ) ) ;
#21457 = CARTESIAN_POINT ( 'NONE',  ( 14.24201292913401140, 14.87178044790754328, -1.500000000000002220 ) ) ;
#21458 = CARTESIAN_POINT ( 'NONE',  ( 20.54099941694853726, 6.510794959084822864, 11.49999999999999645 ) ) ;
#21459 = ORIENTED_EDGE ( 'NONE', *, *, #51643, .F. ) ;
#21460 = LINE ( 'NONE', #89499, #27193 ) ;
#21461 = CARTESIAN_POINT ( 'NONE',  ( 13.91401389203221406, -3.316774720514426456, 158.0376437107427137 ) ) ;
#21462 = CARTESIAN_POINT ( 'NONE',  ( 22.34790896907852442, -0.4833156648990815651, -1.500000000000002220 ) ) ;
#21463 = CARTESIAN_POINT ( 'NONE',  ( -93.52287095715010423, -24.33832256527049509, 0.1851278514138617326 ) ) ;
#21464 = CARTESIAN_POINT ( 'NONE',  ( -84.50669220013847394, -24.34968618360934300, 0.1864209137778835013 ) ) ;
#21465 = EDGE_LOOP ( 'NONE', ( #51799, #37599, #68815, #32602, #24064, #43567 ) ) ;
#21466 = LINE ( 'NONE', #37217, #80920 ) ;
#21467 = CARTESIAN_POINT ( 'NONE',  ( -35.62991077901555315, -24.83644354573578994, 8.397322867130093016 ) ) ;
#21468 = AXIS2_PLACEMENT_3D ( 'NONE', #93539, #94547, #55007 ) ;
#21469 = EDGE_CURVE ( 'NONE', #14570, #18015, #90433, .T. ) ;
#21470 = CARTESIAN_POINT ( 'NONE',  ( -18.00717387566553995, 10.56535500573724740, 11.49999999999998934 ) ) ;
#21471 = EDGE_CURVE ( 'NONE', #56978, #19777, #96605, .T. ) ;
#21472 = EDGE_LOOP ( 'NONE', ( #26654, #15014, #58702, #86993 ) ) ;
#21474 = VERTEX_POINT ( 'NONE', #26102 ) ;
#21473 = CARTESIAN_POINT ( 'NONE',  ( -86.55452917198827834, -23.96119346886881374, -0.6495511937831903726 ) ) ;
#21475 = EDGE_LOOP ( 'NONE', ( #78469, #60073, #85366, #23629 ) ) ;
#21476 = CARTESIAN_POINT ( 'NONE',  ( -100.5858019367288136, -24.83644354573579349, 8.397322867130096569 ) ) ;
#21477 = CARTESIAN_POINT ( 'NONE',  ( 18.35617536642501690, 10.39506492455470088, -1.500000000000002220 ) ) ;
#21478 = ORIENTED_EDGE ( 'NONE', *, *, #17837, .T. ) ;
#21479 = CARTESIAN_POINT ( 'NONE',  ( -19.80875734969026425, -5.965225279485572685, 31.02402280011862246 ) ) ;
#21480 = LINE ( 'NONE', #17259, #33671 ) ;
#21481 = CARTESIAN_POINT ( 'NONE',  ( -21.74948284930419717, -1.071797830193938372, 11.49999999999998934 ) ) ;
#21482 = CARTESIAN_POINT ( 'NONE',  ( -72.62287095715005592, -23.47593901973091235, -1.443836447539006196 ) ) ;
#21483 = DIRECTION ( 'NONE',  ( 0.000000000000000000, 0.000000000000000000, -1.000000000000000000 ) ) ;
#21484 = CARTESIAN_POINT ( 'NONE',  ( -84.55620429048340725, -24.64965694238574656, 8.947790433994198267 ) ) ;
#21485 = CARTESIAN_POINT ( 'NONE',  ( 18.95625057990686813, 10.65820999021175730, -1.500000000000002220 ) ) ;
#21486 = DIRECTION ( 'NONE',  ( 0.000000000000000000, -1.000000000000000000, 0.000000000000000000 ) ) ;
#21488 = ORIENTED_EDGE ( 'NONE', *, *, #66648, .F. ) ;
#21487 = CARTESIAN_POINT ( 'NONE',  ( -22.22805510923732086, 2.117028069546627922, 11.49999999999999645 ) ) ;
#21489 = ADVANCED_FACE ( 'NONE', ( #73284, #34224 ), #33719, .T. ) ;
#21490 = LINE ( 'NONE', #97630, #8045 ) ;
#21491 = DIRECTION ( 'NONE',  ( 0.000000000000000000, 0.000000000000000000, -1.000000000000000000 ) ) ;
#21492 = CARTESIAN_POINT ( 'NONE',  ( 0.4325450954222598288, -2.349999999999997868, 0.000000000000000000 ) ) ;
#21493 = ORIENTED_EDGE ( 'NONE', *, *, #9576, .T. ) ;
#21494 = ORIENTED_EDGE ( 'NONE', *, *, #70406, .F. ) ;
#21495 = VECTOR ( 'NONE', #76561, 1000.000000000000000 ) ;
#21496 = ORIENTED_EDGE ( 'NONE', *, *, #42343, .T. ) ;
#21497 = SECURITY_CLASSIFICATION ( '', '', #45759 ) ;
#21498 = CYLINDRICAL_SURFACE ( 'NONE', #38377, 28.45799999999999486 ) ;
#21499 = B_SPLINE_CURVE_WITH_KNOTS ( 'NONE', 3,
 ( #62344, #936, #31886, #76042, #76536, #62860 ),
 .UNSPECIFIED., .F., .F.,
 ( 4, 2, 4 ),
 ( 0.001160938631735150117, 0.001382550680209819645, 0.001604162728684488956 ),
 .UNSPECIFIED. ) ;
#21500 = DIRECTION ( 'NONE',  ( 0.000000000000000000, 0.9999999999976377785, 2.173523156925979128E-06 ) ) ;
#21501 = CARTESIAN_POINT ( 'NONE',  ( 29.70220533163293908, -3.584876737299458771, 28.20564067568759015 ) ) ;
#21502 = DIRECTION ( 'NONE',  ( 0.4109113463207474393, 0.000000000000000000, -0.9116753070391184766 ) ) ;
#21503 = CARTESIAN_POINT ( 'NONE',  ( -0.02075734969026423599, -3.316774720514426456, -0.08597719988137648983 ) ) ;
#21505 = CARTESIAN_POINT ( 'NONE',  ( -19.35591191756920892, -0.7100623379298715010, -1.500000000000002220 ) ) ;
#21504 = VECTOR ( 'NONE', #12568, 1000.000000000000227 ) ;
#21506 = DIRECTION ( 'NONE',  ( 3.773278334444167608E-23, -1.000000000000000000, 0.000000000000000000 ) ) ;
#21507 = ORIENTED_EDGE ( 'NONE', *, *, #41645, .F. ) ;
#21508 = CARTESIAN_POINT ( 'NONE',  ( -8.858824863812619910, -17.32749669425128047, 11.49999999999999645 ) ) ;
#21509 = FACE_OUTER_BOUND ( 'NONE', #83911, .T. ) ;
#21510 = AXIS2_PLACEMENT_3D ( 'NONE', #397, #38958, #30345 ) ;
#21511 = ORIENTED_EDGE ( 'NONE', *, *, #9217, .F. ) ;
#21512 = LINE ( 'NONE', #75306, #57263 ) ;
#21513 = CARTESIAN_POINT ( 'NONE',  ( 2.747717285871495108, -5.876774720514405637, 18.94713297040818034 ) ) ;
#21514 = CYLINDRICAL_SURFACE ( 'NONE', #25490, 0.2999999999999981570 ) ;
#21515 = LINE ( 'NONE', #83421, #94140 ) ;
#21516 = ADVANCED_FACE ( 'NONE', ( #57072 ), #64192, .F. ) ;
#21517 = CARTESIAN_POINT ( 'NONE',  ( 18.19143915067776263, 7.407926943018095400, -1.500000000000002220 ) ) ;
#21518 = B_SPLINE_SURFACE_WITH_KNOTS ( 'NONE', 3, 1, ( 
 ( #41498, #74798 ),
 ( #26267, #59598 ),
 ( #18642, #49620 ),
 ( #11044, #42009 ),
 ( #72951, #3448 ),
 ( #15392, #84414 ),
 ( #77284, #30621 ),
 ( #38731, #84907 ),
 ( #16392, #91524 ),
 ( #47359, #45373 ),
 ( #6293, #68701 ),
 ( #69697, #53980 ),
 ( #23490, #62093 ),
 ( #6784, #179 ),
 ( #76290, #99129 ),
 ( #7786, #62587 ),
 ( #85407, #100108 ),
 ( #52979, #83915 ),
 ( #61602, #37741 ),
 ( #675, #31120 ),
 ( #93013, #24008 ),
 ( #14393, #46354 ),
 ( #54471, #99620 ),
 ( #92518, #30121 ),
 ( #29628, #15894 ),
 ( #61094, #22992 ),
 ( #37251, #22496 ) ),
 .UNSPECIFIED., .F., .F., .F.,
 ( 4, 1, 1, 1, 1, 1, 1, 1, 1, 1, 1, 1, 1, 1, 1, 1, 1, 1, 1, 1, 1, 1, 1, 1, 4 ),
 ( 2, 2 ),
 ( 0.000000000000000000, 0.04401447057613983027, 0.08743412366770532407, 0.1301183986578977048, 0.1725536945581823134, 0.2145547559681394989, 0.2562980920971315024, 0.2984382251332498015, 0.3408490025880946961, 0.3827151889670263873, 0.4239240454075315911, 0.4642462432504168568, 0.5040736714617970460, 0.5438619058684905916, 0.5835667249796533396, 0.6230943188523323517, 0.6632290607685835671, 0.7035512586114681666, 0.7439378946861853192, 0.7845412548000912922, 0.8257501112405982724, 0.8677573633885087290, 0.9107451640323117603, 0.9549144468914786410, 1.000000000000000000 ),
 ( 0.000000000000000000, 1.000000000000000000 ),
 .UNSPECIFIED. ) ;
#21519 = FACE_OUTER_BOUND ( 'NONE', #9732, .T. ) ;
#21520 = ORIENTED_EDGE ( 'NONE', *, *, #100223, .F. ) ;
#21521 = CARTESIAN_POINT ( 'NONE',  ( 17.62533924669398999, -12.40915598911231577, 11.49999999999998934 ) ) ;
#21522 = FACE_OUTER_BOUND ( 'NONE', #49072, .T. ) ;
#21523 = DIRECTION ( 'NONE',  ( -1.000000000000000000, 0.000000000000000000, -0.000000000000000000 ) ) ;
#21524 = CARTESIAN_POINT ( 'NONE',  ( -50.52287095715006160, -24.14321612903118108, -0.2833117244520885203 ) ) ;
#21525 = CARTESIAN_POINT ( 'NONE',  ( -99.67151487672813914, -25.18439404741721788, 3.611381302008842997 ) ) ;
#21526 = CARTESIAN_POINT ( 'NONE',  ( 22.18053613645642841, 6.281410551025238043, -1.500000000000002220 ) ) ;
#21527 = ADVANCED_FACE ( 'NONE', ( #87504 ), #17990, .F. ) ;
#21528 = APPLICATION_PROTOCOL_DEFINITION ( 'international standard', 'config_control_design', 1994, #16760 ) ;
#21529 = CARTESIAN_POINT ( 'NONE',  ( 0.2746452767749879009, 3.927610442141378666, -1.700000000000009059 ) ) ;
#21530 = LINE ( 'NONE', #67743, #79858 ) ;
#21531 = CARTESIAN_POINT ( 'NONE',  ( 5.670567493371958534, -19.34269084982597775, 11.49999999999999645 ) ) ;
#21532 = DIRECTION ( 'NONE',  ( 0.000000000000000000, -1.000000000000000000, 0.000000000000000000 ) ) ;
#21533 = CARTESIAN_POINT ( 'NONE',  ( 11.05000000000000426, -2.000000000000000888, 18.24068255301867936 ) ) ;
#21534 = CARTESIAN_POINT ( 'NONE',  ( -4.743266218460161276, -5.876774720514413630, 19.49357334786887108 ) ) ;
#21535 = DIRECTION ( 'NONE',  ( -3.773278334453079618E-23, 0.9999999999976377785, 2.173523156925979975E-06 ) ) ;
#21536 = CARTESIAN_POINT ( 'NONE',  ( -111.1810695982967161, -25.29779247168320566, 3.716321001747168395 ) ) ;
#21537 = CARTESIAN_POINT ( 'NONE',  ( 15.94990109002195489, -11.90149544800030590, -1.500000000000002220 ) ) ;
#21538 = AXIS2_PLACEMENT_3D ( 'NONE', #50217, #11636, #2545 ) ;
#21539 = DIRECTION ( 'NONE',  ( 0.000000000000000000, 2.173523156925980399E-06, -0.9999999999976378895 ) ) ;
#21540 = CARTESIAN_POINT ( 'NONE',  ( 19.48663422773152121, -3.193742178437300794, -1.500000000000002220 ) ) ;
#21541 = LINE ( 'NONE', #14434, #81576 ) ;
#21542 = B_SPLINE_CURVE_WITH_KNOTS ( 'NONE', 3,
 ( #60033, #75719, #30049, #61025, #21432, #28564, #76222, #37179, #37672, #6220 ),
 .UNSPECIFIED., .F., .F.,
 ( 4, 2, 2, 2, 4 ),
 ( 0.0003558180612557550128, 0.001068662273289818030, 0.001781506485323880885, 0.002494350697357944173, 0.003207194909392007028 ),
 .UNSPECIFIED. ) ;
#21543 = AXIS2_PLACEMENT_3D ( 'NONE', #62257, #56150, #40414 ) ;
#21544 = DESIGN_CONTEXT ( 'detailed design', #18107, 'design' ) ;
#21545 = CARTESIAN_POINT ( 'NONE',  ( -125.6228709571500275, -23.84081130438200802, 10.88220057463249191 ) ) ;
#21546 = CARTESIAN_POINT ( 'NONE',  ( -1.540913562699879114, -6.376774720514410077, 19.44316438561912008 ) ) ;
#21547 = CARTESIAN_POINT ( 'NONE',  ( 10.45329875151443488, -17.81600612866554556, 11.49999999999999645 ) ) ;
#21548 = CARTESIAN_POINT ( 'NONE',  ( -128.5895376238167103, -24.64965694238408034, 8.947790433994645909 ) ) ;
#21549 = CARTESIAN_POINT ( 'NONE',  ( -97.52287095715006160, -24.64965694238575011, 8.947790433994194714 ) ) ;
#21550 = APPROVAL ( #5935, 'UNSPECIFIED' ) ;
#21551 = CARTESIAN_POINT ( 'NONE',  ( -106.6344508903434019, -23.48783264082477729, -1.443836473390085695 ) ) ;
#21552 = CARTESIAN_POINT ( 'NONE',  ( -4.086358941109507370, -22.34742993483353146, 11.49999999999999645 ) ) ;
#21553 = VERTEX_POINT ( 'NONE', #79880 ) ;
#21554 = DIRECTION ( 'NONE',  ( 0.1478094111296165969, -0.9890158633619159367, 0.000000000000000000 ) ) ;
#21555 = CARTESIAN_POINT ( 'NONE',  ( 25.05730599792489599, -2.682774720540237468, -18.59674224247002172 ) ) ;
#21556 = CARTESIAN_POINT ( 'NONE',  ( 0.4983251850863967269, 20.17815531296474418, -1.500000000000002220 ) ) ;
#21557 = CARTESIAN_POINT ( 'NONE',  ( -115.6228709571500559, -29.50250243563736774, 8.947779886222134493 ) ) ;
#21558 = CARTESIAN_POINT ( 'NONE',  ( -52.52287095715006870, -24.64965694238574656, 8.947790433994203596 ) ) ;
#21559 = EDGE_CURVE ( 'NONE', #71622, #64237, #74198, .T. ) ;
#21560 = ORIENTED_EDGE ( 'NONE', *, *, #65875, .T. ) ;
#21561 = VERTEX_POINT ( 'NONE', #10373 ) ;
#21562 = DIRECTION ( 'NONE',  ( 0.000000000000000000, 0.000000000000000000, 1.000000000000000000 ) ) ;
#21563 = CARTESIAN_POINT ( 'NONE',  ( 19.82229641098322404, 11.46754112681587046, -1.500000000000002220 ) ) ;
#21564 = CARTESIAN_POINT ( 'NONE',  ( -29.53721135371585760, -24.26652312753709140, 0.1864212292069160337 ) ) ;
#21565 = CARTESIAN_POINT ( 'NONE',  ( -14.38888013576714719, -16.06800976983558726, -1.500000000000002220 ) ) ;
#21566 = FACE_OUTER_BOUND ( 'NONE', #77739, .T. ) ;
#21567 = CARTESIAN_POINT ( 'NONE',  ( -127.6234793054417338, -24.66019654487200441, 8.947790411086106843 ) ) ;
#21568 = APPROVAL_PERSON_ORGANIZATION ( #18562, #36350, #79464 ) ;
#21569 = CARTESIAN_POINT ( 'NONE',  ( 11.28189403632909915, 17.58240144430209995, 11.49999999999999645 ) ) ;
#21570 = ORIENTED_EDGE ( 'NONE', *, *, #12213, .T. ) ;
#21571 = CARTESIAN_POINT ( 'NONE',  ( -69.87926231432713564, -25.24754257055753115, 4.903253054825144730 ) ) ;
#21572 = CARTESIAN_POINT ( 'NONE',  ( 5.346615758220810477, 21.33151429383102382, -1.500000000000002220 ) ) ;
#21573 = LINE ( 'NONE', #53556, #17122 ) ;
#21574 = CARTESIAN_POINT ( 'NONE',  ( -28.74184145762639631, -24.79700204495068760, 7.085838617364061065 ) ) ;
#21575 = AXIS2_PLACEMENT_3D ( 'NONE', #25556, #40779, #71741 ) ;
#21576 = VERTEX_POINT ( 'NONE', #26608 ) ;
#21577 = CARTESIAN_POINT ( 'NONE',  ( 4.190829928318763109, -6.376774720514401196, 18.23548058298382557 ) ) ;
#21578 = CARTESIAN_POINT ( 'NONE',  ( -96.62287095715005592, -24.64965695001468404, 8.947790433994178727 ) ) ;
#21579 = VERTEX_POINT ( 'NONE', #81390 ) ;
#21580 = CARTESIAN_POINT ( 'NONE',  ( -72.56475950965167954, -23.48786465467241058, 11.44779295918254824 ) ) ;
#21581 = VERTEX_POINT ( 'NONE', #2780 ) ;
#21582 = AXIS2_PLACEMENT_3D ( 'NONE', #7540, #92765, #23251 ) ;
#21583 = ORIENTED_EDGE ( 'NONE', *, *, #54719, .F. ) ;
#21584 = EDGE_CURVE ( 'NONE', #88881, #62896, #88007, .T. ) ;
#21585 = CARTESIAN_POINT ( 'NONE',  ( -71.63071712269331215, -24.35071581493543391, 9.817618358456021710 ) ) ;
#21586 = LINE ( 'NONE', #19599, #45413 ) ;
#21587 = CARTESIAN_POINT ( 'NONE',  ( -57.50308292730503723, -24.15543982623907127, -0.2315651400026663420 ) ) ;
#21588 = CARTESIAN_POINT ( 'NONE',  ( 18.16468007720714795, -9.286844270591712913, -1.500000000000002220 ) ) ;
#21589 = ORIENTED_EDGE ( 'NONE', *, *, #39354, .F. ) ;
#21590 = CARTESIAN_POINT ( 'NONE',  ( -0.7827064370038755436, -5.876774720514410966, 19.55912026249540148 ) ) ;
#21591 = CARTESIAN_POINT ( 'NONE',  ( -99.52287095715009002, -24.66019654487200441, 8.947790411086119278 ) ) ;
#21592 = CARTESIAN_POINT ( 'NONE',  ( -97.52287095715006160, -29.50247984919015209, -1.443849546365050029 ) ) ;
#21593 = CARTESIAN_POINT ( 'NONE',  ( -91.52287095715009002, -23.72747288104470087, -1.053458166803225904 ) ) ;
#21594 = EDGE_LOOP ( 'NONE', ( #98640, #53409, #17333 ) ) ;
#21595 = CARTESIAN_POINT ( 'NONE',  ( -8.160000000000000142, -9.652339641703484574, -1.621096496867199033 ) ) ;
#21596 = CARTESIAN_POINT ( 'NONE',  ( -28.90723246652128609, -24.63645969467739150, 7.813650128146762519 ) ) ;
#21597 = B_SPLINE_CURVE_WITH_KNOTS ( 'NONE', 3,
 ( #35931, #37928, #7972, #23689, #868, #100296 ),
 .UNSPECIFIED., .F., .F.,
 ( 4, 2, 4 ),
 ( 0.000000000000000000, 0.001380764517854763014, 0.002761529035709526028 ),
 .UNSPECIFIED. ) ;
#21598 = CARTESIAN_POINT ( 'NONE',  ( 15.20108283357335921, -14.20388156210760577, -1.500000000000002220 ) ) ;
#21599 = EDGE_CURVE ( 'NONE', #13237, #60950, #25091, .T. ) ;
#21600 = VERTEX_POINT ( 'NONE', #80890 ) ;
#21602 = ORIENTED_EDGE ( 'NONE', *, *, #61490, .F. ) ;
#21601 = CARTESIAN_POINT ( 'NONE',  ( 4.017909867803298063, -6.376774720514402972, 18.55402206357357286 ) ) ;
#21603 = B_SPLINE_CURVE_WITH_KNOTS ( 'NONE', 3,
 ( #7220, #64441, #30565, #79624 ),
 .UNSPECIFIED., .F., .F.,
 ( 4, 4 ),
 ( 0.000000000000000000, 9.999999999998897304E-05 ),
 .UNSPECIFIED. ) ;
#21604 = B_SPLINE_SURFACE_WITH_KNOTS ( 'NONE', 3, 1, ( 
 ( #65706, #71300 ),
 ( #18004, #95633 ),
 ( #48467, #49976 ),
 ( #80903, #2295 ),
 ( #33733, #26624 ),
 ( #40345, #1786 ),
 ( #32725, #96137 ),
 ( #79896, #63708 ),
 ( #65213, #94624 ),
 ( #10389, #73301 ),
 ( #41347, #79397 ),
 ( #57585, #64715 ),
 ( #9887, #72300 ),
 ( #25105, #33225 ),
 ( #3795, #64206 ) ),
 .UNSPECIFIED., .F., .F., .F.,
 ( 4, 1, 1, 1, 1, 1, 1, 1, 1, 1, 1, 1, 4 ),
 ( 2, 2 ),
 ( 0.000000000000000000, 0.08594794314412776415, 0.1691252118806905458, 0.2503991071860499074, 0.3322897361388365001, 0.4133642879158791472, 0.4941722833711859053, 0.5760217353866371459, 0.6607569692540058437, 0.7457831259137418511, 0.8300435929752247866, 0.9140275458206815751, 1.000000000000000000 ),
 ( 0.000000000000000000, 1.000000000000000000 ),
 .UNSPECIFIED. ) ;
#21605 = CARTESIAN_POINT ( 'NONE',  ( -98.62287095715005592, -23.48783264082478439, -1.443836473390061936 ) ) ;
#21606 = ORIENTED_EDGE ( 'NONE', *, *, #33610, .T. ) ;
#21607 = ORIENTED_EDGE ( 'NONE', *, *, #72131, .T. ) ;
#21608 = CARTESIAN_POINT ( 'NONE',  ( 29.73860345376319358, 1.682774720514426114, 3.721136469884293236E-15 ) ) ;
#21609 = CARTESIAN_POINT ( 'NONE',  ( -55.52287095715005449, -23.48783264082477018, -1.443836473390094577 ) ) ;
#21610 = DIRECTION ( 'NONE',  ( -3.773278334453079030E-23, 0.9999999999976377785, 2.173523156925979128E-06 ) ) ;
#21611 = CARTESIAN_POINT ( 'NONE',  ( -105.6228709571500559, -29.50248528299804818, 1.056150453629043584 ) ) ;
#21613 = ORIENTED_EDGE ( 'NONE', *, *, #61338, .F. ) ;
#21612 = CARTESIAN_POINT ( 'NONE',  ( 6.025212951983072607, -21.27585971943098642, 11.49999999999999645 ) ) ;
#21614 = EDGE_CURVE ( 'NONE', #29436, #56695, #11376, .T. ) ;
#21615 = CARTESIAN_POINT ( 'NONE',  ( -72.62287095715004170, -23.73907113216991860, -1.053371485793228146 ) ) ;
#21616 = VECTOR ( 'NONE', #28009, 1000.000000000000000 ) ;
#21617 = CARTESIAN_POINT ( 'NONE',  ( -20.48750165597241590, 9.616757810196778777, -1.500000000000002220 ) ) ;
#21619 = VERTEX_POINT ( 'NONE', #75751 ) ;
#21618 = CARTESIAN_POINT ( 'NONE',  ( -124.5228709571500616, -23.47593901973090524, -1.443836447538996204 ) ) ;
#21620 = B_SPLINE_CURVE_WITH_KNOTS ( 'NONE', 3,
 ( #90316, #7074, #53263, #52261 ),
 .UNSPECIFIED., .F., .F.,
 ( 4, 4 ),
 ( 0.000000000000000000, 9.999999999998897304E-05 ),
 .UNSPECIFIED. ) ;
#21621 = AXIS2_PLACEMENT_3D ( 'NONE', #40448, #55182, #63297 ) ;
#21622 = VERTEX_POINT ( 'NONE', #21958 ) ;
#21623 = CARTESIAN_POINT ( 'NONE',  ( -10.15655021453082263, -4.851073166933324465, 30.10912256999369774 ) ) ;
#21624 = CARTESIAN_POINT ( 'NONE',  ( -15.79248070760165490, 12.47733877207048181, 11.49999999999998934 ) ) ;
#21625 = DIRECTION ( 'NONE',  ( -0.000000000000000000, 1.000000000000000000, -0.000000000000000000 ) ) ;
#21626 = ORIENTED_EDGE ( 'NONE', *, *, #66305, .T. ) ;
#21627 = DIRECTION ( 'NONE',  ( 0.000000000000000000, 0.000000000000000000, 1.000000000000000000 ) ) ;
#21628 = CARTESIAN_POINT ( 'NONE',  ( 13.15158565771796084, -18.08388448789661851, -1.500000000000002220 ) ) ;
#21629 = EDGE_LOOP ( 'NONE', ( #92238, #88940, #65850, #60272 ) ) ;
#21630 = VERTEX_POINT ( 'NONE', #12859 ) ;
#21631 = DIRECTION ( 'NONE',  ( -3.773278334453079030E-23, 0.9999999999976377785, 2.173523156925979128E-06 ) ) ;
#21632 = DIRECTION ( 'NONE',  ( 0.000000000000000000, -0.9999999999976377785, -2.173523156925979128E-06 ) ) ;
#21633 = DIRECTION ( 'NONE',  ( 8.334928612639484546E-17, 1.000000000000000000, 7.321843366904296032E-17 ) ) ;
#21634 = LINE ( 'NONE', #95908, #67654 ) ;
#21635 = DIRECTION ( 'NONE',  ( 3.773278334444166432E-23, -1.000000000000000000, 0.000000000000000000 ) ) ;
#21636 = CARTESIAN_POINT ( 'NONE',  ( 7.694069055508638399, 17.95645395709951941, -1.500000000000002220 ) ) ;
#21637 = FACE_OUTER_BOUND ( 'NONE', #40453, .T. ) ;
#21638 = CARTESIAN_POINT ( 'NONE',  ( -13.16228656746626591, 16.97819584282690286, 11.49999999999998934 ) ) ;
#21639 = CARTESIAN_POINT ( 'NONE',  ( -2.220741593810419801, -6.376774720514411854, 19.46247113826587238 ) ) ;
#21640 = DIRECTION ( 'NONE',  ( 1.000000000000000000, 3.773278334444166432E-23, 8.201307841325785021E-29 ) ) ;
#21641 = CARTESIAN_POINT ( 'NONE',  ( -34.52287095715006160, -24.50216790748203266, 0.6166512839542475088 ) ) ;
#21642 = CARTESIAN_POINT ( 'NONE',  ( 20.43669262517703800, -10.12641136740851699, -1.500000000000002220 ) ) ;
#21643 = AXIS2_PLACEMENT_3D ( 'NONE', #91300, #76554, #37016 ) ;
#21644 = EDGE_CURVE ( 'NONE', #61677, #80660, #21460, .T. ) ;
#21645 = PERSON_AND_ORGANIZATION ( #70597, #27821 ) ;
#21646 = DIRECTION ( 'NONE',  ( -3.773278334453079618E-23, 0.9999999999976377785, 2.173523156925979975E-06 ) ) ;
#21647 = CARTESIAN_POINT ( 'NONE',  ( -32.30247028140506416, -5.965225279485572685, 27.60502002861223048 ) ) ;
#21648 = CARTESIAN_POINT ( 'NONE',  ( 8.914523860536577970, -17.85282776015759154, 11.49999999999999645 ) ) ;
#21649 = DIRECTION ( 'NONE',  ( 1.000000000000000000, 3.773278334444167608E-23, 8.201307833595939069E-29 ) ) ;
#21650 = VECTOR ( 'NONE', #13419, 1000.000000000000000 ) ;
#21651 = CARTESIAN_POINT ( 'NONE',  ( -39.61746832362916848, -23.48786465467240703, 11.44779295918255002 ) ) ;
#21652 = CARTESIAN_POINT ( 'NONE',  ( -108.6228709571500701, -24.33832256526968862, 0.1851278514119918950 ) ) ;
#21653 = ORIENTED_EDGE ( 'NONE', *, *, #82442, .T. ) ;
#21654 = CARTESIAN_POINT ( 'NONE',  ( -4.141025641025638748, -5.876774720514426953, 21.75000000000000355 ) ) ;
#21655 = CARTESIAN_POINT ( 'NONE',  ( -70.58953762381671027, -23.48786465467241058, 11.44779295918254469 ) ) ;
#21656 = CARTESIAN_POINT ( 'NONE',  ( -20.31635052000798325, -7.690577546848336610, 11.49999999999998934 ) ) ;
#21657 = CARTESIAN_POINT ( 'NONE',  ( -66.52287095715006160, -23.47596703998600631, 11.44779298504228748 ) ) ;
#21658 = CARTESIAN_POINT ( 'NONE',  ( -14.21210043416151159, 13.53504130633199765, -1.500000000000002220 ) ) ;
#21659 = CARTESIAN_POINT ( 'NONE',  ( -100.4426124108961176, -25.13313949306887451, 7.101635536975466678 ) ) ;
#21660 = ORIENTED_EDGE ( 'NONE', *, *, #86831, .F. ) ;
#21661 = CONTEXT_DEPENDENT_SHAPE_REPRESENTATION ( #14819, #90395 ) ;
#21662 = CARTESIAN_POINT ( 'NONE',  ( 7.462166178408539352, -6.475225279485573360, -27.67315496249664974 ) ) ;
#21663 = LINE ( 'NONE', #68365, #67004 ) ;
#21664 = CARTESIAN_POINT ( 'NONE',  ( 20.39306652673287701, -2.074774109220689500, 11.49999999999999645 ) ) ;
#21665 = CARTESIAN_POINT ( 'NONE',  ( 28.30015606816038698, 1.477225279485574028, -13.13501953239208930 ) ) ;
#21666 = CARTESIAN_POINT ( 'NONE',  ( -93.55620429048337883, -23.48783264082478084, -1.443836473390063713 ) ) ;
#21667 = ADVANCED_FACE ( 'NONE', ( #60062 ), #14352, .F. ) ;
#21668 = VERTEX_POINT ( 'NONE', #74275 ) ;
#21669 = CARTESIAN_POINT ( 'NONE',  ( -62.52287095715006160, -24.50321055353804311, 9.387540953477525818 ) ) ;
#21670 = DIRECTION ( 'NONE',  ( 0.000000000000000000, 0.000000000000000000, 1.000000000000000000 ) ) ;
#21671 = EDGE_CURVE ( 'NONE', #22324, #35733, #81887, .T. ) ;
#21672 = CARTESIAN_POINT ( 'NONE',  ( 11.62916340711181284, 0.3587747205144265483, 28.75961759920349792 ) ) ;
#21673 = CARTESIAN_POINT ( 'NONE',  ( -123.5228709571500616, -24.64965694238408034, 8.947790433994191162 ) ) ;
#21674 = VECTOR ( 'NONE', #63925, 1000.000000000000000 ) ;
#21675 = EDGE_LOOP ( 'NONE', ( #83768, #12504, #88921, #22086 ) ) ;
#21676 = CARTESIAN_POINT ( 'NONE',  ( 32.68381218857752657, 4.917472161913310380, -3.063707678755810182 ) ) ;
#21677 = ADVANCED_FACE ( 'NONE', ( #45330 ), #12363, .T. ) ;
#21678 = EDGE_CURVE ( 'NONE', #75171, #81379, #27610, .T. ) ;
#21679 = CARTESIAN_POINT ( 'NONE',  ( -14.75821945985506645, 17.75411527500383002, 11.49999999999999645 ) ) ;
#21680 = CARTESIAN_POINT ( 'NONE',  ( -20.44213351528904354, 10.05872170072450977, 11.49999999999998934 ) ) ;
#21681 = CARTESIAN_POINT ( 'NONE',  ( -34.22287095715006444, -23.47596703998600276, 11.44779298504227683 ) ) ;
#21682 = CIRCLE ( 'NONE', #65488, 1.149999999999998135 ) ;
#21683 = CARTESIAN_POINT ( 'NONE',  ( -105.6228709571500417, -24.62226745350444546, 0.9660975649729522940 ) ) ;
#21684 = DIRECTION ( 'NONE',  ( 0.000000000000000000, 0.5747471426738535172, 0.8183310589170139648 ) ) ;
#21685 = ADVANCED_FACE ( 'NONE', ( #74762 ), #68161, .T. ) ;
#21686 = CARTESIAN_POINT ( 'NONE',  ( -115.5228709571500474, -24.52232992886360563, 0.6492154411906000400 ) ) ;
#21687 = CARTESIAN_POINT ( 'NONE',  ( -99.64934318012689118, -25.30157686769864966, 4.927356324713951352 ) ) ;
#21688 = B_SPLINE_CURVE_WITH_KNOTS ( 'NONE', 3,
 ( #5431, #83547, #20647, #22136 ),
 .UNSPECIFIED., .F., .F.,
 ( 4, 4 ),
 ( 0.007875538328797549587, 0.009214210883376282302 ),
 .UNSPECIFIED. ) ;
#21689 = CARTESIAN_POINT ( 'NONE',  ( 21.88901064076550185, 0.7357440816682787599, 11.49999999999998934 ) ) ;
#21690 = LINE ( 'NONE', #52661, #20293 ) ;
#21691 = CARTESIAN_POINT ( 'NONE',  ( -87.54287233632688014, -24.66019654487200441, 8.947790411086112172 ) ) ;
#21692 = DIRECTION ( 'NONE',  ( 0.000000000000000000, 0.9999999999976377785, 2.173523156925979128E-06 ) ) ;
#21693 = CARTESIAN_POINT ( 'NONE',  ( -125.5562042904833930, -24.99156044556202261, 7.747789690856173195 ) ) ;
#21694 = CARTESIAN_POINT ( 'NONE',  ( -61.64687923781919920, -29.50249039766296022, 3.409318347773680369 ) ) ;
#21695 = CARTESIAN_POINT ( 'NONE',  ( -4.465079497292244959, -5.876774720514410077, 19.29815762497054976 ) ) ;
#21696 = EDGE_LOOP ( 'NONE', ( #21244, #31954, #6149, #28236 ) ) ;
#21697 = CARTESIAN_POINT ( 'NONE',  ( 13.86372479123709311, 15.02075200336711092, -1.500000000000002220 ) ) ;
#21698 = ORIENTED_EDGE ( 'NONE', *, *, #38540, .F. ) ;
#21699 = ORIENTED_EDGE ( 'NONE', *, *, #44468, .T. ) ;
#21700 = VERTEX_POINT ( 'NONE', #67179 ) ;
#21701 = ORIENTED_EDGE ( 'NONE', *, *, #40871, .T. ) ;
#21702 = EDGE_CURVE ( 'NONE', #75490, #38526, #37253, .T. ) ;
#21703 = CARTESIAN_POINT ( 'NONE',  ( 17.08057647167376913, 15.47633299359885761, 11.49999999999998934 ) ) ;
#21704 = CARTESIAN_POINT ( 'NONE',  ( -35.52287095715006160, -24.63287334234369297, 0.9662140553102194218 ) ) ;
#21705 = CARTESIAN_POINT ( 'NONE',  ( -18.67835518149133378, -7.740158416121700746, -1.500000000000002220 ) ) ;
#21706 = ORIENTED_EDGE ( 'NONE', *, *, #80237, .F. ) ;
#21707 = CARTESIAN_POINT ( 'NONE',  ( -54.62287095715005592, -24.64965695001467694, 8.947790433994185832 ) ) ;
#21708 = CARTESIAN_POINT ( 'NONE',  ( -40.49165087243459737, -25.30353303947430987, 5.543942858925161588 ) ) ;
#21709 = CARTESIAN_POINT ( 'NONE',  ( -127.9228709571500815, -23.47596703998600631, 11.44779298504227860 ) ) ;
#21710 = CARTESIAN_POINT ( 'NONE',  ( -99.58876850471365572, -24.35071581493543391, 9.817618358456025263 ) ) ;
#21712 = ORIENTED_EDGE ( 'NONE', *, *, #29854, .F. ) ;
#21711 = CARTESIAN_POINT ( 'NONE',  ( 18.57079561221590325, -10.74342183689097574, 11.49999999999999645 ) ) ;
#21713 = FACE_OUTER_BOUND ( 'NONE', #38309, .T. ) ;
#21714 = DIRECTION ( 'NONE',  ( -0.000000000000000000, 1.000000000000000000, -0.000000000000000000 ) ) ;
#21715 = VERTEX_POINT ( 'NONE', #97113 ) ;
#21716 = CARTESIAN_POINT ( 'NONE',  ( -20.61657899823519813, -2.091364977790679980, 11.49999999999998934 ) ) ;
#21717 = EDGE_CURVE ( 'NONE', #38068, #41731, #28104, .T. ) ;
#21719 = ORIENTED_EDGE ( 'NONE', *, *, #33179, .F. ) ;
#21718 = CARTESIAN_POINT ( 'NONE',  ( -19.77875734969026311, 5.356774720514425603, 0.7300228001186309656 ) ) ;
#21720 = EDGE_CURVE ( 'NONE', #42461, #55826, #99087, .T. ) ;
#21721 = CARTESIAN_POINT ( 'NONE',  ( -28.50260975624814819, -23.79695530739836329, -0.6495505116914124244 ) ) ;
#21722 = ORIENTED_EDGE ( 'NONE', *, *, #57736, .T. ) ;
#21723 = CARTESIAN_POINT ( 'NONE',  ( 4.856316114246853388, -6.376774720514408301, 19.03119074624055074 ) ) ;
#21724 = ORIENTED_EDGE ( 'NONE', *, *, #29482, .T. ) ;
#21725 = CARTESIAN_POINT ( 'NONE',  ( 10.18035917307295435, 18.35650967997132099, -1.500000000000002220 ) ) ;
#21726 = B_SPLINE_CURVE_WITH_KNOTS ( 'NONE', 3,
 ( #100003, #53867, #59479, #52863, #92407, #77175, #69078, #36631 ),
 .UNSPECIFIED., .F., .F.,
 ( 4, 2, 2, 4 ),
 ( 0.000000000000000000, 0.002001079623178224527, 0.003001619434767338526, 0.004002159246356452524 ),
 .UNSPECIFIED. ) ;
#21727 = CARTESIAN_POINT ( 'NONE',  ( -12.87221125579857528, -17.80329210173279364, 11.49999999999999645 ) ) ;
#21728 = ADVANCED_FACE ( 'NONE', ( #6747 ), #36709, .T. ) ;
#21729 = CARTESIAN_POINT ( 'NONE',  ( -37.57567300276403444, -24.66019654487199730, 8.947790411086113949 ) ) ;
#21730 = CARTESIAN_POINT ( 'NONE',  ( 21.27769986149581172, 7.469961712261545372, -1.500000000000002220 ) ) ;
#21731 = CARTESIAN_POINT ( 'NONE',  ( -20.39251343623233836, 4.912230638944180328, -1.500000000000002220 ) ) ;
#21732 = EDGE_CURVE ( 'NONE', #62904, #59914, #66693, .T. ) ;
#21733 = FACE_OUTER_BOUND ( 'NONE', #12511, .T. ) ;
#21734 = DIRECTION ( 'NONE',  ( -0.000000000000000000, 1.000000000000000000, -0.000000000000000000 ) ) ;
#21735 = CARTESIAN_POINT ( 'NONE',  ( 0.000000000000000000, 7.470345474798854293E-16, -6.099999999999999645 ) ) ;
#21736 = VERTEX_POINT ( 'NONE', #20472 ) ;
#21737 = EDGE_CURVE ( 'NONE', #79503, #45193, #58808, .T. ) ;
#21738 = ORIENTED_EDGE ( 'NONE', *, *, #37579, .T. ) ;
#21739 = ORIENTED_EDGE ( 'NONE', *, *, #20116, .T. ) ;
#21740 = CYLINDRICAL_SURFACE ( 'NONE', #51493, 2.399999999999999911 ) ;
#21741 = VECTOR ( 'NONE', #100136, 1000.000000000000114 ) ;
#21742 = CARTESIAN_POINT ( 'NONE',  ( -19.93307770644097232, -8.117153041090405807, -1.500000000000002220 ) ) ;
#21743 = CARTESIAN_POINT ( 'NONE',  ( 5.271800844963591359, 0.3587747205143965168, -28.56638892015329745 ) ) ;
#21744 = VERTEX_POINT ( 'NONE', #20970 ) ;
#21745 = CARTESIAN_POINT ( 'NONE',  ( 14.88031740681034698, -14.96734982212533183, 11.49999999999998934 ) ) ;
#21746 = DIRECTION ( 'NONE',  ( -0.6599726524652352877, 0.000000000000000000, 0.7512896232465889890 ) ) ;
#21747 = LINE ( 'NONE', #45118, #5971 ) ;
#21748 = CARTESIAN_POINT ( 'NONE',  ( -35.62287095715005592, -24.99132157543083821, 2.256160258750667502 ) ) ;
#21749 = DIRECTION ( 'NONE',  ( 0.000000000000000000, 0.000000000000000000, 1.000000000000000000 ) ) ;
#21750 = DIRECTION ( 'NONE',  ( -3.773278334453080206E-23, 0.9999999999976377785, 2.173523156925979975E-06 ) ) ;
#21751 = CARTESIAN_POINT ( 'NONE',  ( -19.90388773112789167, 9.559999800501117306, -1.500000000000002220 ) ) ;
#21752 = LINE ( 'NONE', #67456, #19261 ) ;
#21753 = VECTOR ( 'NONE', #48587, 1000.000000000000000 ) ;
#21754 = ORIENTED_EDGE ( 'NONE', *, *, #84391, .F. ) ;
#21755 = DIRECTION ( 'NONE',  ( 0.000000000000000000, 1.000000000000000000, 0.000000000000000000 ) ) ;
#21756 = CARTESIAN_POINT ( 'NONE',  ( 12.78578435864683449, 3.995361385602315796, -28.02483137475221397 ) ) ;
#21757 = LINE ( 'NONE', #84165, #72809 ) ;
#21758 = CARTESIAN_POINT ( 'NONE',  ( -62.52208505296627550, -23.48786465467241058, 11.44779295918255002 ) ) ;
#21759 = CARTESIAN_POINT ( 'NONE',  ( -7.499459838998954631, -17.95702976299720532, 11.49999999999998934 ) ) ;
#21760 = CARTESIAN_POINT ( 'NONE',  ( -19.64189229742525455, -8.423329616690555355, 11.49999999999998934 ) ) ;
#21761 = CARTESIAN_POINT ( 'NONE',  ( -70.16128103861791487, -25.04479545170914179, 7.555221618711828846 ) ) ;
#21762 = CYLINDRICAL_SURFACE ( 'NONE', #44728, 4.299999999999999822 ) ;
#21763 = CARTESIAN_POINT ( 'NONE',  ( 0.000000000000000000, -4.056774720514426669, 0.000000000000000000 ) ) ;
#21764 = CARTESIAN_POINT ( 'NONE',  ( -36.62287095715007723, -24.51387760970723662, 9.387446482453421837 ) ) ;
#21765 = CARTESIAN_POINT ( 'NONE',  ( -11.86362535333686807, -19.25999739251378173, -1.500000000000002220 ) ) ;
#21766 = B_SPLINE_CURVE_WITH_KNOTS ( 'NONE', 3,
 ( #43866, #4806, #51479, #35759 ),
 .UNSPECIFIED., .F., .F.,
 ( 4, 4 ),
 ( 0.5591709285427831633, 0.5601716755835483008 ),
 .UNSPECIFIED. ) ;
#21767 = VERTEX_POINT ( 'NONE', #51941 ) ;
#21768 = CARTESIAN_POINT ( 'NONE',  ( -10.21384395349166496, 6.475225279485573360, 29.49402280011861777 ) ) ;
#21769 = DIRECTION ( 'NONE',  ( 0.8898870177566430284, -9.915199454925210578E-07, 0.4561809899888475961 ) ) ;
#21770 = CARTESIAN_POINT ( 'NONE',  ( 6.953341435731974940, 18.52374150113109152, 11.49999999999999645 ) ) ;
#21771 = CARTESIAN_POINT ( 'NONE',  ( -76.58953762381673869, -23.48783264082478084, -1.443836473390065489 ) ) ;
#21772 = ORIENTED_EDGE ( 'NONE', *, *, #17582, .F. ) ;
#21773 = B_SPLINE_CURVE_WITH_KNOTS ( 'NONE', 3,
 ( #85285, #8169, #9673, #56370, #85796, #94403, #94902, #62462 ),
 .UNSPECIFIED., .F., .F.,
 ( 4, 2, 2, 4 ),
 ( -0.001240355328176767288, -0.0002398155169398778330, 0.0007607242942970116224, 0.002761803916770795737 ),
 .UNSPECIFIED. ) ;
#21774 = CARTESIAN_POINT ( 'NONE',  ( -66.55620429048340725, -24.64898659630528854, 1.056161002820824368 ) ) ;
#21775 = CARTESIAN_POINT ( 'NONE',  ( -115.5228709571500616, -25.00158670708909625, 2.256160236439166411 ) ) ;
#21776 = CARTESIAN_POINT ( 'NONE',  ( -0.6006773669993965559, 21.62980403441659760, 11.49999999999998934 ) ) ;
#21777 = LINE ( 'NONE', #90313, #1031 ) ;
#21778 = CARTESIAN_POINT ( 'NONE',  ( 8.513215801882951794, -17.43586836189350819, -1.500000000000002220 ) ) ;
#21779 = CARTESIAN_POINT ( 'NONE',  ( -7.160000000000000142, 7.891155995661682354, 5.788828319098143993 ) ) ;
#21780 = CARTESIAN_POINT ( 'NONE',  ( -35.62287095715006302, -24.92579138211019085, 1.929029949965666013 ) ) ;
#21781 = CARTESIAN_POINT ( 'NONE',  ( 18.46520180437041603, 7.126043738416648843, -1.500000000000002220 ) ) ;
#21782 = ORIENTED_EDGE ( 'NONE', *, *, #72066, .F. ) ;
#21783 = VECTOR ( 'NONE', #9068, 1000.000000000000114 ) ;
#21784 = CARTESIAN_POINT ( 'NONE',  ( 6.844040470191356640, -19.11863935190610064, 11.49999999999999645 ) ) ;
#21785 = DIRECTION ( 'NONE',  ( 0.000000000000000000, 0.000000000000000000, -1.000000000000000000 ) ) ;
#21786 = B_SPLINE_CURVE_WITH_KNOTS ( 'NONE', 3,
 ( #89336, #74597, #5088, #36533, #82709, #36039 ),
 .UNSPECIFIED., .F., .F.,
 ( 4, 2, 4 ),
 ( 1.570755371633993761E-05, 0.001396183895866087753, 0.002776660238015835579 ),
 .UNSPECIFIED. ) ;
#21787 = CARTESIAN_POINT ( 'NONE',  ( 33.63416148851499088, -3.931067265920685561, -11.97433369283768734 ) ) ;
#21788 = ADVANCED_FACE ( 'NONE', ( #44333 ), #98595, .F. ) ;
#21789 = ORIENTED_EDGE ( 'NONE', *, *, #40097, .T. ) ;
#21790 = B_SPLINE_SURFACE_WITH_KNOTS ( 'NONE', 3, 3, ( 
 ( #41127, #41632, #72574, #19267 ),
 ( #10670, #94399, #48237, #79168 ),
 ( #11655, #64487, #34009, #25891 ),
 ( #94895, #25387, #80676, #56364 ),
 ( #3564, #87795, #34510, #65482 ),
 ( #88802, #98382, #97882, #27886 ),
 ( #52230, #50735, #36491, #74070 ) ),
 .UNSPECIFIED., .F., .F., .F.,
 ( 4, 3, 4 ),
 ( 4, 4 ),
 ( 0.0004766839783845224225, 0.1029713700210912741, 0.2054660560637980304 ),
 ( 0.1395294911668197024, 0.1406065943737035973 ),
 .UNSPECIFIED. ) ;
#21791 = CARTESIAN_POINT ( 'NONE',  ( -102.5909799838791088, -24.15620529776628445, 10.23563542870660292 ) ) ;
#21792 = CARTESIAN_POINT ( 'NONE',  ( -63.62287095715004881, -29.50250243563736774, 8.947779886222145151 ) ) ;
#21793 = PLANE ( 'NONE',  #71029 ) ;
#21794 = EDGE_CURVE ( 'NONE', #97387, #60884, #93982, .T. ) ;
#21795 = CARTESIAN_POINT ( 'NONE',  ( 12.92500000000000426, 0.000000000000000000, 0.000000000000000000 ) ) ;
#21796 = CARTESIAN_POINT ( 'NONE',  ( -50.47238528336495733, -25.12325454535568880, 7.100110082141690704 ) ) ;
#21797 = CARTESIAN_POINT ( 'NONE',  ( -18.39468835979788608, -8.022455445098881199, -1.500000000000002220 ) ) ;
#21798 = EDGE_CURVE ( 'NONE', #30073, #31528, #53442, .T. ) ;
#21799 = CARTESIAN_POINT ( 'NONE',  ( -1.140932434931746582E-13, -6.376774720514426953, 21.78128695274321203 ) ) ;
#21800 = ORIENTED_EDGE ( 'NONE', *, *, #88846, .T. ) ;
#21801 = CARTESIAN_POINT ( 'NONE',  ( -72.55620429048340725, -24.64898659630528854, 1.056161002820823036 ) ) ;
#21802 = EDGE_CURVE ( 'NONE', #8909, #12190, #44251, .T. ) ;
#21803 = ADVANCED_FACE ( 'NONE', ( #31079 ), #77243, .F. ) ;
#21804 = CARTESIAN_POINT ( 'NONE',  ( -10.82450569625279613, 20.10975305113172951, 11.49999999999999645 ) ) ;
#21805 = CARTESIAN_POINT ( 'NONE',  ( -50.16163650206989644, -25.31297212321189605, 4.712129047060907183 ) ) ;
#21806 = CARTESIAN_POINT ( 'NONE',  ( -86.62287095715004170, -24.64898659630528854, 1.056161002820827921 ) ) ;
#21807 = CARTESIAN_POINT ( 'NONE',  ( -114.5562042904833788, -24.65952944569305316, 1.056160979905703234 ) ) ;
#21808 = EDGE_CURVE ( 'NONE', #76224, #58188, #4362, .T. ) ;
#21809 = CARTESIAN_POINT ( 'NONE',  ( 5.654014271574485662, -5.876774720514419847, 20.92503208403226722 ) ) ;
#21810 = AXIS2_PLACEMENT_3D ( 'NONE', #14703, #30933, #53787 ) ;
#21811 = CARTESIAN_POINT ( 'NONE',  ( 33.74124265030975067, -3.622774720514426949, -12.32597719988138252 ) ) ;
#21812 = DIRECTION ( 'NONE',  ( -3.773278334453079030E-23, 0.9999999999976377785, 2.173523156925979128E-06 ) ) ;
#21813 = ORIENTED_EDGE ( 'NONE', *, *, #94312, .T. ) ;
#21814 = CARTESIAN_POINT ( 'NONE',  ( -20.15914900662387055, -2.930279687489938389, 11.49999999999998934 ) ) ;
#21815 = ORIENTED_EDGE ( 'NONE', *, *, #19698, .F. ) ;
#21816 = ADVANCED_FACE ( 'NONE', ( #8256 ), #15352, .F. ) ;
#21817 = CARTESIAN_POINT ( 'NONE',  ( 7.334040449947802465, -21.76207178258647090, 11.49999999999998934 ) ) ;
#21818 = CARTESIAN_POINT ( 'NONE',  ( -37.62287095715006302, -24.65952944569304250, 1.056160979905693020 ) ) ;
#21819 = AXIS2_PLACEMENT_3D ( 'NONE', #88006, #27609, #58072 ) ;
#21820 = ORIENTED_EDGE ( 'NONE', *, *, #62068, .T. ) ;
#21821 = CARTESIAN_POINT ( 'NONE',  ( -108.6278307361934594, -24.15620529776629155, 10.23563542870659404 ) ) ;
#21822 = CARTESIAN_POINT ( 'NONE',  ( -77.58471930946036821, -24.51419770103158768, 9.386484678747166299 ) ) ;
#21823 = ADVANCED_FACE ( 'NONE', ( #39696 ), #93474, .T. ) ;
#21824 = CARTESIAN_POINT ( 'NONE',  ( -51.59326263455098172, -24.15620529776628089, 10.23563542870660470 ) ) ;
#21826 = ORIENTED_EDGE ( 'NONE', *, *, #7135, .T. ) ;
#21825 = CARTESIAN_POINT ( 'NONE',  ( -3.310264809446246570, -21.00426241492911927, 11.49999999999999645 ) ) ;
#21827 = ORIENTED_EDGE ( 'NONE', *, *, #59642, .T. ) ;
#21828 = CARTESIAN_POINT ( 'NONE',  ( 20.56832688555235222, -8.368550285707721414, 11.49999999999998934 ) ) ;
#21829 = CARTESIAN_POINT ( 'NONE',  ( -18.09956831669839872, 9.893135806712603397, -1.500000000000002220 ) ) ;
#21830 = EDGE_CURVE ( 'NONE', #17220, #26478, #69149, .T. ) ;
#21831 = VERTEX_POINT ( 'NONE', #70656 ) ;
#21832 = ORIENTED_EDGE ( 'NONE', *, *, #19324, .T. ) ;
#21833 = CARTESIAN_POINT ( 'NONE',  ( 6.697025426467099862, -6.376774720514424288, 21.43052570396496037 ) ) ;
#21834 = CARTESIAN_POINT ( 'NONE',  ( 2.787364042957740651, -5.876774720514424288, 21.14548745790758488 ) ) ;
#21835 = VERTEX_POINT ( 'NONE', #76739 ) ;
#21836 = ORIENTED_EDGE ( 'NONE', *, *, #52356, .T. ) ;
#21837 = DIRECTION ( 'NONE',  ( 0.000000000000000000, 0.000000000000000000, 1.000000000000000000 ) ) ;
#21839 = CARTESIAN_POINT ( 'NONE',  ( -41.53954185366745122, -24.35071581493542681, 9.817618358456032368 ) ) ;
#21838 = B_SPLINE_CURVE_WITH_KNOTS ( 'NONE', 3,
 ( #7008, #30339, #37955, #15117 ),
 .UNSPECIFIED., .F., .F.,
 ( 4, 4 ),
 ( 0.8003574401347743894, 0.8093638714068899231 ),
 .UNSPECIFIED. ) ;
#21840 = CARTESIAN_POINT ( 'NONE',  ( -85.52287095715006160, -23.47596703998600631, 11.44779298504228393 ) ) ;
#21841 = CARTESIAN_POINT ( 'NONE',  ( -8.262104503270727207, -19.10415460921518971, -1.500000000000002220 ) ) ;
#21842 = CARTESIAN_POINT ( 'NONE',  ( -12.31242093702619123, -17.95196869449987531, 11.49999999999999645 ) ) ;
#21843 = CARTESIAN_POINT ( 'NONE',  ( -40.52227049441191298, -25.27806139208687597, 5.079412585072950570 ) ) ;
#21844 = CARTESIAN_POINT ( 'NONE',  ( -52.52287095715006160, -23.72747288104470087, -1.053458166803227680 ) ) ;
#21845 = CARTESIAN_POINT ( 'NONE',  ( 21.16529133594374557, -7.503415950508986576, 11.49999999999998934 ) ) ;
#21846 = EDGE_CURVE ( 'NONE', #53793, #31312, #90253, .T. ) ;
#21847 = CARTESIAN_POINT ( 'NONE',  ( -50.80769758106637823, -25.26334732355762824, 4.647238457533181766 ) ) ;
#21848 = ORIENTED_EDGE ( 'NONE', *, *, #48200, .T. ) ;
#21849 = LINE ( 'NONE', #51328, #50146 ) ;
#21850 = DIRECTION ( 'NONE',  ( -0.000000000000000000, -0.000000000000000000, -1.000000000000000000 ) ) ;
#21851 = AXIS2_PLACEMENT_3D ( 'NONE', #39895, #93675, #93170 ) ;
#21852 = ORIENTED_EDGE ( 'NONE', *, *, #96206, .F. ) ;
#21853 = EDGE_LOOP ( 'NONE', ( #58125, #71237, #88153, #56619, #65626, #96766, #64869, #7000, #19436 ) ) ;
#21854 = EDGE_CURVE ( 'NONE', #29476, #93240, #45017, .T. ) ;
#21855 = CARTESIAN_POINT ( 'NONE',  ( -46.60716005348672297, -23.73791477778911840, 11.05961554403171299 ) ) ;
#21856 = EDGE_LOOP ( 'NONE', ( #70778, #74853 ) ) ;
#21857 = CARTESIAN_POINT ( 'NONE',  ( -9.236746577462426444, 19.23066362772381055, -1.500000000000002220 ) ) ;
#21858 = VERTEX_POINT ( 'NONE', #54434 ) ;
#21859 = CARTESIAN_POINT ( 'NONE',  ( -6.181720432442950219, -5.876774720514410966, 19.67464842890028720 ) ) ;
#21860 = CARTESIAN_POINT ( 'NONE',  ( -2.129267666952235682, 20.92775224702969439, -1.500000000000002220 ) ) ;
#21861 = DIRECTION ( 'NONE',  ( -0.000000000000000000, 2.173523156925979552E-06, -0.9999999999976378895 ) ) ;
#21862 = CARTESIAN_POINT ( 'NONE',  ( -111.2450078774014344, -25.25753193669086016, 3.808477968289406768 ) ) ;
#21863 = DIRECTION ( 'NONE',  ( 3.773278334444166432E-23, -1.000000000000000000, 0.000000000000000000 ) ) ;
#21864 = CARTESIAN_POINT ( 'NONE',  ( 20.57945552106664877, -7.502658216658728563, -1.500000000000002220 ) ) ;
#21865 = LINE ( 'NONE', #6156, #52833 ) ;
#21866 = ORIENTED_EDGE ( 'NONE', *, *, #54772, .T. ) ;
#21867 = CARTESIAN_POINT ( 'NONE',  ( -40.01839366089613748, -25.29500187561385260, 5.509688069775453556 ) ) ;
#21868 = CARTESIAN_POINT ( 'NONE',  ( -50.62287095715005592, -29.50249982740957577, 7.747779886224967605 ) ) ;
#21869 = B_SPLINE_CURVE_WITH_KNOTS ( 'NONE', 3,
 ( #5554, #98895, #43628, #89301, #50743, #74566, #27896, #81689, #36500, #96909 ),
 .UNSPECIFIED., .F., .F.,
 ( 4, 2, 2, 2, 4 ),
 ( 0.000000000000000000, 0.0004035656830125077606, 0.0008071313660250155212, 0.001210697049037523336, 0.001614262732050031042 ),
 .UNSPECIFIED. ) ;
#21870 = CARTESIAN_POINT ( 'NONE',  ( -130.5728709571500588, -23.47596703998600631, 11.44779298504227860 ) ) ;
#21871 = CARTESIAN_POINT ( 'NONE',  ( -10.23453989644235484, -23.17878777331894469, 8.640809912072077381 ) ) ;
#21872 = CARTESIAN_POINT ( 'NONE',  ( 14.64190796094839264, -15.47823801613018269, -1.500000000000002220 ) ) ;
#21873 = CARTESIAN_POINT ( 'NONE',  ( -98.51141593473609248, -24.35071581493543391, 9.817618358456027039 ) ) ;
#21874 = CARTESIAN_POINT ( 'NONE',  ( -107.5144641672072794, -24.35071581493543746, 9.817618358456021710 ) ) ;
#21875 = AXIS2_PLACEMENT_3D ( 'NONE', #8980, #39932, #33821 ) ;
#21876 = PLANE ( 'NONE',  #24350 ) ;
#21877 = CARTESIAN_POINT ( 'NONE',  ( -33.48326937963503269, -24.51314013834315375, 0.6176544820404119562 ) ) ;
#21878 = CARTESIAN_POINT ( 'NONE',  ( 21.67916507323446496, -5.852930566066080864, -1.500000000000002220 ) ) ;
#21879 = LINE ( 'NONE', #6173, #36105 ) ;
#21880 = ORIENTED_EDGE ( 'NONE', *, *, #14760, .T. ) ;
#21881 = CARTESIAN_POINT ( 'NONE',  ( -81.52287095715004739, -23.96177878511308634, 10.65340807706330395 ) ) ;
#21882 = CARTESIAN_POINT ( 'NONE',  ( -19.07250549579359244, -4.594354733287289605, 11.49999999999999645 ) ) ;
#21883 = CARTESIAN_POINT ( 'NONE',  ( -96.62287095715005592, -29.50248528299804818, 1.056150453629042030 ) ) ;
#21884 = PLANE ( 'NONE',  #59364 ) ;
#21885 = ORIENTED_EDGE ( 'NONE', *, *, #11340, .F. ) ;
#21886 = VECTOR ( 'NONE', #100214, 1000.000000000000000 ) ;
#21887 = PLANE ( 'NONE',  #60423 ) ;
#21888 = LINE ( 'NONE', #52868, #88546 ) ;
#21889 = FACE_OUTER_BOUND ( 'NONE', #94599, .T. ) ;
#21890 = AXIS2_PLACEMENT_3D ( 'NONE', #73890, #66296, #27718 ) ;
#21891 = CARTESIAN_POINT ( 'NONE',  ( -26.02232103978952438, -24.75203499431761500, 7.265335466635947093 ) ) ;
#21892 = CARTESIAN_POINT ( 'NONE',  ( -16.88869819569221065, 10.18974688345344148, 11.49999999999998934 ) ) ;
#21893 = ORIENTED_EDGE ( 'NONE', *, *, #13804, .F. ) ;
#21894 = DIRECTION ( 'NONE',  ( 0.000000000000000000, -2.173523156925980399E-06, 0.9999999999976378895 ) ) ;
#21895 = CARTESIAN_POINT ( 'NONE',  ( -116.6228709571500701, -23.48783264082478794, -1.443836473390058606 ) ) ;
#21896 = CALENDAR_DATE ( 2026, 9, 10 ) ;
#21897 = EDGE_CURVE ( 'NONE', #64237, #60171, #72613, .T. ) ;
#21898 = ORIENTED_EDGE ( 'NONE', *, *, #63293, .T. ) ;
#21899 = LINE ( 'NONE', #6195, #92137 ) ;
#21900 = CARTESIAN_POINT ( 'NONE',  ( -103.6228709571500559, -24.66019654487199375, 8.947790411086124607 ) ) ;
#21901 = DIRECTION ( 'NONE',  ( 0.000000000000000000, 0.000000000000000000, -1.000000000000000000 ) ) ;
#21902 = DIRECTION ( 'NONE',  ( -1.000000000000000000, -0.000000000000000000, 0.000000000000000000 ) ) ;
#21903 = DIRECTION ( 'NONE',  ( 0.000000000000000000, -2.173523156925979552E-06, 0.9999999999976378895 ) ) ;
#21904 = EDGE_CURVE ( 'NONE', #38251, #20637, #63673, .T. ) ;
#21905 = CARTESIAN_POINT ( 'NONE',  ( -69.71577706848860601, -25.24515085459215769, 5.512506713422812510 ) ) ;
#21906 = EDGE_CURVE ( 'NONE', #1896, #45069, #91997, .T. ) ;
#21907 = CARTESIAN_POINT ( 'NONE',  ( -107.5552281182121845, -23.96119346886881729, -0.6495511937831858207 ) ) ;
#21908 = CARTESIAN_POINT ( 'NONE',  ( 19.63333621495807435, 3.783328549194958867, 11.49999999999998934 ) ) ;
#21909 = B_SPLINE_CURVE_WITH_KNOTS ( 'NONE', 3,
 ( #19649, #81566, #59733, #69708 ),
 .UNSPECIFIED., .F., .F.,
 ( 4, 4 ),
 ( 1.387778780781445676E-17, 0.0001000000000000028508 ),
 .UNSPECIFIED. ) ;
#21910 = EDGE_CURVE ( 'NONE', #82077, #48068, #91494, .T. ) ;
#21911 = FACE_OUTER_BOUND ( 'NONE', #81536, .T. ) ;
#21912 = LINE ( 'NONE', #39152, #100231 ) ;
#21913 = VERTEX_POINT ( 'NONE', #62051 ) ;
#21914 = B_SPLINE_CURVE_WITH_KNOTS ( 'NONE', 3,
 ( #73373, #50045, #79477, #3378, #3871, #11466, #34310, #10462, #26193, #9465, #41422, #2874, #65288, #34809 ),
 .UNSPECIFIED., .F., .F.,
 ( 4, 2, 2, 2, 2, 2, 4 ),
 ( 0.000000000000000000, 0.0001605340506961548935, 0.0003210681013923097869, 0.0006421362027846000582, 0.0009632043041768902211, 0.001123738354873028960, 0.001284272405569167590 ),
 .UNSPECIFIED. ) ;
#21915 = CARTESIAN_POINT ( 'NONE',  ( -3.108974358974355923, -6.376774720514427841, 21.75000000000001066 ) ) ;
#21916 = ADVANCED_FACE ( 'NONE', ( #39194 ), #70152, .T. ) ;
#21917 = CARTESIAN_POINT ( 'NONE',  ( -109.5228709571500616, -23.47593901973090524, -1.443836447538996426 ) ) ;
#21918 = VECTOR ( 'NONE', #100158, 1000.000000000000000 ) ;
#21919 = CARTESIAN_POINT ( 'NONE',  ( -80.62881840819318313, -24.73531770709095312, 8.716586749053508498 ) ) ;
#21920 = DIRECTION ( 'NONE',  ( 1.000000000000000000, 0.000000000000000000, -5.238131417152343399E-15 ) ) ;
#21921 = CARTESIAN_POINT ( 'NONE',  ( -39.53341462708579712, -24.51314013834315730, 0.6176544820404118452 ) ) ;
#21922 = LINE ( 'NONE', #21423, #41618 ) ;
#21923 = CARTESIAN_POINT ( 'NONE',  ( -2.188401442307694289, -6.376774720514411854, 19.46153846153846700 ) ) ;
#21924 = CARTESIAN_POINT ( 'NONE',  ( -34.62287095715004881, -23.96127896941631619, -0.6493128931037907003 ) ) ;
#21925 = CARTESIAN_POINT ( 'NONE',  ( -70.52287095715007581, -29.50248528299804818, 1.056150453629036701 ) ) ;
#21926 = ORIENTED_EDGE ( 'NONE', *, *, #70427, .F. ) ;
#21927 = CARTESIAN_POINT ( 'NONE',  ( 0.8729654516333695824, -20.24016528753796962, -1.500000000000002220 ) ) ;
#21928 = CARTESIAN_POINT ( 'NONE',  ( -119.5228709571500758, -29.50250243563736774, 8.947779886222134493 ) ) ;
#21929 = CARTESIAN_POINT ( 'NONE',  ( -80.48900664166535535, -25.12298712672050982, 7.101635559041870494 ) ) ;
#21930 = LINE ( 'NONE', #52913, #46045 ) ;
#21931 = ORIENTED_EDGE ( 'NONE', *, *, #92161, .T. ) ;
#21932 = DIRECTION ( 'NONE',  ( -3.773278334453079030E-23, 0.9999999999976377785, 2.173523156925979128E-06 ) ) ;
#21933 = FACE_OUTER_BOUND ( 'NONE', #35361, .T. ) ;
#21934 = CARTESIAN_POINT ( 'NONE',  ( 18.99975792849237877, 6.539580213093530325, -1.500000000000002220 ) ) ;
#21935 = CARTESIAN_POINT ( 'NONE',  ( -11.11193726737652199, 17.91617163517716804, 11.49999999999999645 ) ) ;
#21936 = CARTESIAN_POINT ( 'NONE',  ( -101.5228709571500758, -24.64898659630368627, 1.056161002820829697 ) ) ;
#21937 = CARTESIAN_POINT ( 'NONE',  ( -22.05048665130746954, -1.834114841651104832, 11.49999999999998934 ) ) ;
#21938 = CARTESIAN_POINT ( 'NONE',  ( 12.93548710985481698, 15.95582723538240266, 11.49999999999998934 ) ) ;
#21939 = DIRECTION ( 'NONE',  ( -0.09824042138329623641, -2.980407940728110405E-17, 0.9951627101165078093 ) ) ;
#21940 = VECTOR ( 'NONE', #89609, 1000.000000000000000 ) ;
#21941 = CARTESIAN_POINT ( 'NONE',  ( 15.63775912259811918, 4.567193422985928564, -28.22903731538494299 ) ) ;
#21942 = VERTEX_POINT ( 'NONE', #34104 ) ;
#21943 = CARTESIAN_POINT ( 'NONE',  ( -15.87499999999997868, 0.000000000000000000, 1.249999999999997113 ) ) ;
#21944 = ORIENTED_EDGE ( 'NONE', *, *, #85445, .F. ) ;
#21945 = CARTESIAN_POINT ( 'NONE',  ( 30.93860345374796239, 5.965225279485572685, 26.43402280011862615 ) ) ;
#21946 = CARTESIAN_POINT ( 'NONE',  ( -67.62287095715004170, -24.50321055353805377, 9.387540953477529371 ) ) ;
#21947 = ORIENTED_EDGE ( 'NONE', *, *, #27772, .T. ) ;
#21948 = AXIS2_PLACEMENT_3D ( 'NONE', #68443, #29874, #91763 ) ;
#21949 = ORIENTED_EDGE ( 'NONE', *, *, #50224, .T. ) ;
#21950 = DIRECTION ( 'NONE',  ( -3.773278334444167608E-23, 1.000000000000000000, 0.000000000000000000 ) ) ;
#21951 = CARTESIAN_POINT ( 'NONE',  ( -49.36949249605027745, -25.10037777829114702, 7.227091855933934994 ) ) ;
#21952 = CARTESIAN_POINT ( 'NONE',  ( -89.62287095714999907, -24.51283580621364777, 0.6167428607019738163 ) ) ;
#21953 = CARTESIAN_POINT ( 'NONE',  ( -19.87711886888390822, 5.503898473480427711, -1.500000000000002220 ) ) ;
#21954 = B_SPLINE_CURVE_WITH_KNOTS ( 'NONE', 3,
 ( #87203, #41041, #71997, #18683 ),
 .UNSPECIFIED., .F., .F.,
 ( 4, 4 ),
 ( 0.1888945234595363343, 0.1898952705003016106 ),
 .UNSPECIFIED. ) ;
#21955 = AXIS2_PLACEMENT_3D ( 'NONE', #68386, #52657, #67393 ) ;
#21956 = CARTESIAN_POINT ( 'NONE',  ( -11.65619939812097527, 18.16556634249905855, 11.49999999999999645 ) ) ;
#21957 = ORIENTED_EDGE ( 'NONE', *, *, #97587, .F. ) ;
#21958 = CARTESIAN_POINT ( 'NONE',  ( -8.063330319165405768, -10.15233964170348457, 1.310587897985993733 ) ) ;
#21959 = EDGE_CURVE ( 'NONE', #12627, #33110, #17647, .T. ) ;
#21960 = DIRECTION ( 'NONE',  ( 0.000000000000000000, -1.000000000000000000, 0.000000000000000000 ) ) ;
#21961 = CARTESIAN_POINT ( 'NONE',  ( 16.41691039316204481, 15.16158741987741365, -1.500000000000002220 ) ) ;
#21962 = AXIS2_PLACEMENT_3D ( 'NONE', #23810, #47167, #83713 ) ;
#21963 = CARTESIAN_POINT ( 'NONE',  ( -79.95270946814521551, -25.12205784548233822, 6.976216635617262796 ) ) ;
#21964 = LINE ( 'NONE', #68165, #18927 ) ;
#21965 = ORIENTED_EDGE ( 'NONE', *, *, #86675, .T. ) ;
#21966 = CARTESIAN_POINT ( 'NONE',  ( -50.58953762381672448, -25.00182538069145011, 7.747789668545099317 ) ) ;
#21967 = CARTESIAN_POINT ( 'NONE',  ( -49.49482000239348878, -24.35071581493542325, 9.817618358456035921 ) ) ;
#21968 = CARTESIAN_POINT ( 'NONE',  ( -18.00717387566553995, 10.56535500573724740, -1.500000000000002220 ) ) ;
#21969 = ORIENTED_EDGE ( 'NONE', *, *, #57672, .T. ) ;
#21970 = EDGE_CURVE ( 'NONE', #1888, #2927, #64949, .T. ) ;
#21972 = ORIENTED_EDGE ( 'NONE', *, *, #77043, .F. ) ;
#21971 = CARTESIAN_POINT ( 'NONE',  ( -86.51786579561228052, -23.73766607897671221, -1.055555164236433141 ) ) ;
#21973 = ORIENTED_EDGE ( 'NONE', *, *, #27446, .T. ) ;
#21974 = CARTESIAN_POINT ( 'NONE',  ( -109.5183300406462479, -23.96169478059713498, 10.65365249895717703 ) ) ;
#21975 = CARTESIAN_POINT ( 'NONE',  ( 0.3207198112191017025, -21.10926996749724083, -1.500000000000002220 ) ) ;
#21976 = EDGE_CURVE ( 'NONE', #31671, #56351, #99928, .T. ) ;
#21977 = EDGE_LOOP ( 'NONE', ( #39301, #28529, #88524, #78616 ) ) ;
#21978 = FACE_OUTER_BOUND ( 'NONE', #56166, .T. ) ;
#21979 = CARTESIAN_POINT ( 'NONE',  ( -99.97649549088345111, -25.26221303177835154, 7.032284653420170173 ) ) ;
#21980 = CARTESIAN_POINT ( 'NONE',  ( -16.40380107638378604, 14.33077157581830008, -1.500000000000002220 ) ) ;
#21981 = CARTESIAN_POINT ( 'NONE',  ( 15.97264540888996365, -5.965225279485572685, -27.93485543958161443 ) ) ;
#21982 = CARTESIAN_POINT ( 'NONE',  ( 5.399550031316281640, -0.3587747205144061202, -28.54570968857217395 ) ) ;
#21983 = CARTESIAN_POINT ( 'NONE',  ( -79.48403147916279465, -25.21891630973060572, 6.539601158515170987 ) ) ;
#21984 = CARTESIAN_POINT ( 'NONE',  ( -12.31242093702619123, -17.95196869449987531, -1.500000000000002220 ) ) ;
#21985 = CARTESIAN_POINT ( 'NONE',  ( -71.70689869863497279, -25.31639743646335816, 6.146638256948438794 ) ) ;
#21987 = ORIENTED_EDGE ( 'NONE', *, *, #58412, .T. ) ;
#21986 = CARTESIAN_POINT ( 'NONE',  ( 6.212073114426278408, 21.40951068830820958, 11.49999999999999645 ) ) ;
#21988 = CARTESIAN_POINT ( 'NONE',  ( -124.4728709571500360, -29.48149383318413896, 5.000941583504025623 ) ) ;
#21989 = CARTESIAN_POINT ( 'NONE',  ( -85.53826411963355270, -25.00182538069147142, 7.747789668545045139 ) ) ;
#21990 = CARTESIAN_POINT ( 'NONE',  ( -43.62287095715007013, -23.94994826722515668, -0.6494450866351720864 ) ) ;
#21991 = ORIENTED_EDGE ( 'NONE', *, *, #6161, .T. ) ;
#21992 = VERTEX_POINT ( 'NONE', #56451 ) ;
#21993 = B_SPLINE_CURVE_WITH_KNOTS ( 'NONE', 3,
 ( #2575, #72589, #80688, #43133 ),
 .UNSPECIFIED., .F., .F.,
 ( 4, 4 ),
 ( 0.000000000000000000, 9.999999999998897304E-05 ),
 .UNSPECIFIED. ) ;
#21994 = ORIENTED_EDGE ( 'NONE', *, *, #11170, .F. ) ;
#21995 = CARTESIAN_POINT ( 'NONE',  ( -85.52287095715006160, -23.48786465467241058, 11.44779295918254292 ) ) ;
#21996 = CARTESIAN_POINT ( 'NONE',  ( 13.39648796734645231, 16.42122281929413319, 11.49999999999998934 ) ) ;
#21997 = PLANE ( 'NONE',  #4465 ) ;
#21998 = CARTESIAN_POINT ( 'NONE',  ( -130.5728709571500019, -23.86952536761623733, -1.017619990082604398 ) ) ;
#21999 = CARTESIAN_POINT ( 'NONE',  ( 20.59900142331985151, -4.215361659006737760, -17.99865718129769832 ) ) ;
#22000 = CARTESIAN_POINT ( 'NONE',  ( 6.371704462700114924, -5.876774720514427841, 21.83798798526824214 ) ) ;
#22001 = CARTESIAN_POINT ( 'NONE',  ( -19.00951991574052968, 3.723548053296564575, -1.500000000000002220 ) ) ;
#22002 = CARTESIAN_POINT ( 'NONE',  ( -40.93435094691191267, -25.25978494880519776, 3.590542803917028181 ) ) ;
#22003 = VERTEX_POINT ( 'NONE', #94988 ) ;
#22004 = CARTESIAN_POINT ( 'NONE',  ( 17.17441491540288823, 9.109037055621362455, 11.49999999999999645 ) ) ;
#22005 = DIRECTION ( 'NONE',  ( -0.000000000000000000, 1.000000000000000000, -0.000000000000000000 ) ) ;
#22006 = EDGE_LOOP ( 'NONE', ( #12026, #39312, #67665, #3154 ) ) ;
#22007 = CARTESIAN_POINT ( 'NONE',  ( -41.52287095715006870, -23.48786465467240347, 11.44779295918255180 ) ) ;
#22008 = CARTESIAN_POINT ( 'NONE',  ( 2.884397429187188333, -6.376774720514406525, 18.67943752795919110 ) ) ;
#22009 = DIRECTION ( 'NONE',  ( -1.000000000000000000, -3.773278334444167608E-23, -8.201307833595939069E-29 ) ) ;
#22010 = CARTESIAN_POINT ( 'NONE',  ( -97.25938181864586340, -23.78087380709146359, 10.97511746239721653 ) ) ;
#22011 = EDGE_CURVE ( 'NONE', #97904, #18367, #64073, .T. ) ;
#22012 = B_SPLINE_CURVE_WITH_KNOTS ( 'NONE', 3,
 ( #2087, #24895, #24399, #41646 ),
 .UNSPECIFIED., .F., .F.,
 ( 4, 4 ),
 ( 5.551115123125782086E-17, 9.999999999998900014E-05 ),
 .UNSPECIFIED. ) ;
#22013 = CARTESIAN_POINT ( 'NONE',  ( 14.10018531369908423, 13.67006465538575277, -1.500000000000002220 ) ) ;
#22014 = FACE_OUTER_BOUND ( 'NONE', #49250, .T. ) ;
#22015 = VERTEX_POINT ( 'NONE', #41725 ) ;
#22016 = CARTESIAN_POINT ( 'NONE',  ( 10.28227983848843152, -18.94921665015282031, 11.49999999999998934 ) ) ;
#22017 = CARTESIAN_POINT ( 'NONE',  ( -80.51244414166535535, -25.04307398257883577, 7.563174194274490780 ) ) ;
#22018 = LINE ( 'NONE', #59122, #80479 ) ;
#22019 = CARTESIAN_POINT ( 'NONE',  ( -57.62287095715003460, -24.65952944569304606, 1.056160979905696573 ) ) ;
#22020 = CARTESIAN_POINT ( 'NONE',  ( -100.0747864355570158, -25.27473232648502233, 3.344773415373787806 ) ) ;
#22021 = CARTESIAN_POINT ( 'NONE',  ( 5.395019145045520048, -22.42585393411717121, -1.500000000000002220 ) ) ;
#22022 = AXIS2_PLACEMENT_3D ( 'NONE', #99923, #30434, #71514 ) ;
#22023 = CALENDAR_DATE ( 2026, 9, 10 ) ;
#22024 = CARTESIAN_POINT ( 'NONE',  ( -93.54916376374448816, -24.34968618360934656, 0.1864209137778838343 ) ) ;
#22025 = CARTESIAN_POINT ( 'NONE',  ( -83.52287095715006160, -29.50250243563736774, 8.947779886222141599 ) ) ;
#22026 = CARTESIAN_POINT ( 'NONE',  ( 13.10547390533899836, 15.29217475743441312, 11.49999999999999645 ) ) ;
#22027 = CARTESIAN_POINT ( 'NONE',  ( -109.1652331756773862, -25.28814200412482549, 3.437502494680751752 ) ) ;
#22028 = CARTESIAN_POINT ( 'NONE',  ( -32.50391374051680060, -23.96169478059712787, 10.65365249895719124 ) ) ;
#22029 = AXIS2_PLACEMENT_3D ( 'NONE', #58817, #36469, #91255 ) ;
#22030 = EDGE_CURVE ( 'NONE', #79100, #97847, #50370, .T. ) ;
#22032 = DIRECTION ( 'NONE',  ( -0.000000000000000000, -1.000000000000000000, 0.000000000000000000 ) ) ;
#22031 = VECTOR ( 'NONE', #44894, 1000.000000000000000 ) ;
#22033 = CARTESIAN_POINT ( 'NONE',  ( -40.62287095715005592, -23.47593901973091235, -1.443836447539011525 ) ) ;
#22034 = LINE ( 'NONE', #68235, #75316 ) ;
#22035 = CARTESIAN_POINT ( 'NONE',  ( 19.12242951303546334, 5.485007674754557527, 11.49999999999998934 ) ) ;
#22036 = CIRCLE ( 'NONE', #69060, 1.325999999999990298 ) ;
#22037 = EDGE_CURVE ( 'NONE', #47882, #43726, #41931, .T. ) ;
#22038 = CARTESIAN_POINT ( 'NONE',  ( -97.62287095715005592, -23.48786465467241058, 11.44779295918254114 ) ) ;
#22039 = CARTESIAN_POINT ( 'NONE',  ( -16.86558833231006460, 10.32443627698238409, -1.500000000000002220 ) ) ;
#22040 = AXIS2_PLACEMENT_3D ( 'NONE', #50048, #74364, #73378 ) ;
#22041 = CARTESIAN_POINT ( 'NONE',  ( -126.5218657896009233, -23.73791477778912551, 11.05961554403169878 ) ) ;
#22042 = EDGE_CURVE ( 'NONE', #90366, #50837, #26491, .T. ) ;
#22043 = EDGE_CURVE ( 'NONE', #87115, #33316, #26981, .T. ) ;
#22044 = CARTESIAN_POINT ( 'NONE',  ( -1.030996059302438761, -6.376774720514415407, 20.06599527532949878 ) ) ;
#22045 = PLANE ( 'NONE',  #92892 ) ;
#22046 = CARTESIAN_POINT ( 'NONE',  ( -18.79711486612840332, 8.613068827758688428, 11.49999999999999645 ) ) ;
#22047 = CARTESIAN_POINT ( 'NONE',  ( -111.5895376238167245, -24.64965694238407679, 8.947790433994649462 ) ) ;
#22048 = ADVANCED_FACE ( 'NONE', ( #24971 ), #49337, .T. ) ;
#22049 = CARTESIAN_POINT ( 'NONE',  ( -24.90875734969025501, -6.376774720514426953, 27.45402280011862572 ) ) ;
#22050 = CARTESIAN_POINT ( 'NONE',  ( 0.000000000000000000, -5.876774720514426953, 15.00000000000000178 ) ) ;
#22051 = CARTESIAN_POINT ( 'NONE',  ( -20.26579564662877075, -10.28286414166031726, 11.49999999999999645 ) ) ;
#22052 = EDGE_LOOP ( 'NONE', ( #44367, #74722, #64350, #51326 ) ) ;
#22053 = DIRECTION ( 'NONE',  ( 1.000000000000000000, 0.000000000000000000, 0.000000000000000000 ) ) ;
#22054 = CARTESIAN_POINT ( 'NONE',  ( 27.53860345374808105, -1.477225279485574028, -1.352392034746782823 ) ) ;
#22055 = CARTESIAN_POINT ( 'NONE',  ( 15.40757771627215256, 13.04930689719894765, -1.500000000000002220 ) ) ;
#22056 = ADVANCED_FACE ( 'NONE', ( #87884, #9753 ), #81265, .F. ) ;
#22057 = CARTESIAN_POINT ( 'NONE',  ( -60.62287095715004881, -23.47593901973091235, -1.443836447539007972 ) ) ;
#22058 = LINE ( 'NONE', #69751, #15606 ) ;
#22059 = VECTOR ( 'NONE', #49277, 1000.000000000000000 ) ;
#22060 = ORIENTED_EDGE ( 'NONE', *, *, #75096, .T. ) ;
#22061 = ORIENTED_EDGE ( 'NONE', *, *, #27228, .T. ) ;
#22062 = CARTESIAN_POINT ( 'NONE',  ( -10.54059822343757880, -5.876774720514426953, 22.82308057603841078 ) ) ;
#22063 = CARTESIAN_POINT ( 'NONE',  ( 12.66508800429495629, 19.07499079241581086, 11.49999999999998934 ) ) ;
#22064 = DIRECTION ( 'NONE',  ( 0.9951627101165076983, 0.000000000000000000, 0.09824042138329622254 ) ) ;
#22065 = CARTESIAN_POINT ( 'NONE',  ( 8.597998336517790108, -19.88058937513707392, -1.500000000000002220 ) ) ;
#22066 = PLANE ( 'NONE',  #86851 ) ;
#22067 = CARTESIAN_POINT ( 'NONE',  ( -114.6228709571500701, -24.50216790748204687, 0.6166512839542572788 ) ) ;
#22068 = CARTESIAN_POINT ( 'NONE',  ( -13.90609606471210391, -15.62508359690603221, 11.49999999999999645 ) ) ;
#22069 = ORIENTED_EDGE ( 'NONE', *, *, #290, .F. ) ;
#22070 = CARTESIAN_POINT ( 'NONE',  ( -74.52287095715007581, -24.64965694238408034, 8.947790433994200043 ) ) ;
#22071 = CARTESIAN_POINT ( 'NONE',  ( 17.71009474140864981, 13.04663522181963309, 11.49999999999998934 ) ) ;
#22072 = CARTESIAN_POINT ( 'NONE',  ( 0.000000000000000000, -4.056774720514426669, 0.000000000000000000 ) ) ;
#22073 = CARTESIAN_POINT ( 'NONE',  ( -41.86334916006617135, -25.10926027280345707, 4.024173299727788589 ) ) ;
#22074 = ORIENTED_EDGE ( 'NONE', *, *, #91799, .T. ) ;
#22075 = CARTESIAN_POINT ( 'NONE',  ( -94.62287095715005592, -23.47596703998600631, 11.44779298504227860 ) ) ;
#22076 = CARTESIAN_POINT ( 'NONE',  ( -90.62361247365680583, -25.00182538069147142, 7.747789668545044250 ) ) ;
#22077 = ORIENTED_EDGE ( 'NONE', *, *, #84471, .F. ) ;
#22078 = DIRECTION ( 'NONE',  ( 0.000000000000000000, 0.000000000000000000, 1.000000000000000000 ) ) ;
#22079 = ORIENTED_EDGE ( 'NONE', *, *, #62272, .F. ) ;
#22080 = ORIENTED_EDGE ( 'NONE', *, *, #23941, .F. ) ;
#22081 = FACE_OUTER_BOUND ( 'NONE', #23189, .T. ) ;
#22082 = CARTESIAN_POINT ( 'NONE',  ( -95.62287095715004170, -24.52323809116984776, 9.355190652339416602 ) ) ;
#22083 = CARTESIAN_POINT ( 'NONE',  ( -36.57019023030961336, -23.48783264082477018, -1.443836473390095909 ) ) ;
#22084 = CARTESIAN_POINT ( 'NONE',  ( 19.91419669613914678, 4.404666692190684962, -1.500000000000002220 ) ) ;
#22085 = EDGE_CURVE ( 'NONE', #39655, #36906, #80774, .T. ) ;
#22086 = ORIENTED_EDGE ( 'NONE', *, *, #2198, .F. ) ;
#22087 = CARTESIAN_POINT ( 'NONE',  ( -93.62287095715005592, -24.64965695001468404, 8.947790433994180503 ) ) ;
#22088 = CARTESIAN_POINT ( 'NONE',  ( 23.60872659128563456, -0.9000000000000000222, -2.097483029078133665 ) ) ;
#22089 = AXIS2_PLACEMENT_3D ( 'NONE', #73360, #9950, #3855 ) ;
#22090 = EDGE_CURVE ( 'NONE', #31760, #78378, #51530, .T. ) ;
#22091 = CARTESIAN_POINT ( 'NONE',  ( -98.55620429048337883, -24.65952944569304606, 1.056160979905700792 ) ) ;
#22092 = CARTESIAN_POINT ( 'NONE',  ( 10.34999999999998010, 22.00000000000000000, 0.000000000000000000 ) ) ;
#22093 = ORIENTED_EDGE ( 'NONE', *, *, #28603, .F. ) ;
#22094 = CARTESIAN_POINT ( 'NONE',  ( -49.92287095715005307, -23.47596703998600631, 11.44779298504227683 ) ) ;
#22095 = CARTESIAN_POINT ( 'NONE',  ( -29.81175120719462157, -25.26247357602138166, 4.942810953739434687 ) ) ;
#22096 = CARTESIAN_POINT ( 'NONE',  ( -8.262104503270727207, -19.10415460921518971, -1.500000000000002220 ) ) ;
#22098 = EDGE_CURVE ( 'NONE', #44804, #8909, #40708, .T. ) ;
#22097 = ORIENTED_EDGE ( 'NONE', *, *, #88021, .T. ) ;
#22100 = ORIENTED_EDGE ( 'NONE', *, *, #62191, .F. ) ;
#22099 = CARTESIAN_POINT ( 'NONE',  ( -98.62287095715005592, -24.64965695001469115, 8.947790433994178727 ) ) ;
#22101 = VECTOR ( 'NONE', #66037, 1000.000000000000000 ) ;
#22102 = DIRECTION ( 'NONE',  ( 0.000000000000000000, 1.478457507934778393E-16, -1.000000000000000000 ) ) ;
#22104 = ORIENTED_EDGE ( 'NONE', *, *, #59460, .F. ) ;
#22103 = EDGE_CURVE ( 'NONE', #77156, #96725, #62402, .T. ) ;
#22105 = ORIENTED_EDGE ( 'NONE', *, *, #807, .T. ) ;
#22106 = VECTOR ( 'NONE', #65554, 1000.000000000000114 ) ;
#22107 = DIRECTION ( 'NONE',  ( 0.000000000000000000, -0.9999999999976377785, -2.173523156925979128E-06 ) ) ;
#22108 = CARTESIAN_POINT ( 'NONE',  ( -92.62287095715001328, -23.96177878511308634, 10.65340807706329862 ) ) ;
#22109 = CARTESIAN_POINT ( 'NONE',  ( -76.52287095715010423, -23.72773821059537269, 11.05748984161097503 ) ) ;
#22110 = AXIS2_PLACEMENT_3D ( 'NONE', #13358, #75263, #68162 ) ;
#22111 = CARTESIAN_POINT ( 'NONE',  ( -40.62287095715006302, -23.85229601348996553, 10.88205029486208808 ) ) ;
#22112 = CARTESIAN_POINT ( 'NONE',  ( -109.1226296748707654, -25.22180349218709949, 3.485716899910509259 ) ) ;
#22113 = CARTESIAN_POINT ( 'NONE',  ( -73.55620429048342146, -24.66019654487199020, 8.947790411086131712 ) ) ;
#22115 = ORIENTED_EDGE ( 'NONE', *, *, #93302, .F. ) ;
#22114 = CARTESIAN_POINT ( 'NONE',  ( -2.366842300981895519, -21.98859952056468714, 11.49999999999999645 ) ) ;
#22116 = DIRECTION ( 'NONE',  ( -1.000000000000000000, 0.000000000000000000, 0.000000000000000000 ) ) ;
#22117 = CARTESIAN_POINT ( 'NONE',  ( 21.95517018727266390, 5.574673621280945568, 11.49999999999998934 ) ) ;
#22119 = ORIENTED_EDGE ( 'NONE', *, *, #2958, .T. ) ;
#22118 = CARTESIAN_POINT ( 'NONE',  ( -111.5228709571500758, -24.66019654487200441, 8.947790411086108620 ) ) ;
#22120 = ORIENTED_EDGE ( 'NONE', *, *, #36774, .T. ) ;
#22121 = B_SPLINE_CURVE_WITH_KNOTS ( 'NONE', 3,
 ( #559, #99005, #29500, #91399 ),
 .UNSPECIFIED., .F., .F.,
 ( 4, 4 ),
 ( 0.6909934214884121406, 0.6999998527605277854 ),
 .UNSPECIFIED. ) ;
#22122 = DIRECTION ( 'NONE',  ( -0.000000000000000000, 1.000000000000000000, -0.000000000000000000 ) ) ;
#22123 = CC_DESIGN_PERSON_AND_ORGANIZATION_ASSIGNMENT ( #15918, #6812, ( #21418 ) ) ;
#22124 = CARTESIAN_POINT ( 'NONE',  ( 4.949566031639514918, 19.51814346981619863, -1.500000000000002220 ) ) ;
#22125 = LINE ( 'NONE', #53108, #57058 ) ;
#22126 = EDGE_LOOP ( 'NONE', ( #3666, #82468, #52577, #17207 ) ) ;
#22127 = CARTESIAN_POINT ( 'NONE',  ( -89.52287095715010423, -23.73934037231756733, 11.05740245334328797 ) ) ;
#22128 = CARTESIAN_POINT ( 'NONE',  ( -7.907391756136429528, -20.87048397725295956, -1.500000000000002220 ) ) ;
#22129 = ORIENTED_EDGE ( 'NONE', *, *, #56277, .F. ) ;
#22130 = ORIENTED_EDGE ( 'NONE', *, *, #29838, .F. ) ;
#22131 = CARTESIAN_POINT ( 'NONE',  ( 10.34999999999998010, 22.00000000000000000, 0.000000000000000000 ) ) ;
#22132 = CARTESIAN_POINT ( 'NONE',  ( -81.81052289590537896, -25.19653879850945444, 6.629276519863234185 ) ) ;
#22133 = DIRECTION ( 'NONE',  ( -1.000000000000000000, 8.334928612639484546E-17, 0.000000000000000000 ) ) ;
#22134 = VECTOR ( 'NONE', #30334, 1000.000000000000114 ) ;
#22135 = FACE_OUTER_BOUND ( 'NONE', #71568, .T. ) ;
#22136 = CARTESIAN_POINT ( 'NONE',  ( 14.43441819135929727, -5.965225279485572685, -28.36222020317710246 ) ) ;
#22137 = CARTESIAN_POINT ( 'NONE',  ( -1.081029368968937421, 19.50181592447522050, 11.49999999999998934 ) ) ;
#22138 = CARTESIAN_POINT ( 'NONE',  ( -32.62287095715006302, -23.47596703998600276, 11.44779298504227505 ) ) ;
#22139 = CARTESIAN_POINT ( 'NONE',  ( 2.695732861974529104, -21.29187259674557708, 11.49999999999998934 ) ) ;
#22140 = AXIS2_PLACEMENT_3D ( 'NONE', #52352, #84282, #77163 ) ;
#22141 = CARTESIAN_POINT ( 'NONE',  ( -2.656471864501908975, -6.376774720514411854, 19.66116880005639800 ) ) ;
#22142 = DIRECTION ( 'NONE',  ( -3.773278334444166432E-23, 1.000000000000000000, 0.000000000000000000 ) ) ;
#22143 = CARTESIAN_POINT ( 'NONE',  ( -122.6228709571500559, -24.65952944569305316, 1.056160979905706343 ) ) ;
#22144 = CARTESIAN_POINT ( 'NONE',  ( -21.74799678179195794, 7.114197580472080951, -1.500000000000002220 ) ) ;
#22145 = CARTESIAN_POINT ( 'NONE',  ( -106.5177683666152717, -23.96169478059714564, 10.65365249895717170 ) ) ;
#22146 = CARTESIAN_POINT ( 'NONE',  ( -29.62287095715004881, -24.57333416927490433, 1.056161302446588124 ) ) ;
#22147 = CARTESIAN_POINT ( 'NONE',  ( 13.89251353435424363, -14.32104260081073832, 11.49999999999999645 ) ) ;
#22148 = CARTESIAN_POINT ( 'NONE',  ( -89.81226385320384509, -25.06732983082694943, 7.447789526168956620 ) ) ;
#22149 = CARTESIAN_POINT ( 'NONE',  ( -74.62679211367564847, -24.51419770103159124, 9.386484678747162747 ) ) ;
#22150 = DIRECTION ( 'NONE',  ( -1.000000000000000000, 0.000000000000000000, 0.000000000000000000 ) ) ;
#22151 = EDGE_CURVE ( 'NONE', #56978, #46703, #87158, .T. ) ;
#22152 = EDGE_LOOP ( 'NONE', ( #98797, #27094, #28196, #38787 ) ) ;
#22153 = CARTESIAN_POINT ( 'NONE',  ( -106.5228709571500758, -23.47596703998600631, 11.44779298504228038 ) ) ;
#22154 = CARTESIAN_POINT ( 'NONE',  ( -65.52287095715001897, -24.63345952396254290, 9.038047939301506517 ) ) ;
#22155 = B_SPLINE_CURVE_WITH_KNOTS ( 'NONE', 3,
 ( #31268, #321, #63753, #69333, #85552, #39884, #25152, #48514 ),
 .UNSPECIFIED., .F., .F.,
 ( 4, 2, 2, 4 ),
 ( 0.000000000000000000, 0.002001079623178219757, 0.003001619434767331153, 0.004002159246356442983 ),
 .UNSPECIFIED. ) ;
#22156 = CARTESIAN_POINT ( 'NONE',  ( -11.39883337241029793, 18.50525654427185884, 11.49999999999998934 ) ) ;
#22157 = CARTESIAN_POINT ( 'NONE',  ( 15.97264540888995299, 3.316774720514426456, -27.93485543958162154 ) ) ;
#22158 = CARTESIAN_POINT ( 'NONE',  ( -19.37596289572233488, 2.755671585415585767, -1.500000000000002220 ) ) ;
#22159 = AXIS2_PLACEMENT_3D ( 'NONE', #56393, #87314, #89322 ) ;
#22160 = DIRECTION ( 'NONE',  ( 0.000000000000000000, 0.9999999999976377785, 2.173523156925979975E-06 ) ) ;
#22161 = ORIENTED_EDGE ( 'NONE', *, *, #92479, .F. ) ;
#22162 = ITEM_DEFINED_TRANSFORMATION ( 'NONE', 'NONE', #9928,  #218 ) ;
#22163 = EDGE_CURVE ( 'NONE', #60537, #47938, #67759, .T. ) ;
#22164 = DIRECTION ( 'NONE',  ( 1.000000000000000000, 3.773278334444167608E-23, 8.201307833595939069E-29 ) ) ;
#22165 = CARTESIAN_POINT ( 'NONE',  ( -88.52287095715006160, -29.50248528299804818, 1.056150453629040253 ) ) ;
#22166 = CARTESIAN_POINT ( 'NONE',  ( -12.04554601739387998, 16.56303510970703385, 11.49999999999999645 ) ) ;
#22167 = CARTESIAN_POINT ( 'NONE',  ( -94.52287095715007581, -23.72747288104470087, -1.053458166803226126 ) ) ;
#22168 = EDGE_CURVE ( 'NONE', #87869, #18728, #96991, .T. ) ;
#22169 = AXIS2_PLACEMENT_3D ( 'NONE', #63290, #86602, #22684 ) ;
#22170 = CARTESIAN_POINT ( 'NONE',  ( 0.3000000000000007661, 2.265596578422603396E-15, -18.50000000000000000 ) ) ;
#22171 = VERTEX_POINT ( 'NONE', #28470 ) ;
#22172 = CARTESIAN_POINT ( 'NONE',  ( -29.49875734969026198, -5.965225279485572685, 10.11402280011862587 ) ) ;
#22173 = CARTESIAN_POINT ( 'NONE',  ( -39.61224275064198963, -25.28892508652457849, 3.692191117659460176 ) ) ;
#22174 = AXIS2_PLACEMENT_3D ( 'NONE', #50332, #88389, #42240 ) ;
#22175 = PLANE ( 'NONE',  #27401 ) ;
#22176 = VECTOR ( 'NONE', #16625, 1000.000000000000000 ) ;
#22177 = EDGE_CURVE ( 'NONE', #95349, #72422, #68050, .T. ) ;
#22178 = CARTESIAN_POINT ( 'NONE',  ( 14.76093561896379214, 5.965225279485572685, -27.88148769130088667 ) ) ;
#22179 = CARTESIAN_POINT ( 'NONE',  ( -42.62287095715006302, -24.50321055353803956, 9.387540953477536476 ) ) ;
#22180 = CARTESIAN_POINT ( 'NONE',  ( 11.60186680256600233, 19.91347440808847935, 11.49999999999999645 ) ) ;
#22181 = CARTESIAN_POINT ( 'NONE',  ( 20.42703387425654427, 10.12935691860780985, -1.500000000000002220 ) ) ;
#22182 = CARTESIAN_POINT ( 'NONE',  ( -10.34999999999999254, 1.000000000000000000, -2.500000000000001332 ) ) ;
#22183 = LINE ( 'NONE', #76970, #82026 ) ;
#22184 = CARTESIAN_POINT ( 'NONE',  ( -60.85008373276800597, -25.19805002435821706, 6.796443416052955655 ) ) ;
#22185 = DIRECTION ( 'NONE',  ( -3.773278334444166432E-23, 1.000000000000000000, 0.000000000000000000 ) ) ;
#22186 = CARTESIAN_POINT ( 'NONE',  ( -110.5481100400817098, -25.00158670708910336, 2.256160236439219258 ) ) ;
#22187 = CARTESIAN_POINT ( 'NONE',  ( 1.548332177993611225, -21.85883989728069565, 11.49999999999998934 ) ) ;
#22188 = CARTESIAN_POINT ( 'NONE',  ( -54.58953762381672448, -23.48783264082478084, -1.443836473390070596 ) ) ;
#22189 = CARTESIAN_POINT ( 'NONE',  ( -50.62287095715004881, -23.85196035786901092, -0.8779234886474973631 ) ) ;
#22190 = CARTESIAN_POINT ( 'NONE',  ( -40.54449484207607668, -25.31535585427448609, 5.077976992978702420 ) ) ;
#22191 = CARTESIAN_POINT ( 'NONE',  ( -48.87574965546946260, -25.24455176971168413, 6.222157127945766142 ) ) ;
#22192 = CARTESIAN_POINT ( 'NONE',  ( -103.6228709571500417, -24.65952944569304606, 1.056160979905701680 ) ) ;
#22193 = CARTESIAN_POINT ( 'NONE',  ( -122.6228709571500843, -23.96177878511309345, 10.65340807706328441 ) ) ;
#22194 = ORIENTED_EDGE ( 'NONE', *, *, #43528, .T. ) ;
#22195 = CARTESIAN_POINT ( 'NONE',  ( 7.241121213506172438, 19.11196469071355963, 11.49999999999998934 ) ) ;
#22196 = ORIENTED_EDGE ( 'NONE', *, *, #53688, .F. ) ;
#22197 = ORIENTED_EDGE ( 'NONE', *, *, #4149, .T. ) ;
#22198 = ORIENTED_EDGE ( 'NONE', *, *, #3715, .T. ) ;
#22199 = VERTEX_POINT ( 'NONE', #4650 ) ;
#22200 = EDGE_CURVE ( 'NONE', #70837, #14471, #67261, .T. ) ;
#22201 = CARTESIAN_POINT ( 'NONE',  ( -8.497478458550677516, -21.44862750780143656, -1.500000000000002220 ) ) ;
#22202 = CARTESIAN_POINT ( 'NONE',  ( -61.63716700260808068, -24.15543982623907127, -0.2315651400026656481 ) ) ;
#22203 = CARTESIAN_POINT ( 'NONE',  ( -20.14672940031187665, -1.731937678239350298, -1.500000000000002220 ) ) ;
#22204 = ORIENTED_EDGE ( 'NONE', *, *, #74187, .T. ) ;
#22205 = VECTOR ( 'NONE', #91011, 1000.000000000000000 ) ;
#22206 = CARTESIAN_POINT ( 'NONE',  ( -27.14027225143419741, -25.03511874060541587, 4.027978703335532096 ) ) ;
#22207 = CARTESIAN_POINT ( 'NONE',  ( -72.52287095715007581, -23.48786465467241058, 11.44779295918254647 ) ) ;
#22208 = EDGE_CURVE ( 'NONE', #82121, #65481, #81805, .T. ) ;
#22209 = DIRECTION ( 'NONE',  ( 0.000000000000000000, 0.000000000000000000, 1.000000000000000000 ) ) ;
#22210 = CARTESIAN_POINT ( 'NONE',  ( -99.51645779387621360, -23.96169478059713853, 10.65365249895717703 ) ) ;
#22212 = ORIENTED_EDGE ( 'NONE', *, *, #89532, .F. ) ;
#22211 = CARTESIAN_POINT ( 'NONE',  ( -18.57871158907727249, 10.67946855401146777, 11.49999999999999645 ) ) ;
#22213 = CARTESIAN_POINT ( 'NONE',  ( -128.6228709571500701, -24.33832256526968862, 0.1851278514119945040 ) ) ;
#22214 = DIRECTION ( 'NONE',  ( -3.773278334453080206E-23, 0.9999999999976377785, 2.173523156925979975E-06 ) ) ;
#22215 = ORIENTED_EDGE ( 'NONE', *, *, #55584, .T. ) ;
#22216 = VECTOR ( 'NONE', #70568, 1000.000000000000000 ) ;
#22217 = CARTESIAN_POINT ( 'NONE',  ( -20.61657899823519813, -2.091364977790679980, -1.500000000000002220 ) ) ;
#22218 = EDGE_CURVE ( 'NONE', #87928, #82473, #38553, .T. ) ;
#22220 = ORIENTED_EDGE ( 'NONE', *, *, #62098, .T. ) ;
#22219 = LINE ( 'NONE', #53202, #50733 ) ;
#22221 = EDGE_CURVE ( 'NONE', #89963, #8495, #62916, .T. ) ;
#22222 = B_SPLINE_SURFACE_WITH_KNOTS ( 'NONE', 3, 3, ( 
 ( #56723, #33866, #5905, #13010 ),
 ( #58215, #59713, #4425, #98246 ),
 ( #89156, #4920, #67827, #83522 ),
 ( #20627, #6413, #44983, #19630 ),
 ( #51594, #58703, #36863, #43976 ),
 ( #36365, #35864, #68312, #97757 ),
 ( #43486, #37369, #28248, #50592 ) ),
 .UNSPECIFIED., .F., .F., .F.,
 ( 4, 3, 4 ),
 ( 4, 4 ),
 ( 0.0004766839783844792713, 0.1029713700210910104, 0.2054660560637975308 ),
 ( 0.2195498469782498629, 0.2206638714302722182 ),
 .UNSPECIFIED. ) ;
#22223 = CARTESIAN_POINT ( 'NONE',  ( -29.55620429048338593, -24.57942546158513508, 8.947790451450490679 ) ) ;
#22224 = VERTEX_POINT ( 'NONE', #6134 ) ;
#22225 = CARTESIAN_POINT ( 'NONE',  ( 4.967948717948723392, -5.876774720514413630, 20.00140224358974095 ) ) ;
#22226 = CARTESIAN_POINT ( 'NONE',  ( 20.57779966680088890, -7.652443150423321683, 11.49999999999999645 ) ) ;
#22227 = CARTESIAN_POINT ( 'NONE',  ( -73.56460842735368999, -23.48786465467241058, 11.44779295918254824 ) ) ;
#22228 = CARTESIAN_POINT ( 'NONE',  ( 14.20245820080859289, -17.52920931871068433, -1.500000000000002220 ) ) ;
#22229 = CARTESIAN_POINT ( 'NONE',  ( 10.18035917307295435, 18.35650967997132099, 11.49999999999998934 ) ) ;
#22230 = LINE ( 'NONE', #7523, #83684 ) ;
#22231 = DIRECTION ( 'NONE',  ( -0.6755245625654127117, 0.4376337494475115442, -0.5934166046845339437 ) ) ;
#22232 = EDGE_LOOP ( 'NONE', ( #64561, #77272, #9991, #24575 ) ) ;
#22233 = ORIENTED_EDGE ( 'NONE', *, *, #89177, .T. ) ;
#22234 = VERTEX_POINT ( 'NONE', #20348 ) ;
#22235 = CARTESIAN_POINT ( 'NONE',  ( -66.49653113318395015, -24.51314013834316441, 0.6176544820404136216 ) ) ;
#22236 = AXIS2_PLACEMENT_3D ( 'NONE', #98338, #21215, #83114 ) ;
#22237 = EDGE_CURVE ( 'NONE', #56809, #15338, #35103, .T. ) ;
#22238 = CARTESIAN_POINT ( 'NONE',  ( 20.54099941694853726, 6.510794959084822864, -1.500000000000002220 ) ) ;
#22239 = DIRECTION ( 'NONE',  ( 2.216313064514630211E-15, -7.253388211138789781E-15, 1.000000000000000000 ) ) ;
#22240 = ORIENTED_EDGE ( 'NONE', *, *, #1924, .T. ) ;
#22241 = CARTESIAN_POINT ( 'NONE',  ( -7.596101150008887082, -19.70107428960382734, 11.49999999999998934 ) ) ;
#22242 = CARTESIAN_POINT ( 'NONE',  ( 12.66784028006542151, -2.682774720514427003, -27.12025593822526304 ) ) ;
#22243 = CARTESIAN_POINT ( 'NONE',  ( -56.62287095715005592, -29.50250786944525672, 11.44777988621623876 ) ) ;
#22244 = EDGE_CURVE ( 'NONE', #2429, #29553, #35802, .T. ) ;
#22245 = CARTESIAN_POINT ( 'NONE',  ( -83.62625791794420138, -24.51419770103157347, 9.386484678747182286 ) ) ;
#22246 = AXIS2_PLACEMENT_3D ( 'NONE', #57357, #3060, #34502 ) ;
#22247 = CARTESIAN_POINT ( 'NONE',  ( 13.80377080874918150, 3.316774720514426900, -27.21172484903264532 ) ) ;
#22248 = FACE_OUTER_BOUND ( 'NONE', #60598, .T. ) ;
#22249 = CARTESIAN_POINT ( 'NONE',  ( 2.574831182292884435, -22.01391258260016315, -1.500000000000002220 ) ) ;
#22250 = CARTESIAN_POINT ( 'NONE',  ( -71.51122638652783792, -23.96119346886880308, -0.6495511937832095795 ) ) ;
#22251 = ORIENTED_EDGE ( 'NONE', *, *, #72583, .T. ) ;
#22252 = CARTESIAN_POINT ( 'NONE',  ( -51.08169923747086472, -25.24859996806887708, 4.960538017754059226 ) ) ;
#22253 = CARTESIAN_POINT ( 'NONE',  ( -79.62287095715002749, -23.72747288104469376, -1.053458166803226348 ) ) ;
#22254 = CYLINDRICAL_SURFACE ( 'NONE', #69539, 28.96799999999999642 ) ;
#22255 = EDGE_CURVE ( 'NONE', #57335, #31312, #43219, .T. ) ;
#22256 = EDGE_CURVE ( 'NONE', #23337, #97853, #89380, .T. ) ;
#22257 = DIRECTION ( 'NONE',  ( -0.000000000000000000, 1.000000000000000000, -0.000000000000000000 ) ) ;
#22258 = CARTESIAN_POINT ( 'NONE',  ( -18.83898130102433299, -4.906684326670742280, -1.500000000000002220 ) ) ;
#22259 = CARTESIAN_POINT ( 'NONE',  ( 16.24497012180664868, 13.92215130028523973, -1.500000000000002220 ) ) ;
#22260 = CARTESIAN_POINT ( 'NONE',  ( -62.52208516091440060, -23.48783264082476308, -1.443836473390090580 ) ) ;
#22261 = LINE ( 'NONE', #69456, #88408 ) ;
#22262 = CARTESIAN_POINT ( 'NONE',  ( 11.62916340711181284, -0.3587747205144265483, 28.75961759920349792 ) ) ;
#22263 = DIRECTION ( 'NONE',  ( -1.000000000000000000, -0.000000000000000000, -0.000000000000000000 ) ) ;
#22264 = CARTESIAN_POINT ( 'NONE',  ( -15.33504971967173702, 16.71734053393862496, -1.500000000000002220 ) ) ;
#22265 = ORIENTED_EDGE ( 'NONE', *, *, #80751, .F. ) ;
#22266 = DIRECTION ( 'NONE',  ( 0.000000000000000000, 1.000000000000000000, -8.673617379884035472E-16 ) ) ;
#22267 = DIRECTION ( 'NONE',  ( -0.000000000000000000, -1.000000000000000000, -0.000000000000000000 ) ) ;
#22268 = CARTESIAN_POINT ( 'NONE',  ( -19.37706247964952411, -4.161318200553020041, 11.49999999999999645 ) ) ;
#22269 = LINE ( 'NONE', #68473, #72332 ) ;
#22270 = EDGE_CURVE ( 'NONE', #48580, #89004, #39387, .T. ) ;
#22271 = VERTEX_POINT ( 'NONE', #50827 ) ;
#22272 = CARTESIAN_POINT ( 'NONE',  ( -5.891837592278976743, -5.876774720514418071, 20.62654306927474934 ) ) ;
#22273 = CARTESIAN_POINT ( 'NONE',  ( -68.52287095715006160, -23.48783264082476308, -1.443836473390092356 ) ) ;
#22274 = CARTESIAN_POINT ( 'NONE',  ( 19.28387207504633949, -9.851753786812027514, -1.500000000000002220 ) ) ;
#22275 = CIRCLE ( 'NONE', #79002, 10.11363636363636331 ) ;
#22276 = CARTESIAN_POINT ( 'NONE',  ( -49.47157371846719087, -25.27517952430710579, 3.177618491393788602 ) ) ;
#22277 = CARTESIAN_POINT ( 'NONE',  ( -16.98888496755095545, 9.415225082695979353, -1.500000000000002220 ) ) ;
#22278 = CARTESIAN_POINT ( 'NONE',  ( -61.62287095715007013, -23.96127896941632685, -0.6493128931037863705 ) ) ;
#22279 = DIRECTION ( 'NONE',  ( 0.000000000000000000, 2.173523156925980399E-06, -0.9999999999976378895 ) ) ;
#22280 = CARTESIAN_POINT ( 'NONE',  ( 19.51516567812286596, -3.327523070855789911, -1.500000000000002220 ) ) ;
#22281 = ORIENTED_EDGE ( 'NONE', *, *, #68571, .T. ) ;
#22282 = AXIS2_PLACEMENT_3D ( 'NONE', #62999, #9692, #65011 ) ;
#22283 = CARTESIAN_POINT ( 'NONE',  ( -19.38859340154505873, -6.080128201517944753, 11.49999999999999645 ) ) ;
#22284 = CARTESIAN_POINT ( 'NONE',  ( -80.59164251549320568, -24.40034930558991277, 0.3402023900116063482 ) ) ;
#22285 = EDGE_CURVE ( 'NONE', #50179, #90405, #46764, .T. ) ;
#22286 = DIRECTION ( 'NONE',  ( 3.773278334444166432E-23, -1.000000000000000000, 0.000000000000000000 ) ) ;
#22287 = EDGE_CURVE ( 'NONE', #2927, #12184, #85380, .T. ) ;
#22288 = ORIENTED_EDGE ( 'NONE', *, *, #649, .F. ) ;
#22289 = CARTESIAN_POINT ( 'NONE',  ( -102.5529375350971719, -24.15620529776628800, 10.23563542870660292 ) ) ;
#22290 = CARTESIAN_POINT ( 'NONE',  ( -119.4728709571500502, -25.40675428744130215, 5.000950437788803882 ) ) ;
#22291 = CARTESIAN_POINT ( 'NONE',  ( -49.74369414166532977, -25.25214427568299413, 4.940878066772249610 ) ) ;
#22292 = CARTESIAN_POINT ( 'NONE',  ( -128.6228709571500417, -24.65952944569305316, 1.056160979905707897 ) ) ;
#22293 = CARTESIAN_POINT ( 'NONE',  ( -0.7067007548136460260, -5.876774720514410077, 19.51517878119693350 ) ) ;
#22294 = CARTESIAN_POINT ( 'NONE',  ( -16.07871291144651593, -12.00523380332558965, -1.500000000000002220 ) ) ;
#22295 = B_SPLINE_CURVE_WITH_KNOTS ( 'NONE', 3,
 ( #52930, #60052, #82368, #12352 ),
 .UNSPECIFIED., .F., .F.,
 ( 4, 4 ),
 ( 1.859750800284052969E-05, 0.003138001591829818297 ),
 .UNSPECIFIED. ) ;
#22296 = EDGE_CURVE ( 'NONE', #38301, #85731, #27, .T. ) ;
#22297 = CARTESIAN_POINT ( 'NONE',  ( -85.52287095715009002, -24.62226745350443480, 0.9660975649729474091 ) ) ;
#22298 = ORIENTED_EDGE ( 'NONE', *, *, #98209, .T. ) ;
#22299 = CARTESIAN_POINT ( 'NONE',  ( -72.62287095715005592, -24.64965695001468404, 8.947790433994184056 ) ) ;
#22300 = VECTOR ( 'NONE', #71833, 1000.000000000000000 ) ;
#22301 = EDGE_CURVE ( 'NONE', #91517, #56450, #1029, .T. ) ;
#22302 = B_SPLINE_CURVE_WITH_KNOTS ( 'NONE', 3,
 ( #91422, #90437, #6196, #67123 ),
 .UNSPECIFIED., .F., .F.,
 ( 4, 4 ),
 ( 0.000000000000000000, 0.0001000000000000167422 ),
 .UNSPECIFIED. ) ;
#22303 = CARTESIAN_POINT ( 'NONE',  ( -22.87863416751641310, 0.2071024363326711970, 11.49999999999999645 ) ) ;
#22304 = CARTESIAN_POINT ( 'NONE',  ( -22.17926634000774655, 4.976981427743210951, 11.49999999999998934 ) ) ;
#22305 = CARTESIAN_POINT ( 'NONE',  ( -30.47287095715005734, -24.75009217604366896, 1.389584765085777107 ) ) ;
#22306 = CARTESIAN_POINT ( 'NONE',  ( -51.22287095715006444, -23.47596703998600631, 11.44779298504227683 ) ) ;
#22307 = CARTESIAN_POINT ( 'NONE',  ( -40.33261254874832247, -25.19566596169548589, 3.298413478895628970 ) ) ;
#22308 = CARTESIAN_POINT ( 'NONE',  ( -89.52287095715006160, -23.47593901973090169, -1.443836447538996426 ) ) ;
#22309 = VECTOR ( 'NONE', #83872, 1000.000000000000114 ) ;
#22310 = CARTESIAN_POINT ( 'NONE',  ( 10.95759398273795249, 4.132774720514426292, -26.86884997114579932 ) ) ;
#22311 = CARTESIAN_POINT ( 'NONE',  ( 4.621320343559262689, 12.74999999999999645, 2.100000000000000089 ) ) ;
#22312 = ORIENTED_EDGE ( 'NONE', *, *, #94920, .T. ) ;
#22313 = VECTOR ( 'NONE', #71470, 999.9999999999998863 ) ;
#22314 = CARTESIAN_POINT ( 'NONE',  ( -20.10423522397153562, 3.301153050299447056, 11.49999999999998934 ) ) ;
#22315 = ORIENTED_EDGE ( 'NONE', *, *, #85406, .T. ) ;
#22316 = CARTESIAN_POINT ( 'NONE',  ( 17.43399715339889511, -14.94103553264482720, -1.500000000000002220 ) ) ;
#22317 = CARTESIAN_POINT ( 'NONE',  ( -115.5228709571500616, -23.48786465467241769, 11.44779295918253759 ) ) ;
#22318 = ORIENTED_EDGE ( 'NONE', *, *, #77692, .T. ) ;
#22319 = CARTESIAN_POINT ( 'NONE',  ( -108.5164728378366448, -24.15620529776629510, 10.23563542870659404 ) ) ;
#22320 = CYLINDRICAL_SURFACE ( 'NONE', #79304, 1.399999999999998579 ) ;
#22321 = ADVANCED_FACE ( 'NONE', ( #92867 ), #77635, .F. ) ;
#22322 = CYLINDRICAL_SURFACE ( 'NONE', #18853, 1.399999999999998579 ) ;
#22324 = VERTEX_POINT ( 'NONE', #39083 ) ;
#22323 = CARTESIAN_POINT ( 'NONE',  ( -20.90244970016518877, -3.954922567530639199, 11.49999999999999645 ) ) ;
#22325 = EDGE_LOOP ( 'NONE', ( #91599, #28955, #98330, #51461 ) ) ;
#22326 = CARTESIAN_POINT ( 'NONE',  ( 7.537409830304743430, 20.87355781386819942, 11.49999999999998934 ) ) ;
#22327 = CARTESIAN_POINT ( 'NONE',  ( -11.86786554430972096, -16.85652113839894639, -1.500000000000002220 ) ) ;
#22328 = ORIENTED_EDGE ( 'NONE', *, *, #28255, .T. ) ;
#22329 = EDGE_LOOP ( 'NONE', ( #2668, #59752, #85789, #74626 ) ) ;
#22330 = DIRECTION ( 'NONE',  ( 0.000000000000000000, -0.000000000000000000, -1.000000000000000000 ) ) ;
#22331 = CARTESIAN_POINT ( 'NONE',  ( -113.6228709571500417, -24.66019654487199730, 8.947790411086121054 ) ) ;
#22332 = ORIENTED_EDGE ( 'NONE', *, *, #7163, .T. ) ;
#22333 = CARTESIAN_POINT ( 'NONE',  ( -91.58605177063969904, -24.51314013834316086, 0.6176544820404156200 ) ) ;
#22334 = VERTEX_POINT ( 'NONE', #76631 ) ;
#22335 = CARTESIAN_POINT ( 'NONE',  ( -125.5801323110720347, -25.21753527833458719, 3.539999278834446539 ) ) ;
#22336 = CARTESIAN_POINT ( 'NONE',  ( -88.62287095715004170, -29.50250786944525672, 11.44777988621623344 ) ) ;
#22337 = CARTESIAN_POINT ( 'NONE',  ( 20.84756458399398937, 0.1950554047328266483, -1.500000000000002220 ) ) ;
#22338 = CARTESIAN_POINT ( 'NONE',  ( -16.08361747308824263, -14.67194924222005170, 11.49999999999999645 ) ) ;
#22339 = LINE ( 'NONE', #12737, #33167 ) ;
#22340 = CARTESIAN_POINT ( 'NONE',  ( -78.63772173417845579, -23.96169478059713498, 10.65365249895717881 ) ) ;
#22341 = CARTESIAN_POINT ( 'NONE',  ( 22.29217321540274099, 2.676729263222305644, -1.500000000000002220 ) ) ;
#22342 = PLANE ( 'NONE',  #59528 ) ;
#22343 = ORIENTED_EDGE ( 'NONE', *, *, #54568, .F. ) ;
#22344 = CARTESIAN_POINT ( 'NONE',  ( -58.52287095715006160, -24.65952944569304250, 1.056160979905695463 ) ) ;
#22345 = DIRECTION ( 'NONE',  ( -0.000000000000000000, 0.000000000000000000, 1.000000000000000000 ) ) ;
#22346 = B_SPLINE_SURFACE_WITH_KNOTS ( 'NONE', 3, 1, ( 
 ( #27286, #58729 ),
 ( #89679, #27777 ),
 ( #34898, #64880 ),
 ( #89184, #57747 ),
 ( #42023, #72968 ),
 ( #20650, #3460 ),
 ( #20154, #80069 ),
 ( #51119, #65871 ),
 ( #82063, #50619 ),
 ( #41512, #95790 ),
 ( #34396, #65374 ),
 ( #81571, #12547 ),
 ( #96790, #26782 ),
 ( #88687, #19157 ),
 ( #12045, #73958 ),
 ( #30767, #60241 ),
 ( #91168, #37885 ),
 ( #98771, #98268 ),
 ( #29271, #6933 ),
 ( #75933, #90671 ),
 ( #29772, #100250 ),
 ( #45013, #68838 ),
 ( #22635, #36386 ),
 ( #53627, #51622 ),
 ( #99274, #92160 ),
 ( #44505, #52612 ),
 ( #84054, #7425 ) ),
 .UNSPECIFIED., .F., .F., .F.,
 ( 4, 1, 1, 1, 1, 1, 1, 1, 1, 1, 1, 1, 1, 1, 1, 1, 1, 1, 1, 1, 1, 1, 1, 1, 4 ),
 ( 2, 2 ),
 ( 0.000000000000000000, 0.03378811616271054641, 0.06719393237387928652, 0.09986241085682445728, 0.1325666121262581154, 0.1651511732547866207, 0.1979131873557913035, 0.2313190035669617506, 0.2650832782673736010, 0.2992553087581147908, 0.3343985665049780120, 0.3699428235093075723, 0.4062835607000604976, 0.4440638196985086106, 0.4829977068727752676, 0.5233544466133043249, 0.5655365896041486540, 0.6096129240658192394, 0.6563908113764169716, 0.7058854949364569142, 0.7583245002617309272, 0.8138317829411497728, 0.8727945590393895170, 0.9347222295400736680, 1.000000000000000000 ),
 ( 0.000000000000000000, 1.000000000000000000 ),
 .UNSPECIFIED. ) ;
#22347 = VERTEX_POINT ( 'NONE', #22838 ) ;
#22348 = ORIENTED_EDGE ( 'NONE', *, *, #74378, .T. ) ;
#22349 = DIRECTION ( 'NONE',  ( -3.773278334444166432E-23, 1.000000000000000000, 0.000000000000000000 ) ) ;
#22350 = ORIENTED_EDGE ( 'NONE', *, *, #67688, .F. ) ;
#22351 = EDGE_CURVE ( 'NONE', #23980, #37481, #15747, .T. ) ;
#22352 = CARTESIAN_POINT ( 'NONE',  ( 21.01207135711032237, 3.775690236426352264, -1.500000000000002220 ) ) ;
#22353 = ORIENTED_EDGE ( 'NONE', *, *, #66242, .T. ) ;
#22354 = CARTESIAN_POINT ( 'NONE',  ( -17.93810645791062441, 10.97360191750010827, -1.500000000000002220 ) ) ;
#22355 = CARTESIAN_POINT ( 'NONE',  ( -30.53646390802392929, -24.83533449111644842, 1.633466014234818076 ) ) ;
#22356 = CARTESIAN_POINT ( 'NONE',  ( 15.29947330337541445, -3.316774720514426456, -27.16854002387010780 ) ) ;
#22357 = CARTESIAN_POINT ( 'NONE',  ( -65.52287095715004739, -24.82576562948885979, 8.398263436605498455 ) ) ;
#22358 = CARTESIAN_POINT ( 'NONE',  ( -21.51515180086577317, 4.489188270810763548, -1.500000000000002220 ) ) ;
#22359 = CARTESIAN_POINT ( 'NONE',  ( -87.60282549588966106, -23.48783264082478084, -1.443836473390063713 ) ) ;
#22360 = ORIENTED_EDGE ( 'NONE', *, *, #42902, .F. ) ;
#22361 = CARTESIAN_POINT ( 'NONE',  ( -74.62287095715005592, -24.64965695001467694, 8.947790433994184056 ) ) ;
#22362 = ADVANCED_FACE ( 'NONE', ( #91869 ), #12669, .T. ) ;
#22363 = EDGE_CURVE ( 'NONE', #78994, #25204, #36963, .T. ) ;
#22364 = AXIS2_PLACEMENT_3D ( 'NONE', #14422, #68726, #14918 ) ;
#22365 = EDGE_CURVE ( 'NONE', #37863, #82958, #33459, .T. ) ;
#22366 = CARTESIAN_POINT ( 'NONE',  ( -116.6228709571500133, -24.50216790748204332, 0.6166512839542576119 ) ) ;
#22367 = CARTESIAN_POINT ( 'NONE',  ( -39.55620429048340014, -23.48783264082477729, -1.443836473390071484 ) ) ;
#22368 = EDGE_CURVE ( 'NONE', #30073, #57610, #69766, .T. ) ;
#22369 = CARTESIAN_POINT ( 'NONE',  ( -20.44301536939603992, -23.48238912038987536, 9.960784317162937995 ) ) ;
#22370 = B_SPLINE_CURVE_WITH_KNOTS ( 'NONE', 3,
 ( #59035, #89973, #12834, #90964, #51918, #37675 ),
 .UNSPECIFIED., .F., .F.,
 ( 4, 2, 4 ),
 ( 0.000000000000000000, 0.001380901958385393966, 0.002761803916770787931 ),
 .UNSPECIFIED. ) ;
#22371 = CARTESIAN_POINT ( 'NONE',  ( 18.63368790978032763, -10.32677859091227113, -1.500000000000002220 ) ) ;
#22372 = CARTESIAN_POINT ( 'NONE',  ( -98.55492552392462358, -23.96169478059713498, 10.65365249895717881 ) ) ;
#22373 = CARTESIAN_POINT ( 'NONE',  ( -107.5862535881878870, -24.66019654487200441, 8.947790411086112172 ) ) ;
#22374 = LINE ( 'NONE', #83290, #98943 ) ;
#22375 = AXIS2_PLACEMENT_3D ( 'NONE', #48040, #75479, #61290 ) ;
#22376 = CARTESIAN_POINT ( 'NONE',  ( -33.58058290153915237, -24.51314013834315375, 0.6176544820404119562 ) ) ;
#22377 = CARTESIAN_POINT ( 'NONE',  ( -17.89120377161202313, 13.61666483413312712, -1.500000000000002220 ) ) ;
#22378 = CARTESIAN_POINT ( 'NONE',  ( -110.9402950654992708, -25.21970293610405633, 6.713732480141158199 ) ) ;
#22379 = ORIENTED_EDGE ( 'NONE', *, *, #37769, .T. ) ;
#22380 = B_SPLINE_CURVE_WITH_KNOTS ( 'NONE', 3,
 ( #42374, #20005, #74296, #66714 ),
 .UNSPECIFIED., .F., .F.,
 ( 4, 4 ),
 ( 0.000000000000000000, 0.0001000000000000028644 ),
 .UNSPECIFIED. ) ;
#22381 = LINE ( 'NONE', #58118, #6093 ) ;
#22382 = CARTESIAN_POINT ( 'NONE',  ( -5.058734511472819051, -18.94576116945722788, 11.49999999999999645 ) ) ;
#22383 = DIRECTION ( 'NONE',  ( -3.773278334453079618E-23, 0.9999999999976377785, 2.173523156925979975E-06 ) ) ;
#22384 = AXIS2_PLACEMENT_3D ( 'NONE', #37043, #45660, #29422 ) ;
#22385 = LINE ( 'NONE', #13283, #83616 ) ;
#22386 = ADVANCED_FACE ( 'NONE', ( #10644 ), #87771, .F. ) ;
#22387 = EDGE_LOOP ( 'NONE', ( #47995, #28737, #15115, #90187 ) ) ;
#22388 = CARTESIAN_POINT ( 'NONE',  ( -88.55141012998306849, -24.15620529776628800, 10.23563542870660115 ) ) ;
#22389 = CARTESIAN_POINT ( 'NONE',  ( -125.0509062400423659, -25.34771247321013732, 6.200312561216485108 ) ) ;
#22390 = CARTESIAN_POINT ( 'NONE',  ( -89.90249562519868221, -25.22174524493127734, 6.695141717414601068 ) ) ;
#22391 = PLANE ( 'NONE',  #5058 ) ;
#22393 = EDGE_CURVE ( 'NONE', #49971, #14697, #94372, .T. ) ;
#22392 = CARTESIAN_POINT ( 'NONE',  ( -19.50520112914412252, -2.896358124273927359, 11.49999999999998934 ) ) ;
#22394 = VECTOR ( 'NONE', #19310, 1000.000000000000114 ) ;
#22395 = ORIENTED_EDGE ( 'NONE', *, *, #92034, .F. ) ;
#22396 = CARTESIAN_POINT ( 'NONE',  ( -120.5228709571501042, -24.63345952396256777, 9.038047939301501188 ) ) ;
#22397 = CARTESIAN_POINT ( 'NONE',  ( -118.5228709571501611, -23.96127896941632685, -0.6493128931037936979 ) ) ;
#22398 = ADVANCED_FACE ( 'NONE', ( #71048 ), #33980, .F. ) ;
#22399 = PERSON_AND_ORGANIZATION_ROLE ( 'design_owner' ) ;
#22400 = ORIENTED_EDGE ( 'NONE', *, *, #6109, .T. ) ;
#22401 = CARTESIAN_POINT ( 'NONE',  ( -109.6228709571500559, -24.66019654487199730, 8.947790411086124607 ) ) ;
#22402 = LINE ( 'NONE', #53385, #6929 ) ;
#22403 = DIRECTION ( 'NONE',  ( 0.000000000000000000, 0.000000000000000000, 1.000000000000000000 ) ) ;
#22404 = CARTESIAN_POINT ( 'NONE',  ( 31.79364159983995464, -5.965225279485572685, -11.59305536555894278 ) ) ;
#22405 = CARTESIAN_POINT ( 'NONE',  ( 22.02124265030973760, 6.143225279485574397, 12.85402280011862430 ) ) ;
#22406 = PLANE ( 'NONE',  #74865 ) ;
#22407 = CARTESIAN_POINT ( 'NONE',  ( -91.52287095715007581, -23.72773821059536914, 11.05748984161097326 ) ) ;
#22408 = CARTESIAN_POINT ( 'NONE',  ( 12.72590371223024697, 15.41468647733915809, 11.49999999999998934 ) ) ;
#22409 = ADVANCED_FACE ( 'NONE', ( #18253 ), #94870, .F. ) ;
#22410 = CARTESIAN_POINT ( 'NONE',  ( 6.660000000000001030, 9.283009703645923594, -0.8121581124701985344 ) ) ;
#22411 = CARTESIAN_POINT ( 'NONE',  ( -45.66178293155309831, -23.85049219812685450, 10.88485053497527133 ) ) ;
#22412 = ORIENTED_EDGE ( 'NONE', *, *, #28014, .F. ) ;
#22413 = ADVANCED_FACE ( 'NONE', ( #87260 ), #32987, .T. ) ;
#22414 = LINE ( 'NONE', #92436, #84235 ) ;
#22415 = CARTESIAN_POINT ( 'NONE',  ( -80.65304639033715262, -23.48786465467241413, 11.44779295918254824 ) ) ;
#22416 = DIRECTION ( 'NONE',  ( -0.2164396139380966033, 0.9762960071199348056, -0.000000000000000000 ) ) ;
#22417 = CARTESIAN_POINT ( 'NONE',  ( -81.55436275622071207, -23.96119346886881019, -0.6495511937831893734 ) ) ;
#22418 = CARTESIAN_POINT ( 'NONE',  ( -13.89275734969026388, 5.965225279485572685, 31.02402280011862246 ) ) ;
#22419 = DIRECTION ( 'NONE',  ( 0.000000000000000000, -1.084202172485504557E-16, 1.000000000000000000 ) ) ;
#22420 = B_SPLINE_CURVE_WITH_KNOTS ( 'NONE', 3,
 ( #36088, #19359, #6129, #57947 ),
 .UNSPECIFIED., .F., .F.,
 ( 4, 4 ),
 ( 0.000000000000000000, 1.000000000000000000 ),
 .UNSPECIFIED. ) ;
#22421 = B_SPLINE_SURFACE_WITH_KNOTS ( 'NONE', 3, 3, ( 
 ( #4826, #66750, #97667, #98653 ),
 ( #29152, #59123, #90059, #82438 ),
 ( #12920, #46882, #16410, #1210 ),
 ( #62115, #85428, #62612, #76308 ),
 ( #23515, #93036, #54490, #70216 ),
 ( #38254, #7810, #15415, #37765 ),
 ( #69213, #38754, #47384, #31643 ),
 ( #92540, #14416, #15914, #24029 ),
 ( #697, #23014, #45393, #22517 ),
 ( #6809, #93533, #8312, #7303 ) ),
 .UNSPECIFIED., .F., .F., .F.,
 ( 4, 3, 3, 4 ),
 ( 4, 4 ),
 ( 0.0004766839783810765570, 0.1491231665100168358, 0.2234464077758347156, 0.2977696490416525954 ),
 ( 0.8996026503961034315, 0.9011514434348439906 ),
 .UNSPECIFIED. ) ;
#22422 = DIRECTION ( 'NONE',  ( -1.000000000000000000, -1.387778780781445429E-16, -0.000000000000000000 ) ) ;
#22423 = CARTESIAN_POINT ( 'NONE',  ( 30.09341516180546350, -1.477225279485574028, -11.39311774897855756 ) ) ;
#22424 = VERTEX_POINT ( 'NONE', #95874 ) ;
#22425 = CARTESIAN_POINT ( 'NONE',  ( 2.300710779914242110, 20.15441874099239783, -1.500000000000002220 ) ) ;
#22426 = CARTESIAN_POINT ( 'NONE',  ( -29.49875734969025842, 5.965225279485572685, 15.62202280011862321 ) ) ;
#22427 = DIRECTION ( 'NONE',  ( 0.000000000000000000, 0.000000000000000000, -1.000000000000000000 ) ) ;
#22428 = VECTOR ( 'NONE', #62767, 1000.000000000000114 ) ;
#22429 = CARTESIAN_POINT ( 'NONE',  ( -90.52287095715006160, -23.47593901973090524, -1.443836447538996426 ) ) ;
#22430 = SHAPE_REPRESENTATION ( 'Locking Button_Varsay\X2\0131\X0\lan', ( #37391 ), #48843 ) ;
#22431 = ORIENTED_EDGE ( 'NONE', *, *, #94557, .T. ) ;
#22432 = CARTESIAN_POINT ( 'NONE',  ( 17.47419131657910185, -0.3587747205144265483, 28.31804950686278843 ) ) ;
#22433 = CARTESIAN_POINT ( 'NONE',  ( 7.160000000000000142, -7.572993419422048511, 8.500388862211309515 ) ) ;
#22434 = CARTESIAN_POINT ( 'NONE',  ( -4.233023369943174075, 19.68221892606961987, -1.500000000000002220 ) ) ;
#22435 = CARTESIAN_POINT ( 'NONE',  ( 17.50165659415881336, 11.77592616506222711, 11.49999999999999645 ) ) ;
#22436 = DIRECTION ( 'NONE',  ( -3.773278334453079030E-23, 0.9999999999976377785, 2.173523156925979128E-06 ) ) ;
#22437 = CARTESIAN_POINT ( 'NONE',  ( 21.00647827173414939, 6.864759178008983831, 11.49999999999998934 ) ) ;
#22438 = CARTESIAN_POINT ( 'NONE',  ( 2.947869850540926429, 20.32360706268488215, 11.49999999999998934 ) ) ;
#22439 = CARTESIAN_POINT ( 'NONE',  ( -96.52287095715006160, -24.50216790748204332, 0.6166512839542606095 ) ) ;
#22440 = CARTESIAN_POINT ( 'NONE',  ( -60.64671536082958880, -24.15503026093916006, -0.2815557561904390993 ) ) ;
#22441 = ORIENTED_EDGE ( 'NONE', *, *, #47666, .T. ) ;
#22442 = LINE ( 'NONE', #21943, #46051 ) ;
#22443 = ORIENTED_EDGE ( 'NONE', *, *, #98334, .T. ) ;
#22444 = DIRECTION ( 'NONE',  ( -3.773278334453079030E-23, 0.9999999999976377785, 2.173523156925979128E-06 ) ) ;
#22445 = CARTESIAN_POINT ( 'NONE',  ( -119.6228709571500559, -29.50250243563736774, 8.947779886222134493 ) ) ;
#22446 = ORIENTED_EDGE ( 'NONE', *, *, #84248, .F. ) ;
#22447 = ORIENTED_EDGE ( 'NONE', *, *, #80981, .T. ) ;
#22448 = AXIS2_PLACEMENT_3D ( 'NONE', #79599, #62387, #55788 ) ;
#22449 = VERTEX_POINT ( 'NONE', #86263 ) ;
#22450 = DIRECTION ( 'NONE',  ( 0.000000000000000000, 1.000000000000000000, -0.000000000000000000 ) ) ;
#22451 = CARTESIAN_POINT ( 'NONE',  ( -99.62287095715005592, -23.47596703998600631, 11.44779298504227860 ) ) ;
#22452 = CARTESIAN_POINT ( 'NONE',  ( 0.3906119451836247425, -6.376774720514418959, 20.56083401959467594 ) ) ;
#22453 = CARTESIAN_POINT ( 'NONE',  ( -19.88974639711211623, -5.441847772814488948, -1.500000000000002220 ) ) ;
#22454 = CARTESIAN_POINT ( 'NONE',  ( -3.891998276399621481, 21.28400606017829233, 11.49999999999999645 ) ) ;
#22455 = EDGE_LOOP ( 'NONE', ( #54896, #4708, #50803, #90998 ) ) ;
#22456 = CARTESIAN_POINT ( 'NONE',  ( 1.751198251822017937, 22.56127314141087581, 2.100000000000000089 ) ) ;
#22457 = CARTESIAN_POINT ( 'NONE',  ( -125.5228709571500616, -23.48786465467241769, 11.44779295918253581 ) ) ;
#22458 = CARTESIAN_POINT ( 'NONE',  ( -20.95026660567425481, -7.857139728745305973, -1.500000000000002220 ) ) ;
#22459 = CARTESIAN_POINT ( 'NONE',  ( -80.26303174456680267, -25.12205807651210066, 7.082509393110550278 ) ) ;
#22460 = CARTESIAN_POINT ( 'NONE',  ( -84.62912479653624587, -24.34968618360934300, 0.1864209137778835568 ) ) ;
#22461 = EDGE_LOOP ( 'NONE', ( #54865, #83569, #89895, #40944 ) ) ;
#22462 = CARTESIAN_POINT ( 'NONE',  ( 32.01683625711453374, -5.152774720514459617, -11.91548796314834036 ) ) ;
#22463 = CARTESIAN_POINT ( 'NONE',  ( -49.65272675066790242, -23.73791477778911840, 11.05961554403170943 ) ) ;
#22464 = CARTESIAN_POINT ( 'NONE',  ( -20.92377055399060737, -0.003182555231893603818, -1.500000000000002220 ) ) ;
#22465 = EDGE_LOOP ( 'NONE', ( #83910, #75154, #7603, #63955 ) ) ;
#22467 = ORIENTED_EDGE ( 'NONE', *, *, #72017, .T. ) ;
#22466 = CARTESIAN_POINT ( 'NONE',  ( -67.60280104496969500, -23.73791477778911840, 11.05961554403170766 ) ) ;
#22468 = ORIENTED_EDGE ( 'NONE', *, *, #48370, .T. ) ;
#22469 = CARTESIAN_POINT ( 'NONE',  ( -128.6228709571500417, -24.33927499327855415, 9.819080762295822495 ) ) ;
#22470 = CARTESIAN_POINT ( 'NONE',  ( 20.41123533131232648, 5.719371238976541427, -1.500000000000002220 ) ) ;
#22471 = ORIENTED_EDGE ( 'NONE', *, *, #69482, .F. ) ;
#22472 = DIRECTION ( 'NONE',  ( -1.000000000000000000, -0.000000000000000000, -0.000000000000000000 ) ) ;
#22474 = ADVANCED_FACE ( 'NONE', ( #63452 ), #48725, .T. ) ;
#22473 = CARTESIAN_POINT ( 'NONE',  ( -99.47310917600722746, -25.26221224442602420, 6.670037606239634265 ) ) ;
#22475 = CARTESIAN_POINT ( 'NONE',  ( 21.06710269851327766, -5.618397932909799941, 11.49999999999998934 ) ) ;
#22476 = CARTESIAN_POINT ( 'NONE',  ( -96.52287095715006160, -29.50247984919015209, -1.443849546365050029 ) ) ;
#22477 = EDGE_CURVE ( 'NONE', #20863, #71424, #34547, .T. ) ;
#22478 = CARTESIAN_POINT ( 'NONE',  ( 5.271800844963591359, -0.3587747205143965168, -28.56638892015329745 ) ) ;
#22479 = CARTESIAN_POINT ( 'NONE',  ( -79.37867731102689106, -25.25089957557972298, 6.257626200401206873 ) ) ;
#22480 = CARTESIAN_POINT ( 'NONE',  ( -16.08361747308824263, -14.67194924222005170, -1.500000000000002220 ) ) ;
#22481 = CARTESIAN_POINT ( 'NONE',  ( -71.68214140181162009, -25.31639691930716651, 5.908703739881754124 ) ) ;
#22483 = ORIENTED_EDGE ( 'NONE', *, *, #38947, .F. ) ;
#22482 = CARTESIAN_POINT ( 'NONE',  ( 2.183928509170398602, -22.20744181112294413, 11.49999999999999645 ) ) ;
#22484 = DIRECTION ( 'NONE',  ( 0.000000000000000000, 2.173523156925980399E-06, -0.9999999999976378895 ) ) ;
#22485 = DIRECTION ( 'NONE',  ( -3.773278334453079030E-23, 0.9999999999976377785, 2.173523156925979128E-06 ) ) ;
#22486 = CARTESIAN_POINT ( 'NONE',  ( -28.84663072490566194, -5.965225279485572685, 28.73989617533406715 ) ) ;
#22487 = ORIENTED_EDGE ( 'NONE', *, *, #16919, .T. ) ;
#22488 = EDGE_CURVE ( 'NONE', #50699, #60506, #41103, .T. ) ;
#22489 = EDGE_CURVE ( 'NONE', #81452, #85746, #33472, .T. ) ;
#22490 = ORIENTED_EDGE ( 'NONE', *, *, #83931, .T. ) ;
#22491 = EDGE_CURVE ( 'NONE', #83112, #18471, #66022, .T. ) ;
#22492 = ORIENTED_EDGE ( 'NONE', *, *, #51282, .T. ) ;
#22493 = DIRECTION ( 'NONE',  ( -0.5656310827093756766, 0.8246584009594636333, 1.161164194647626880E-16 ) ) ;
#22494 = CARTESIAN_POINT ( 'NONE',  ( -4.771770383141621608, -20.67029057396967318, 11.49999999999998934 ) ) ;
#22495 = PLANE ( 'NONE',  #17414 ) ;
#22496 = CARTESIAN_POINT ( 'NONE',  ( -80.51244414166535535, -25.03138299555828894, 7.563174219685121713 ) ) ;
#22497 = CARTESIAN_POINT ( 'NONE',  ( -59.58953762381671737, -24.66019654487199375, 8.947790411086138818 ) ) ;
#22498 = LINE ( 'NONE', #53491, #65385 ) ;
#22499 = PLANE ( 'NONE',  #51786 ) ;
#22500 = CARTESIAN_POINT ( 'NONE',  ( -45.56057666545407869, -23.85016227208580020, -0.8807180028928389692 ) ) ;
#22501 = ORIENTED_EDGE ( 'NONE', *, *, #90567, .F. ) ;
#22502 = CIRCLE ( 'NONE', #43612, 1.000000000000000000 ) ;
#22503 = CARTESIAN_POINT ( 'NONE',  ( 10.09180897563621926, 16.61094848277074476, 11.49999999999999645 ) ) ;
#22504 = CARTESIAN_POINT ( 'NONE',  ( -88.88918693012689687, -29.50249691823240994, 6.409318347766594037 ) ) ;
#22505 = VECTOR ( 'NONE', #49752, 1000.000000000000000 ) ;
#22506 = ORIENTED_EDGE ( 'NONE', *, *, #54041, .F. ) ;
#22507 = CARTESIAN_POINT ( 'NONE',  ( -41.52287095715006870, -24.65952944569304606, 1.056160979905691910 ) ) ;
#22508 = CARTESIAN_POINT ( 'NONE',  ( -44.58953762381671737, -23.47593901973091235, -1.443836447539011525 ) ) ;
#22509 = CIRCLE ( 'NONE', #30639, 252.4458649670781085 ) ;
#22510 = DIRECTION ( 'NONE',  ( -1.000000000000000000, -0.000000000000000000, -0.000000000000000000 ) ) ;
#22512 = ADVANCED_FACE ( 'NONE', ( #62268 ), #55161, .F. ) ;
#22511 = CARTESIAN_POINT ( 'NONE',  ( -19.07250549579359244, -4.594354733287289605, 11.49999999999998934 ) ) ;
#22513 = DIRECTION ( 'NONE',  ( 0.000000000000000000, -0.9999999999976377785, -2.173523156925979128E-06 ) ) ;
#22514 = EDGE_LOOP ( 'NONE', ( #28222, #72658, #61819, #67177 ) ) ;
#22515 = CARTESIAN_POINT ( 'NONE',  ( 19.30674495121141376, 9.566621930910674365, -1.500000000000002220 ) ) ;
#22516 = VECTOR ( 'NONE', #36672, 1000.000000000000114 ) ;
#22517 = CARTESIAN_POINT ( 'NONE',  ( -40.47158788874726554, -24.92564183028978775, 1.928384488918254203 ) ) ;
#22518 = CARTESIAN_POINT ( 'NONE',  ( -90.52287095715009002, -24.83620972994591725, 8.398175272781365663 ) ) ;
#22519 = CARTESIAN_POINT ( 'NONE',  ( -13.44081803467414638, 18.71018530922267686, -1.500000000000002220 ) ) ;
#22520 = APPROVAL_ROLE ( '' ) ;
#22521 = CARTESIAN_POINT ( 'NONE',  ( 8.599999999999999645, 24.84999999999999787, 2.100000000000000089 ) ) ;
#22522 = LINE ( 'NONE', #29656, #19886 ) ;
#22523 = CARTESIAN_POINT ( 'NONE',  ( -20.01257119864951051, 2.908879540851186274, 11.49999999999999645 ) ) ;
#22524 = FACE_OUTER_BOUND ( 'NONE', #18125, .T. ) ;
#22525 = CARTESIAN_POINT ( 'NONE',  ( -91.52287095715006160, -24.65952944569304606, 1.056160979905700570 ) ) ;
#22526 = VECTOR ( 'NONE', #81360, 1000.000000000000114 ) ;
#22527 = CARTESIAN_POINT ( 'NONE',  ( -110.8797149084312537, -25.10921396279124096, 2.935128329961295357 ) ) ;
#22528 = DIRECTION ( 'NONE',  ( 0.000000000000000000, 0.000000000000000000, -1.000000000000000000 ) ) ;
#22529 = CARTESIAN_POINT ( 'NONE',  ( -110.6372435692922664, -25.29779163436222333, 3.331084253915489235 ) ) ;
#22530 = CARTESIAN_POINT ( 'NONE',  ( 18.06118663784855372, 8.336529998961283994, -1.500000000000002220 ) ) ;
#22531 = CARTESIAN_POINT ( 'NONE',  ( -97.55620429048339304, -23.48786465467241769, 11.44779295918254114 ) ) ;
#22532 = CARTESIAN_POINT ( 'NONE',  ( -19.19514693104756375, 4.742496307885142315, -1.500000000000002220 ) ) ;
#22533 = CARTESIAN_POINT ( 'NONE',  ( -56.50282025588294488, -24.15543982623907127, -0.2315651400026670359 ) ) ;
#22534 = ADVANCED_FACE ( 'NONE', ( #46534, #37920 ), #94193, .T. ) ;
#22535 = CARTESIAN_POINT ( 'NONE',  ( -40.37522208020789805, -25.29116519044529099, 2.834757491049489264 ) ) ;
#22536 = DIRECTION ( 'NONE',  ( 0.000000000000000000, 0.9999999999976377785, 2.173523156925979128E-06 ) ) ;
#22537 = CARTESIAN_POINT ( 'NONE',  ( 7.614520588612671226, -19.20288753073135268, 11.49999999999999645 ) ) ;
#22538 = CARTESIAN_POINT ( 'NONE',  ( -98.58953762381672448, -24.64898659630529210, 1.056161002820829475 ) ) ;
#22539 = ADVANCED_FACE ( 'NONE', ( #86088 ), #62779, .T. ) ;
#22540 = FACE_OUTER_BOUND ( 'NONE', #99593, .T. ) ;
#22541 = VECTOR ( 'NONE', #76688, 1000.000000000000000 ) ;
#22542 = CARTESIAN_POINT ( 'NONE',  ( -21.73129956901698989, 6.668506094012985663, 11.49999999999999645 ) ) ;
#22543 = VERTEX_POINT ( 'NONE', #32303 ) ;
#22544 = CARTESIAN_POINT ( 'NONE',  ( -67.52287095715007581, -24.50216790748204687, 0.6166512839542540592 ) ) ;
#22545 = CARTESIAN_POINT ( 'NONE',  ( -3.826923076923074429, -6.376774720514427841, 21.75000000000000355 ) ) ;
#22546 = CARTESIAN_POINT ( 'NONE',  ( 17.97931717627152182, 9.192180251422895410, 11.49999999999998934 ) ) ;
#22547 = CARTESIAN_POINT ( 'NONE',  ( -108.6228709571500417, -23.47596703998600631, 11.44779298504227860 ) ) ;
#22548 = LINE ( 'NONE', #13952, #54510 ) ;
#22549 = ORIENTED_EDGE ( 'NONE', *, *, #2599, .T. ) ;
#22550 = ORIENTED_EDGE ( 'NONE', *, *, #71638, .F. ) ;
#22551 = CARTESIAN_POINT ( 'NONE',  ( -0.3225169060639742624, -5.876774720514411854, 19.46611907402017749 ) ) ;
#22552 = CARTESIAN_POINT ( 'NONE',  ( 21.75204538223844963, -7.182240389990739438, -1.500000000000002220 ) ) ;
#22553 = CARTESIAN_POINT ( 'NONE',  ( -51.19827071096799642, -25.18439730688664469, 3.666040128663992981 ) ) ;
#22554 = CARTESIAN_POINT ( 'NONE',  ( 2.186256072416925544, -21.55203199515037582, -1.500000000000002220 ) ) ;
#22555 = CARTESIAN_POINT ( 'NONE',  ( -13.89275734969026388, 0.3587747205144262708, 30.51402280011862089 ) ) ;
#22556 = DIRECTION ( 'NONE',  ( 0.000000000000000000, -0.000000000000000000, -1.000000000000000000 ) ) ;
#22557 = CARTESIAN_POINT ( 'NONE',  ( -12.67655569012464944, 16.65582705476778358, 11.49999999999999645 ) ) ;
#22558 = ORIENTED_EDGE ( 'NONE', *, *, #89628, .F. ) ;
#22559 = CARTESIAN_POINT ( 'NONE',  ( -69.23586867255411903, -25.24754350588972684, 5.333583042115673578 ) ) ;
#22560 = CARTESIAN_POINT ( 'NONE',  ( -0.4018715335629812202, -22.01094342083549193, -1.500000000000002220 ) ) ;
#22561 = CARTESIAN_POINT ( 'NONE',  ( 32.66876533700882845, -6.475225279485573360, -12.58926540598385557 ) ) ;
#22562 = CARTESIAN_POINT ( 'NONE',  ( -41.32330479122543210, -25.10925829605731607, 3.114706959938358111 ) ) ;
#22563 = ORIENTED_EDGE ( 'NONE', *, *, #58382, .F. ) ;
#22564 = CARTESIAN_POINT ( 'NONE',  ( -38.62287095715005592, -29.50248528299804818, 1.056150453629031594 ) ) ;
#22565 = CARTESIAN_POINT ( 'NONE',  ( -90.58310212721774235, -24.92592662359561473, 8.075495903018000021 ) ) ;
#22566 = EDGE_LOOP ( 'NONE', ( #18708, #80365, #36868, #73643 ) ) ;
#22567 = CARTESIAN_POINT ( 'NONE',  ( -117.6228709571500559, -29.50248528299804818, 1.056150453629045360 ) ) ;
#22568 = ORIENTED_EDGE ( 'NONE', *, *, #34194, .T. ) ;
#22569 = AXIS2_PLACEMENT_3D ( 'NONE', #5381, #65809, #96729 ) ;
#22570 = ORIENTED_EDGE ( 'NONE', *, *, #79308, .F. ) ;
#22571 = CARTESIAN_POINT ( 'NONE',  ( -41.58953762381673158, -24.64965694238406613, 8.947790433994661896 ) ) ;
#22572 = CARTESIAN_POINT ( 'NONE',  ( -101.7007079832508367, -25.10935996662800562, 3.725872784279629979 ) ) ;
#22573 = CARTESIAN_POINT ( 'NONE',  ( -100.5228709571500758, -24.14406661686760103, 10.28769366194082302 ) ) ;
#22574 = CARTESIAN_POINT ( 'NONE',  ( 20.14718400222343320, -3.498931157112906476, -1.500000000000002220 ) ) ;
#22575 = ORIENTED_EDGE ( 'NONE', *, *, #79700, .T. ) ;
#22576 = CARTESIAN_POINT ( 'NONE',  ( -0.4362980769230789257, -5.876774720514411854, 19.46153846153846345 ) ) ;
#22577 = CIRCLE ( 'NONE', #71212, 8.452410033082761842 ) ;
#22578 = CARTESIAN_POINT ( 'NONE',  ( -61.52287095715007581, -23.47593901973090169, -1.443836447538997092 ) ) ;
#22579 = CARTESIAN_POINT ( 'NONE',  ( -99.52287095715011844, -23.48783264083466449, -1.443836473374706442 ) ) ;
#22580 = CARTESIAN_POINT ( 'NONE',  ( -10.38793682863964563, 19.71736701935523683, 11.49999999999998934 ) ) ;
#22581 = B_SPLINE_CURVE_WITH_KNOTS ( 'NONE', 3,
 ( #9116, #32457, #24343, #33453, #2024, #10625, #63433, #3024, #94350, #95357, #25842, #8622, #56819, #86741, #17229, #48194, #41587, #9620 ),
 .UNSPECIFIED., .F., .F.,
 ( 4, 2, 2, 2, 2, 2, 2, 2, 4 ),
 ( 0.004711333090593654814, 0.005300261127349137000, 0.005889189164104619185, 0.006478117200860101371, 0.007067045237615584424, 0.007655973274371065743, 0.008244901311126548796, 0.008833829347882030114, 0.009422757384637513167 ),
 .UNSPECIFIED. ) ;
#22582 = FACE_OUTER_BOUND ( 'NONE', #28570, .T. ) ;
#22583 = CARTESIAN_POINT ( 'NONE',  ( -91.52287095715006160, -24.64898659630368272, 1.056161002820827921 ) ) ;
#22584 = ORIENTED_EDGE ( 'NONE', *, *, #37057, .T. ) ;
#22585 = LINE ( 'NONE', #32212, #16009 ) ;
#22586 = VECTOR ( 'NONE', #27720, 1000.000000000000000 ) ;
#22587 = CARTESIAN_POINT ( 'NONE',  ( -29.79716636085243664, -25.26247483479900424, 5.521952527462851812 ) ) ;
#22588 = VECTOR ( 'NONE', #61409, 1000.000000000000000 ) ;
#22589 = CARTESIAN_POINT ( 'NONE',  ( 19.72710162658169608, 6.580912942549038469, -1.500000000000002220 ) ) ;
#22590 = ORIENTED_EDGE ( 'NONE', *, *, #60458, .T. ) ;
#22592 = VERTEX_POINT ( 'NONE', #85086 ) ;
#22591 = CARTESIAN_POINT ( 'NONE',  ( 4.647383884978952828, -6.376774720514411854, 19.72975307774251164 ) ) ;
#22593 = VECTOR ( 'NONE', #49359, 1000.000000000000114 ) ;
#22594 = CARTESIAN_POINT ( 'NONE',  ( -51.31235188911633571, -25.12217787106197164, 6.754155556777655889 ) ) ;
#22595 = ORIENTED_EDGE ( 'NONE', *, *, #16689, .F. ) ;
#22596 = VERTEX_POINT ( 'NONE', #54653 ) ;
#22597 = DIRECTION ( 'NONE',  ( -1.000000000000000000, 0.000000000000000000, -0.000000000000000000 ) ) ;
#22599 = EDGE_CURVE ( 'NONE', #47563, #52812, #1837, .T. ) ;
#22598 = CARTESIAN_POINT ( 'NONE',  ( -50.72667573002448904, -25.27412235707870636, 2.869183044873688360 ) ) ;
#22600 = CARTESIAN_POINT ( 'NONE',  ( -10.34999999999999254, 0.9999999999999993339, 3.499999999999998668 ) ) ;
#22601 = DIRECTION ( 'NONE',  ( 0.000000000000000000, -1.408054769461694189E-16, 1.000000000000000000 ) ) ;
#22602 = FACE_OUTER_BOUND ( 'NONE', #63886, .T. ) ;
#22603 = CARTESIAN_POINT ( 'NONE',  ( 4.621320343559255583, 11.49999999999999467, 0.000000000000000000 ) ) ;
#22605 = EDGE_LOOP ( 'NONE', ( #85865, #45219, #65088, #66500 ) ) ;
#22604 = CARTESIAN_POINT ( 'NONE',  ( 19.81268554055766273, 9.900562300003143079, 11.49999999999999645 ) ) ;
#22606 = CARTESIAN_POINT ( 'NONE',  ( -105.6228709571500559, -23.47596703998600631, 11.44779298504227860 ) ) ;
#22607 = EDGE_CURVE ( 'NONE', #62448, #42265, #51427, .T. ) ;
#22608 = CARTESIAN_POINT ( 'NONE',  ( -18.78231125015805958, 12.62931641965373153, 11.49999999999998934 ) ) ;
#22609 = ADVANCED_FACE ( 'NONE', ( #8965 ), #16068, .T. ) ;
#22611 = VERTEX_POINT ( 'NONE', #16567 ) ;
#22610 = CARTESIAN_POINT ( 'NONE',  ( -29.24636659180999843, -25.20264517434234364, 4.940287045316306802 ) ) ;
#22612 = B_SPLINE_CURVE_WITH_KNOTS ( 'NONE', 3,
 ( #15840, #48317, #8245, #87364, #48824, #55429, #54924, #40698 ),
 .UNSPECIFIED., .F., .F.,
 ( 4, 2, 2, 4 ),
 ( -0.001240355328176769457, -0.0002398155169398802182, 0.0007607242942970090203, 0.002761803916770789232 ),
 .UNSPECIFIED. ) ;
#22613 = ADVANCED_FACE ( 'NONE', ( #76462 ), #99788, .F. ) ;
#22614 = VERTEX_POINT ( 'NONE', #38916 ) ;
#22615 = ADVANCED_FACE ( 'NONE', ( #30296 ), #22673, .T. ) ;
#22616 = PLANE ( 'NONE',  #45050 ) ;
#22617 = CARTESIAN_POINT ( 'NONE',  ( -19.68739882612603864, 4.164723872966736629, 11.49999999999998934 ) ) ;
#22618 = B_SPLINE_SURFACE_WITH_KNOTS ( 'NONE', 3, 3, ( 
 ( #56536, #33686, #64665, #95578 ),
 ( #87974, #90460, #97572, #12825 ),
 ( #28073, #89962, #20938, #51911 ),
 ( #88976, #13821, #82839, #50413 ),
 ( #81356, #43796, #13320, #75715 ),
 ( #11835, #42808, #59522, #52402 ),
 ( #21427, #44301, #58527, #73739 ) ),
 .UNSPECIFIED., .F., .F., .F.,
 ( 4, 3, 4 ),
 ( 4, 4 ),
 ( 0.0004766839783825378447, 0.1029713700210901917, 0.2054660560637978362 ),
 ( 0.02950150192610306865, 0.03052783842092137920 ),
 .UNSPECIFIED. ) ;
#22619 = CARTESIAN_POINT ( 'NONE',  ( -99.58953762381672448, -23.47596703998600631, 11.44779298504227683 ) ) ;
#22620 = ORIENTED_EDGE ( 'NONE', *, *, #39984, .T. ) ;
#22621 = CARTESIAN_POINT ( 'NONE',  ( 15.89146238746079831, -3.595713655330296188, -28.00617091144486182 ) ) ;
#22622 = CARTESIAN_POINT ( 'NONE',  ( 4.697571063781373013, 21.84268702631108994, -1.500000000000002220 ) ) ;
#22623 = B_SPLINE_CURVE_WITH_KNOTS ( 'NONE', 3,
 ( #60907, #52285, #91834, #13704 ),
 .UNSPECIFIED., .F., .F.,
 ( 4, 4 ),
 ( 0.009792917360197044008, 0.01879934863231252917 ),
 .UNSPECIFIED. ) ;
#22624 = EDGE_CURVE ( 'NONE', #37337, #30827, #31810, .T. ) ;
#22625 = ORIENTED_EDGE ( 'NONE', *, *, #78404, .F. ) ;
#22626 = EDGE_LOOP ( 'NONE', ( #38026, #22129, #29851, #95485 ) ) ;
#22627 = CARTESIAN_POINT ( 'NONE',  ( -24.90875734969025501, 6.376774720514426953, 27.45402280011862572 ) ) ;
#22628 = CARTESIAN_POINT ( 'NONE',  ( -80.51244414166535535, -25.03284467579916495, 7.563174216508125269 ) ) ;
#22629 = PLANE ( 'NONE',  #24684 ) ;
#22630 = DIRECTION ( 'NONE',  ( -1.000000000000000000, -3.773278334444168195E-23, -8.201307807930740669E-29 ) ) ;
#22631 = DIRECTION ( 'NONE',  ( 1.000000000000000000, 0.000000000000000000, 0.000000000000000000 ) ) ;
#22632 = CARTESIAN_POINT ( 'NONE',  ( 16.94836550497923966, -9.742303593519430649, -1.500000000000002220 ) ) ;
#22633 = LINE ( 'NONE', #55115, #5319 ) ;
#22634 = CARTESIAN_POINT ( 'NONE',  ( -20.40864349294084334, -6.676163967499375573, -1.500000000000002220 ) ) ;
#22635 = CARTESIAN_POINT ( 'NONE',  ( -25.56915516548917822, -24.92775208071710935, 4.121106392019679987 ) ) ;
#22636 = DIRECTION ( 'NONE',  ( -3.773278334453079030E-23, 0.9999999999976377785, 2.173523156925979128E-06 ) ) ;
#22637 = DIRECTION ( 'NONE',  ( -0.000000000000000000, 1.000000000000000000, -0.000000000000000000 ) ) ;
#22638 = VECTOR ( 'NONE', #50615, 1000.000000000000000 ) ;
#22639 = CARTESIAN_POINT ( 'NONE',  ( 18.61037501828884189, -13.27421459584354579, -1.500000000000002220 ) ) ;
#22640 = CALENDAR_DATE ( 2026, 9, 10 ) ;
#22641 = CARTESIAN_POINT ( 'NONE',  ( -94.62287095715005592, -29.50247984919015209, -1.443849546365051806 ) ) ;
#22642 = CARTESIAN_POINT ( 'NONE',  ( -60.62287095715004881, -29.50248789122583659, 2.256150453626215580 ) ) ;
#22643 = CARTESIAN_POINT ( 'NONE',  ( -19.61284664649099696, 3.773188449817356904, 11.49999999999999645 ) ) ;
#22644 = CARTESIAN_POINT ( 'NONE',  ( -60.62287095715004881, -29.50250243563736774, 8.947779886222145151 ) ) ;
#22645 = VECTOR ( 'NONE', #84733, 1000.000000000000114 ) ;
#22646 = DIRECTION ( 'NONE',  ( 1.000000000000000000, 0.000000000000000000, 0.000000000000000000 ) ) ;
#22647 = DIRECTION ( 'NONE',  ( -0.000000000000000000, 1.000000000000000000, -0.000000000000000000 ) ) ;
#22648 = VERTEX_POINT ( 'NONE', #76964 ) ;
#22649 = CARTESIAN_POINT ( 'NONE',  ( 14.61581670307174008, 6.475225279485573360, -27.35847990810646024 ) ) ;
#22650 = EDGE_CURVE ( 'NONE', #64607, #31523, #19960, .T. ) ;
#22651 = CARTESIAN_POINT ( 'NONE',  ( -105.6228709571500559, -23.48786465467241769, 11.44779295918253759 ) ) ;
#22652 = CARTESIAN_POINT ( 'NONE',  ( -15.31764660673900558, 15.41647822393392175, 11.49999999999998934 ) ) ;
#22653 = CARTESIAN_POINT ( 'NONE',  ( -27.96875734969026084, -3.316774720514426456, -0.08597719988137648983 ) ) ;
#22654 = VECTOR ( 'NONE', #63721, 1000.000000000000000 ) ;
#22655 = CARTESIAN_POINT ( 'NONE',  ( -9.247272915838292917, -17.29429475886123768, -1.500000000000002220 ) ) ;
#22656 = CYLINDRICAL_SURFACE ( 'NONE', #97785, 0.8500000000000017542 ) ;
#22657 = VECTOR ( 'NONE', #24961, 1000.000000000000114 ) ;
#22658 = CARTESIAN_POINT ( 'NONE',  ( -41.32652706876731230, -25.23761884256712307, 3.713814482909440606 ) ) ;
#22659 = DATE_AND_TIME ( #48029, #6956 ) ;
#22660 = AXIS2_PLACEMENT_3D ( 'NONE', #20810, #98939, #76096 ) ;
#22661 = CARTESIAN_POINT ( 'NONE',  ( -91.60161349800799258, -23.48786465467241058, 11.44779295918254469 ) ) ;
#22662 = CARTESIAN_POINT ( 'NONE',  ( 3.769931535195356620, -5.876774720514429617, 21.83933825178638699 ) ) ;
#22663 = CARTESIAN_POINT ( 'NONE',  ( -10.27258457790969892, -17.75692283049141196, 11.49999999999999645 ) ) ;
#22664 = CARTESIAN_POINT ( 'NONE',  ( 30.61643171304413613, 3.478988201194511909, 27.37433008668280365 ) ) ;
#22666 = B_SPLINE_CURVE_WITH_KNOTS ( 'NONE', 3,
 ( #2403, #81523, #80013, #73413, #20108, #64829 ),
 .UNSPECIFIED., .F., .F.,
 ( 4, 2, 4 ),
 ( 1.570755371634052715E-05, 0.001396183895866087536, 0.002776660238015834278 ),
 .UNSPECIFIED. ) ;
#22665 = CARTESIAN_POINT ( 'NONE',  ( -54.52287095715006870, -23.47596703998600631, 11.44779298504229104 ) ) ;
#22667 = AXIS2_PLACEMENT_3D ( 'NONE', #27391, #66965, #41626 ) ;
#22668 = ORIENTED_EDGE ( 'NONE', *, *, #27010, .F. ) ;
#22669 = EDGE_CURVE ( 'NONE', #66017, #53781, #79269, .T. ) ;
#22670 = DIRECTION ( 'NONE',  ( 1.000000000000000000, -0.000000000000000000, 0.000000000000000000 ) ) ;
#22671 = CARTESIAN_POINT ( 'NONE',  ( -39.51912653461286595, -25.18430990892983701, 3.844034515489341608 ) ) ;
#22672 = CARTESIAN_POINT ( 'NONE',  ( -125.5222534766403726, -23.48786465467241769, 11.44779295918253581 ) ) ;
#22673 = PLANE ( 'NONE',  #45088 ) ;
#22674 = EDGE_CURVE ( 'NONE', #53590, #39121, #52692, .T. ) ;
#22675 = CARTESIAN_POINT ( 'NONE',  ( 30.53060340732035982, -6.475225279485573360, 20.86760796525322093 ) ) ;
#22676 = CARTESIAN_POINT ( 'NONE',  ( 32.54161589056530346, 4.044086941844335925, -1.517980283019001453 ) ) ;
#22677 = CARTESIAN_POINT ( 'NONE',  ( 15.98122378838116120, 16.67787885001082770, 11.49999999999999645 ) ) ;
#22678 = CARTESIAN_POINT ( 'NONE',  ( 13.80103769381473811, 18.14473668730428813, -1.500000000000002220 ) ) ;
#22679 = CARTESIAN_POINT ( 'NONE',  ( -74.60134285719104241, -23.73766607897670511, -1.055555164236458898 ) ) ;
#22680 = DIRECTION ( 'NONE',  ( 2.439088438507244272E-15, -7.805083003223181985E-15, 1.000000000000000000 ) ) ;
#22681 = CARTESIAN_POINT ( 'NONE',  ( -119.6228709571500559, -24.64898659630368627, 1.056161002820833028 ) ) ;
#22682 = CARTESIAN_POINT ( 'NONE',  ( -4.914914792326205983, -21.87198836336805385, 11.49999999999999645 ) ) ;
#22683 = PLANE ( 'NONE',  #73852 ) ;
#22684 = DIRECTION ( 'NONE',  ( -3.773278334444166432E-23, 1.000000000000000000, 0.000000000000000000 ) ) ;
#22685 = CARTESIAN_POINT ( 'NONE',  ( -21.55542221127511482, -4.010009934288176758, 11.49999999999998934 ) ) ;
#22686 = APPROVAL ( #16807, 'UNSPECIFIED' ) ;
#22687 = CARTESIAN_POINT ( 'NONE',  ( -5.799455386767018439, -5.876774720514413630, 19.66076420632890276 ) ) ;
#22688 = CARTESIAN_POINT ( 'NONE',  ( -87.59490563179548417, -23.96169478059713498, 10.65365249895718058 ) ) ;
#22689 = CARTESIAN_POINT ( 'NONE',  ( -8.160000000000000142, -2.890508098367099432, -0.2344417481469836528 ) ) ;
#22690 = CARTESIAN_POINT ( 'NONE',  ( -78.54013620366454518, -24.65952944569304606, 1.056160979905704789 ) ) ;
#22691 = FACE_BOUND ( 'NONE', #7406, .T. ) ;
#22692 = ORIENTED_EDGE ( 'NONE', *, *, #4975, .F. ) ;
#22693 = CARTESIAN_POINT ( 'NONE',  ( -16.48689143942861079, 12.14541645011370541, 11.49999999999998934 ) ) ;
#22694 = ORIENTED_EDGE ( 'NONE', *, *, #11400, .F. ) ;
#22695 = VERTEX_POINT ( 'NONE', #64284 ) ;
#22696 = VERTEX_POINT ( 'NONE', #10463 ) ;
#22697 = ORIENTED_EDGE ( 'NONE', *, *, #21559, .T. ) ;
#22698 = CARTESIAN_POINT ( 'NONE',  ( -10.12245940999746985, -20.73198382670940987, 11.49999999999998934 ) ) ;
#22699 = CARTESIAN_POINT ( 'NONE',  ( -61.56641536606631604, -23.48783264082477018, -1.443836473390096575 ) ) ;
#22700 = CARTESIAN_POINT ( 'NONE',  ( -14.64122064730360862, 14.02963135428074004, -1.500000000000002220 ) ) ;
#22701 = ORIENTED_EDGE ( 'NONE', *, *, #83896, .T. ) ;
#22702 = CARTESIAN_POINT ( 'NONE',  ( -29.27791982133463122, -24.88714994053520257, 2.243760839632586102 ) ) ;
#22703 = CARTESIAN_POINT ( 'NONE',  ( -41.58770330147535077, -25.31575704012490746, 5.035072416868334066 ) ) ;
#22704 = B_SPLINE_CURVE_WITH_KNOTS ( 'NONE', 3,
 ( #82821, #75702, #90938, #44282 ),
 .UNSPECIFIED., .F., .F.,
 ( 4, 4 ),
 ( 0.000000000000000000, 1.000000000000000000 ),
 .UNSPECIFIED. ) ;
#22705 = DIRECTION ( 'NONE',  ( -0.000000000000000000, 1.000000000000000000, -0.000000000000000000 ) ) ;
#22706 = CARTESIAN_POINT ( 'NONE',  ( -70.49786096558409554, -24.52300882791528380, 0.6510814631126248253 ) ) ;
#22708 = VERTEX_POINT ( 'NONE', #98053 ) ;
#22707 = CARTESIAN_POINT ( 'NONE',  ( -3.722501342491481235, -21.08806747394077519, 11.49999999999999645 ) ) ;
#22709 = CARTESIAN_POINT ( 'NONE',  ( -110.5228709571500616, -29.50248528299804818, 1.056150453629043584 ) ) ;
#22710 = CARTESIAN_POINT ( 'NONE',  ( -61.61076051278942600, -23.48786465467240703, 11.44779295918255180 ) ) ;
#22711 = VERTEX_POINT ( 'NONE', #26194 ) ;
#22712 = CARTESIAN_POINT ( 'NONE',  ( -6.500255983836059848, -19.66680810221124887, 11.49999999999998934 ) ) ;
#22713 = VECTOR ( 'NONE', #17985, 1000.000000000000114 ) ;
#22714 = EDGE_LOOP ( 'NONE', ( #95017, #74696, #8702, #82840 ) ) ;
#22716 = ORIENTED_EDGE ( 'NONE', *, *, #77814, .F. ) ;
#22715 = DIRECTION ( 'NONE',  ( -1.000000000000000000, -0.000000000000000000, -0.000000000000000000 ) ) ;
#22717 = CARTESIAN_POINT ( 'NONE',  ( -28.48001184966671673, -24.34880053053494464, 0.6176551810875480220 ) ) ;
#22718 = ORIENTED_EDGE ( 'NONE', *, *, #73861, .F. ) ;
#22719 = ORIENTED_EDGE ( 'NONE', *, *, #51229, .T. ) ;
#22720 = CARTESIAN_POINT ( 'NONE',  ( 4.692776824272364422, -5.876774720514404748, 18.67160386110882442 ) ) ;
#22721 = B_SPLINE_CURVE_WITH_KNOTS ( 'NONE', 3,
 ( #72818, #93257, #23744, #24250 ),
 .UNSPECIFIED., .F., .F.,
 ( 4, 4 ),
 ( 0.000000000000000000, 1.000000000000000000 ),
 .UNSPECIFIED. ) ;
#22722 = CARTESIAN_POINT ( 'NONE',  ( 27.86270917940689174, -0.3587747205144265483, 29.49402280011862487 ) ) ;
#22723 = CARTESIAN_POINT ( 'NONE',  ( 12.42595048307055983, -18.10569578304522764, 11.49999999999999645 ) ) ;
#22724 = CARTESIAN_POINT ( 'NONE',  ( -89.59156183601115231, -24.15620529776628445, 10.23563542870660115 ) ) ;
#22725 = CARTESIAN_POINT ( 'NONE',  ( 22.42242567092132433, 2.420433022335332751, -1.500000000000002220 ) ) ;
#22726 = CARTESIAN_POINT ( 'NONE',  ( -19.40599490818632233, 7.965113791304038848, -1.500000000000002220 ) ) ;
#22727 = CARTESIAN_POINT ( 'NONE',  ( -48.55620429048338593, -23.48783264082478794, -1.443836473390069708 ) ) ;
#22728 = CARTESIAN_POINT ( 'NONE',  ( 6.377880655330028681, -6.376774720514424288, 21.48000012937543346 ) ) ;
#22729 = ORIENTED_EDGE ( 'NONE', *, *, #9119, .T. ) ;
#22730 = VECTOR ( 'NONE', #24756, 1000.000000000000000 ) ;
#22731 = EDGE_CURVE ( 'NONE', #26599, #50012, #9968, .T. ) ;
#22732 = EDGE_LOOP ( 'NONE', ( #39811, #39204, #1392, #89937, #67563 ) ) ;
#22733 = CIRCLE ( 'NONE', #51881, 132.8284398600581824 ) ;
#22734 = VERTEX_POINT ( 'NONE', #5222 ) ;
#22735 = EDGE_CURVE ( 'NONE', #27980, #65683, #24820, .T. ) ;
#22736 = CARTESIAN_POINT ( 'NONE',  ( -36.62287095715006302, -23.96127896941631619, -0.6493128931037911444 ) ) ;
#22737 = AXIS2_PLACEMENT_3D ( 'NONE', #21763, #21268, #92783 ) ;
#22738 = CARTESIAN_POINT ( 'NONE',  ( -17.55493245422511350, -12.44833567967518029, -1.500000000000002220 ) ) ;
#22739 = VECTOR ( 'NONE', #84607, 1000.000000000000000 ) ;
#22740 = CARTESIAN_POINT ( 'NONE',  ( -90.62287095715004170, -24.99156045073392818, 7.747789690856161648 ) ) ;
#22741 = ORIENTED_EDGE ( 'NONE', *, *, #75754, .T. ) ;
#22742 = CARTESIAN_POINT ( 'NONE',  ( -21.09505027744838657, -1.104435277493458045, 11.49999999999998934 ) ) ;
#22743 = PLANE ( 'NONE',  #49810 ) ;
#22744 = CARTESIAN_POINT ( 'NONE',  ( -129.6228709571500417, -23.47593901973091235, -1.443836447538995760 ) ) ;
#22745 = CARTESIAN_POINT ( 'NONE',  ( -83.58827326063148178, -24.35071581493543036, 9.817618358456028815 ) ) ;
#22746 = B_SPLINE_CURVE_WITH_KNOTS ( 'NONE', 3,
 ( #30936, #71517, #62914, #25324, #16210, #71013 ),
 .UNSPECIFIED., .F., .F.,
 ( 4, 2, 4 ),
 ( 6.384118678609748304E-06, 0.001386860460828372816, 0.002767336802978135821 ),
 .UNSPECIFIED. ) ;
#22747 = CARTESIAN_POINT ( 'NONE',  ( -33.62287095715005592, -29.50250786944525672, 11.44777988621624409 ) ) ;
#22748 = CARTESIAN_POINT ( 'NONE',  ( -99.12737035893434268, -25.25749934748553827, 3.919097026091935110 ) ) ;
#22749 = CARTESIAN_POINT ( 'NONE',  ( 21.13975321936677787, -6.629177502137091338, -1.500000000000002220 ) ) ;
#22750 = CARTESIAN_POINT ( 'NONE',  ( -71.55916548094597829, -23.73766607897670156, -1.055555164236456012 ) ) ;
#22751 = EDGE_CURVE ( 'NONE', #95088, #67931, #61146, .T. ) ;
#22752 = VERTEX_POINT ( 'NONE', #78967 ) ;
#22753 = CARTESIAN_POINT ( 'NONE',  ( -51.60144572864662393, -25.31633170366855978, 5.335377950845888506 ) ) ;
#22754 = CARTESIAN_POINT ( 'NONE',  ( -39.44687923781921057, -25.27828342519987359, 4.188173683033348027 ) ) ;
#22755 = CARTESIAN_POINT ( 'NONE',  ( 30.53060340732035982, 4.905668307171742626, 14.33114642260468585 ) ) ;
#22756 = LINE ( 'NONE', #16156, #5831 ) ;
#22757 = CARTESIAN_POINT ( 'NONE',  ( 5.650214204171827070, -18.61605495904187535, -1.500000000000002220 ) ) ;
#22758 = CARTESIAN_POINT ( 'NONE',  ( 15.12546962493697933, 15.13007008128210096, -1.500000000000002220 ) ) ;
#22759 = CARTESIAN_POINT ( 'NONE',  ( -62.63183165261912677, -24.34968618360933945, 0.1864209137778799485 ) ) ;
#22760 = FACE_OUTER_BOUND ( 'NONE', #56937, .T. ) ;
#22761 = B_SPLINE_CURVE_WITH_KNOTS ( 'NONE', 3,
 ( #51632, #26793, #43026, #50139 ),
 .UNSPECIFIED., .F., .F.,
 ( 4, 4 ),
 ( 0.4590962244662299963, 0.4600969715069954669 ),
 .UNSPECIFIED. ) ;
#22762 = CARTESIAN_POINT ( 'NONE',  ( -122.5895376238167387, -24.64965694238408034, 8.947790433994649462 ) ) ;
#22763 = PLANE ( 'NONE',  #15217 ) ;
#22764 = CARTESIAN_POINT ( 'NONE',  ( 22.61316900856233403, 2.020702135111208442, -1.500000000000002220 ) ) ;
#22765 = FACE_OUTER_BOUND ( 'NONE', #94664, .T. ) ;
#22766 = CARTESIAN_POINT ( 'NONE',  ( -57.62287095714999907, -23.96177878511307568, 10.65340807706330573 ) ) ;
#22767 = CARTESIAN_POINT ( 'NONE',  ( 18.95923836289803788, 5.684714004613049987, 11.49999999999999645 ) ) ;
#22768 = LINE ( 'NONE', #52746, #98245 ) ;
#22769 = VERTEX_POINT ( 'NONE', #12322 ) ;
#22770 = CARTESIAN_POINT ( 'NONE',  ( 14.61581670307174008, -2.682774720514426559, -27.35847990810646024 ) ) ;
#22771 = CARTESIAN_POINT ( 'NONE',  ( -11.16000000000000014, -9.652339641703484574, 1.628518864987183790 ) ) ;
#22772 = CARTESIAN_POINT ( 'NONE',  ( 12.90450488963236353, -17.39418326053592168, -1.500000000000002220 ) ) ;
#22773 = DIRECTION ( 'NONE',  ( -0.000000000000000000, -0.000000000000000000, -1.000000000000000000 ) ) ;
#22774 = CARTESIAN_POINT ( 'NONE',  ( -13.34961138979462270, 14.11212085816309880, -1.500000000000002220 ) ) ;
#22775 = PLANE ( 'NONE',  #98287 ) ;
#22776 = CARTESIAN_POINT ( 'NONE',  ( -35.62287095715005592, -25.00158670708908915, 2.256160236439166855 ) ) ;
#22777 = CARTESIAN_POINT ( 'NONE',  ( -12.90690225449951001, 15.05119527412115055, -1.500000000000002220 ) ) ;
#22778 = EDGE_CURVE ( 'NONE', #10925, #43589, #53200, .T. ) ;
#22779 = ORIENTED_EDGE ( 'NONE', *, *, #58219, .T. ) ;
#22780 = CARTESIAN_POINT ( 'NONE',  ( 20.27773211485958527, -1.686570798567030183, 11.49999999999999645 ) ) ;
#22781 = PLANE ( 'NONE',  #52153 ) ;
#22782 = VECTOR ( 'NONE', #41861, 1000.000000000000000 ) ;
#22783 = EDGE_CURVE ( 'NONE', #5942, #15143, #6667, .T. ) ;
#22784 = CARTESIAN_POINT ( 'NONE',  ( 33.60604063885286052, -3.409250796720436405, -11.91850954671862617 ) ) ;
#22785 = ORIENTED_EDGE ( 'NONE', *, *, #69335, .T. ) ;
#22786 = CARTESIAN_POINT ( 'NONE',  ( -0.09811904274419530614, -21.77977188575789924, -0.5132947483565734048 ) ) ;
#22787 = FACE_OUTER_BOUND ( 'NONE', #24767, .T. ) ;
#22788 = CARTESIAN_POINT ( 'NONE',  ( -48.87380231474225667, -25.31602077158062869, 6.137091870245725111 ) ) ;
#22789 = CARTESIAN_POINT ( 'NONE',  ( -40.56083858672488418, -23.85049219812685095, 10.88485053497527488 ) ) ;
#22790 = CARTESIAN_POINT ( 'NONE',  ( -81.62287095715008434, -23.47596703998600631, 11.44779298504227860 ) ) ;
#22791 = CARTESIAN_POINT ( 'NONE',  ( -0.1815635828756200498, -20.05798930676971636, 11.49999999999998934 ) ) ;
#22792 = FACE_OUTER_BOUND ( 'NONE', #7862, .T. ) ;
#22793 = ORIENTED_EDGE ( 'NONE', *, *, #12644, .T. ) ;
#22794 = B_SPLINE_CURVE_WITH_KNOTS ( 'NONE', 3,
 ( #71260, #18965, #87988, #71766, #3759, #32688, #79860, #64173, #80872, #18465, #1751, #25579, #63669, #49437, #94589, #17972, #10862, #41311, #72270, #2759 ),
 .UNSPECIFIED., .F., .F.,
 ( 4, 2, 2, 2, 2, 2, 2, 2, 2, 4 ),
 ( 0.000000000000000000, 0.0005538341668565423736, 0.001107668333713084747, 0.001661502500569627012, 0.002215336667426169494, 0.002769170834282711977, 0.003323005001139254025, 0.003876839167995796507, 0.004153756251424071434, 0.004430673334852346795 ),
 .UNSPECIFIED. ) ;
#22795 = CARTESIAN_POINT ( 'NONE',  ( -30.64427850938830389, -23.56000036390796737, -1.497999999999532594 ) ) ;
#22796 = CIRCLE ( 'NONE', #53622, 2.499999999999998668 ) ;
#22797 = CARTESIAN_POINT ( 'NONE',  ( -1.055347110731411187, -22.84297022578905612, 11.49999999999999645 ) ) ;
#22798 = CARTESIAN_POINT ( 'NONE',  ( -22.72798930328562150, -0.2126449523330483371, -1.500000000000002220 ) ) ;
#22799 = ORIENTED_EDGE ( 'NONE', *, *, #41439, .F. ) ;
#22800 = CARTESIAN_POINT ( 'NONE',  ( 0.000000000000000000, 4.132774720514426292, 0.000000000000000000 ) ) ;
#22801 = CARTESIAN_POINT ( 'NONE',  ( -28.52287095715005094, -23.57565896798463356, -1.053490781832481460 ) ) ;
#22802 = CARTESIAN_POINT ( 'NONE',  ( -38.52792539663658999, -24.66019654487199375, 8.947790411086119278 ) ) ;
#22803 = VECTOR ( 'NONE', #65570, 1000.000000000000114 ) ;
#22804 = CARTESIAN_POINT ( 'NONE',  ( -84.52287095715006160, -24.65952944569304606, 1.056160979905698794 ) ) ;
#22805 = EDGE_CURVE ( 'NONE', #76784, #81299, #97568, .T. ) ;
#22806 = ADVANCED_FACE ( 'NONE', ( #20429 ), #71014, .F. ) ;
#22807 = CARTESIAN_POINT ( 'NONE',  ( -28.98875734969026041, 0.3587747205144265483, 25.61802280011862720 ) ) ;
#22808 = CARTESIAN_POINT ( 'NONE',  ( -111.5895376238167387, -23.47596703998600631, 11.44779298504227683 ) ) ;
#22809 = ORIENTED_EDGE ( 'NONE', *, *, #35767, .F. ) ;
#22810 = CARTESIAN_POINT ( 'NONE',  ( 3.729398819442638846, -20.01364129133569136, 11.49999999999998934 ) ) ;
#22811 = VERTEX_POINT ( 'NONE', #6985 ) ;
#22812 = CARTESIAN_POINT ( 'NONE',  ( -2.116611060711651504, 22.89395876494169002, 11.49999999999998934 ) ) ;
#22813 = DIRECTION ( 'NONE',  ( -0.000000000000000000, 2.173523156925979552E-06, -0.9999999999976378895 ) ) ;
#22815 = EDGE_LOOP ( 'NONE', ( #44700, #43076, #46603, #42936 ) ) ;
#22814 = EDGE_CURVE ( 'NONE', #86042, #27009, #84104, .T. ) ;
#22816 = CARTESIAN_POINT ( 'NONE',  ( -101.6228709571500417, -23.72773821059535493, 11.05748984161097681 ) ) ;
#22817 = CARTESIAN_POINT ( 'NONE',  ( 6.431189903846153300, -6.376774720514415407, 20.08974358974358765 ) ) ;
#22818 = CARTESIAN_POINT ( 'NONE',  ( -40.62287095715004881, -24.91544648472620338, 1.928969306349231028 ) ) ;
#22820 = EDGE_LOOP ( 'NONE', ( #53179, #98366, #33729, #54464 ) ) ;
#22819 = CARTESIAN_POINT ( 'NONE',  ( 1.764508054474889009, 21.21474994468914943, 11.49999999999999645 ) ) ;
#22821 = ORIENTED_EDGE ( 'NONE', *, *, #21584, .T. ) ;
#22822 = CARTESIAN_POINT ( 'NONE',  ( 9.120982285578694615, 20.23247719416018242, 11.49999999999998934 ) ) ;
#22823 = CARTESIAN_POINT ( 'NONE',  ( 4.765357849511589805, 20.07956653139741121, 11.49999999999998934 ) ) ;
#22824 = ORIENTED_EDGE ( 'NONE', *, *, #52103, .T. ) ;
#22825 = ORIENTED_EDGE ( 'NONE', *, *, #16120, .T. ) ;
#22826 = CARTESIAN_POINT ( 'NONE',  ( -109.4178292903974352, -25.31627359254128962, 5.278454429945570681 ) ) ;
#22827 = CARTESIAN_POINT ( 'NONE',  ( -39.22520490595655929, -25.22497507903540637, 3.518386540108912719 ) ) ;
#22828 = ORIENTED_EDGE ( 'NONE', *, *, #80633, .F. ) ;
#22829 = CARTESIAN_POINT ( 'NONE',  ( -91.59147655181246250, -24.15543982623907837, -0.2315651400026614848 ) ) ;
#22830 = VERTEX_POINT ( 'NONE', #23195 ) ;
#22831 = CARTESIAN_POINT ( 'NONE',  ( -49.52287095715006160, -23.47596703998600631, 11.44779298504229104 ) ) ;
#22832 = EDGE_CURVE ( 'NONE', #4626, #22347, #9014, .T. ) ;
#22833 = CARTESIAN_POINT ( 'NONE',  ( 32.88562546571908740, 6.376774720514426953, -5.083907541707153754 ) ) ;
#22834 = CARTESIAN_POINT ( 'NONE',  ( -4.186882374726557110, 20.40937146592452223, -1.500000000000002220 ) ) ;
#22835 = ADVANCED_FACE ( 'NONE', ( #59791 ), #20769, .T. ) ;
#22836 = CARTESIAN_POINT ( 'NONE',  ( 18.38516380405726736, -11.72527425286322611, 11.49999999999999645 ) ) ;
#22837 = CARTESIAN_POINT ( 'NONE',  ( 25.04758448870090604, -5.021277251288436716, -9.725080715181634972 ) ) ;
#22838 = CARTESIAN_POINT ( 'NONE',  ( 20.57455539870835537, 4.132774720514415634, -18.22080502500613974 ) ) ;
#22839 = CARTESIAN_POINT ( 'NONE',  ( -21.66288588771858770, -5.991481186202806342, -1.500000000000002220 ) ) ;
#22840 = CARTESIAN_POINT ( 'NONE',  ( -38.66562564847060912, -23.48783264082477729, -1.443836473390076369 ) ) ;
#22841 = ORIENTED_EDGE ( 'NONE', *, *, #4947, .T. ) ;
#22842 = CARTESIAN_POINT ( 'NONE',  ( -75.62287095715005592, -29.50247984919015209, -1.443849546365053582 ) ) ;
#22843 = PLANE ( 'NONE',  #42661 ) ;
#22844 = ORIENTED_EDGE ( 'NONE', *, *, #57554, .F. ) ;
#22845 = ORIENTED_EDGE ( 'NONE', *, *, #77524, .T. ) ;
#22846 = B_SPLINE_CURVE_WITH_KNOTS ( 'NONE', 3,
 ( #96077, #43297, #42314, #81352 ),
 .UNSPECIFIED., .F., .F.,
 ( 4, 4 ),
 ( 0.04982150079182124519, 0.05882793206393686913 ),
 .UNSPECIFIED. ) ;
#22847 = VECTOR ( 'NONE', #67730, 1000.000000000000114 ) ;
#22848 = EDGE_CURVE ( 'NONE', #65188, #24519, #46583, .T. ) ;
#22849 = ORIENTED_EDGE ( 'NONE', *, *, #14736, .F. ) ;
#22850 = CARTESIAN_POINT ( 'NONE',  ( -21.15786647118399699, 2.672229404501205163, -1.500000000000002220 ) ) ;
#22851 = EDGE_CURVE ( 'NONE', #82017, #67705, #45062, .T. ) ;
#22852 = ORIENTED_EDGE ( 'NONE', *, *, #61193, .T. ) ;
#22853 = CARTESIAN_POINT ( 'NONE',  ( -19.96636262075925927, 6.592627302904066511, 11.49999999999998934 ) ) ;
#22854 = PLANE ( 'NONE',  #41695 ) ;
#22855 = CARTESIAN_POINT ( 'NONE',  ( 15.03452642382691629, -3.688048319827653021, -27.40128341529669598 ) ) ;
#22856 = LINE ( 'NONE', #68069, #25555 ) ;
#22857 = CARTESIAN_POINT ( 'NONE',  ( -4.682628417673765142, 21.48327871026360114, -1.500000000000002220 ) ) ;
#22858 = LINE ( 'NONE', #544, #62538 ) ;
#22859 = EDGE_LOOP ( 'NONE', ( #48601, #61946, #89391, #52412 ) ) ;
#22860 = CARTESIAN_POINT ( 'NONE',  ( -39.22287095715006444, -23.47593901973090524, -1.443836447538998202 ) ) ;
#22861 = ADVANCED_FACE ( 'NONE', ( #83598 ), #28826, .F. ) ;
#22862 = CARTESIAN_POINT ( 'NONE',  ( -127.6228709571500559, -23.47596703998600631, 11.44779298504227860 ) ) ;
#22863 = EDGE_CURVE ( 'NONE', #43985, #42816, #67903, .T. ) ;
#22864 = DIRECTION ( 'NONE',  ( 0.000000000000000000, 0.000000000000000000, 1.000000000000000000 ) ) ;
#22865 = VECTOR ( 'NONE', #59870, 1000.000000000000114 ) ;
#22866 = CARTESIAN_POINT ( 'NONE',  ( -130.5728709571500588, -23.47593901973090524, -1.443836447538995982 ) ) ;
#22867 = CARTESIAN_POINT ( 'NONE',  ( -20.45434509553457048, -23.26101209975225004, 10.47594215909544602 ) ) ;
#22868 = CARTESIAN_POINT ( 'NONE',  ( 21.27783752795556538, -0.9766432368044721812, 11.49999999999998934 ) ) ;
#22869 = CARTESIAN_POINT ( 'NONE',  ( -31.24388727629348494, -24.86181185134534388, 1.747789972853592610 ) ) ;
#22870 = LINE ( 'NONE', #6167, #86805 ) ;
#22871 = CARTESIAN_POINT ( 'NONE',  ( -29.52287095715006160, -23.40102634903646717, 11.44779303447556629 ) ) ;
#22872 = CARTESIAN_POINT ( 'NONE',  ( -70.52287095715007581, -23.47593901973090524, -1.443836447538997092 ) ) ;
#22873 = CARTESIAN_POINT ( 'NONE',  ( 16.93931825803137414, 14.88162037096512158, -1.500000000000002220 ) ) ;
#22874 = CARTESIAN_POINT ( 'NONE',  ( -111.9711312661725913, -25.31476271379807841, 5.144092056987718209 ) ) ;
#22875 = VERTEX_POINT ( 'NONE', #84606 ) ;
#22876 = CARTESIAN_POINT ( 'NONE',  ( -99.52287095715009002, -23.47593901973090524, -1.443836447538996648 ) ) ;
#22877 = CARTESIAN_POINT ( 'NONE',  ( -14.21210043416151159, 13.53504130633199765, 11.49999999999999645 ) ) ;
#22878 = CARTESIAN_POINT ( 'NONE',  ( -28.62287095715004170, -24.35949118625558540, 0.6166262265330719750 ) ) ;
#22879 = CARTESIAN_POINT ( 'NONE',  ( -82.52287095715001897, -23.48783264083388289, -1.443836473375923690 ) ) ;
#22880 = ORIENTED_EDGE ( 'NONE', *, *, #98781, .F. ) ;
#22881 = CARTESIAN_POINT ( 'NONE',  ( -88.55459174287842927, -23.96169478059713853, 10.65365249895717703 ) ) ;
#22882 = CARTESIAN_POINT ( 'NONE',  ( -124.4728709572981131, -25.40561136979900780, 5.197855858930376272 ) ) ;
#22883 = CARTESIAN_POINT ( 'NONE',  ( -91.96540889688385789, -25.22174524493127379, 6.695141717414600180 ) ) ;
#22884 = CARTESIAN_POINT ( 'NONE',  ( -6.756748142665309764, -18.51622224137248907, 11.49999999999998934 ) ) ;
#22885 = ORIENTED_EDGE ( 'NONE', *, *, #91593, .T. ) ;
#22886 = CARTESIAN_POINT ( 'NONE',  ( 6.783277368979140576, 6.376774720515100192, -28.31678455572487252 ) ) ;
#22887 = CARTESIAN_POINT ( 'NONE',  ( -69.62287095715005592, -29.50248528299804818, 1.056150453629036701 ) ) ;
#22888 = EDGE_CURVE ( 'NONE', #10502, #41620, #99806, .T. ) ;
#22889 = APPROVAL_ROLE ( '' ) ;
#22890 = ADVANCED_FACE ( 'NONE', ( #92706 ), #7475, .T. ) ;
#22891 = ORIENTED_EDGE ( 'NONE', *, *, #60573, .T. ) ;
#22892 = CARTESIAN_POINT ( 'NONE',  ( -96.52287095715006160, -24.64898659630528499, 1.056161002820829697 ) ) ;
#22893 = CARTESIAN_POINT ( 'NONE',  ( -107.6228709571501128, -24.34917612406838572, 0.1852690917426684236 ) ) ;
#22894 = CARTESIAN_POINT ( 'NONE',  ( -29.62287095715004881, -23.40875089534885589, 11.44779299594469713 ) ) ;
#22895 = CARTESIAN_POINT ( 'NONE',  ( 32.65434780274890159, -3.991214330829748747, -3.988850826987774489 ) ) ;
#22896 = CARTESIAN_POINT ( 'NONE',  ( -1.438454482798693146, -5.876774720514410077, 19.55848054040323092 ) ) ;
#22897 = FACE_OUTER_BOUND ( 'NONE', #89160, .T. ) ;
#22898 = DIRECTION ( 'NONE',  ( -0.000000000000000000, 1.000000000000000000, -0.000000000000000000 ) ) ;
#22899 = CARTESIAN_POINT ( 'NONE',  ( 10.22567584263966722, 17.17405255344276682, -1.500000000000002220 ) ) ;
#22900 = FACE_OUTER_BOUND ( 'NONE', #41366, .T. ) ;
#22901 = CARTESIAN_POINT ( 'NONE',  ( -101.5228709571500758, -29.50247984919015209, -1.443849546365050029 ) ) ;
#22902 = ORIENTED_EDGE ( 'NONE', *, *, #13587, .T. ) ;
#22903 = FACE_OUTER_BOUND ( 'NONE', #39313, .T. ) ;
#22904 = CARTESIAN_POINT ( 'NONE',  ( -110.0449441895338509, -25.18430161695049918, 3.330200698182170793 ) ) ;
#22905 = CARTESIAN_POINT ( 'NONE',  ( -35.67968232430675357, -23.48783264082477729, -1.443836473390077701 ) ) ;
#22906 = DIRECTION ( 'NONE',  ( 1.000000000000000000, -0.000000000000000000, -0.000000000000000000 ) ) ;
#22907 = AXIS2_PLACEMENT_3D ( 'NONE', #64264, #70349, #47518 ) ;
#22908 = CARTESIAN_POINT ( 'NONE',  ( -97.62287095715004170, -24.65952944569304606, 1.056160979905701236 ) ) ;
#22909 = DIRECTION ( 'NONE',  ( -1.000000000000000000, 0.000000000000000000, 0.000000000000000000 ) ) ;
#22910 = EDGE_CURVE ( 'NONE', #88368, #21992, #44681, .T. ) ;
#22911 = CARTESIAN_POINT ( 'NONE',  ( -61.62287095715004881, -23.47593901973091235, -1.443836447539007972 ) ) ;
#22912 = CARTESIAN_POINT ( 'NONE',  ( 5.742690948595683409, -5.876774720514426953, 21.62260900090680593 ) ) ;
#22913 = VERTEX_POINT ( 'NONE', #8488 ) ;
#22914 = CARTESIAN_POINT ( 'NONE',  ( -16.53579703214142427, -11.71821515807347680, 11.49999999999998934 ) ) ;
#22915 = FACE_OUTER_BOUND ( 'NONE', #20527, .T. ) ;
#22916 = CARTESIAN_POINT ( 'NONE',  ( -0.02075734969026423599, -6.475225279485573360, -28.54397719988136828 ) ) ;
#22917 = ADVANCED_FACE ( 'NONE', ( #47060 ), #79993, .T. ) ;
#22918 = ADVANCED_FACE ( 'NONE', ( #71899 ), #35364, .T. ) ;
#22919 = FACE_OUTER_BOUND ( 'NONE', #57447, .T. ) ;
#22920 = EDGE_CURVE ( 'NONE', #22830, #17879, #10480, .T. ) ;
#22921 = ORIENTED_EDGE ( 'NONE', *, *, #32616, .T. ) ;
#22922 = DIRECTION ( 'NONE',  ( 3.773278334444167608E-23, -1.000000000000000000, 0.000000000000000000 ) ) ;
#22923 = AXIS2_PLACEMENT_3D ( 'NONE', #88445, #56508, #33146 ) ;
#22924 = CARTESIAN_POINT ( 'NONE',  ( 19.84801528777503776, 3.447069022702595742, -1.500000000000002220 ) ) ;
#22925 = CARTESIAN_POINT ( 'NONE',  ( 16.02493003730957000, -13.65669227992738577, 11.49999999999999645 ) ) ;
#22927 = ADVANCED_FACE ( 'NONE', ( #41441 ), #57218, .T. ) ;
#22926 = LOCAL_TIME ( 0, 54, 15.00000000000000000, #825 ) ;
#22928 = DIRECTION ( 'NONE',  ( -3.773278334453079618E-23, 0.9999999999976377785, 2.173523156925979975E-06 ) ) ;
#22929 = CARTESIAN_POINT ( 'NONE',  ( 20.41560922187292348, 8.460057656491983380, 11.49999999999998934 ) ) ;
#22930 = B_SPLINE_CURVE_WITH_KNOTS ( 'NONE', 3,
 ( #23857, #54833, #85768, #16255 ),
 .UNSPECIFIED., .F., .F.,
 ( 4, 4 ),
 ( 0.000000000000000000, 9.999999999998897304E-05 ),
 .UNSPECIFIED. ) ;
#22931 = CARTESIAN_POINT ( 'NONE',  ( 20.20254288951482735, -3.758238384022974277, -1.500000000000002220 ) ) ;
#22932 = CARTESIAN_POINT ( 'NONE',  ( -98.62287095715011276, -23.73934037231758154, 11.05740245334328975 ) ) ;
#22933 = CARTESIAN_POINT ( 'NONE',  ( 16.15056352287345476, 3.622774720514426949, -27.77856273171767398 ) ) ;
#22934 = ORIENTED_EDGE ( 'NONE', *, *, #41140, .T. ) ;
#22935 = CARTESIAN_POINT ( 'NONE',  ( 22.33191539159816585, 3.407774720514426647, -16.26852658953824360 ) ) ;
#22936 = ORIENTED_EDGE ( 'NONE', *, *, #79331, .T. ) ;
#22937 = CARTESIAN_POINT ( 'NONE',  ( 0.3910256410256383042, -5.876774720514409189, 19.19230769230768985 ) ) ;
#22938 = DIRECTION ( 'NONE',  ( 0.2488812114211666759, 0.000000000000000000, 0.9685340172660599212 ) ) ;
#22939 = ORIENTED_EDGE ( 'NONE', *, *, #50517, .F. ) ;
#22940 = ORIENTED_EDGE ( 'NONE', *, *, #79675, .F. ) ;
#22941 = ORIENTED_EDGE ( 'NONE', *, *, #12707, .T. ) ;
#22942 = CARTESIAN_POINT ( 'NONE',  ( 32.88562546571908740, -0.3587747205144265483, -5.083907541707153754 ) ) ;
#22943 = CARTESIAN_POINT ( 'NONE',  ( 30.00738719773716667, -1.682774720514426114, -9.049252915307089751 ) ) ;
#22944 = LINE ( 'NONE', #61049, #95769 ) ;
#22945 = CARTESIAN_POINT ( 'NONE',  ( 1.647368763193059582, 20.57021071130147405, -1.500000000000002220 ) ) ;
#22946 = ADVANCED_FACE ( 'NONE', ( #57673 ), #88616, .T. ) ;
#22947 = ADVANCED_FACE ( 'NONE', ( #12480 ), #43448, .T. ) ;
#22948 = CARTESIAN_POINT ( 'NONE',  ( 15.64208908530913256, 14.88810259432246852, 11.49999999999999645 ) ) ;
#22949 = VERTEX_POINT ( 'NONE', #3394 ) ;
#22950 = CARTESIAN_POINT ( 'NONE',  ( -83.62287095715005592, -23.72747288104442021, -1.053458166803661999 ) ) ;
#22951 = CARTESIAN_POINT ( 'NONE',  ( 27.86270917940689174, 6.376774720514426953, 29.02104833056109001 ) ) ;
#22952 = CARTESIAN_POINT ( 'NONE',  ( -4.763361739610138201, -21.85411462188651299, 11.49999999999998934 ) ) ;
#22953 = CARTESIAN_POINT ( 'NONE',  ( -80.45048864170028935, -25.27875090593738960, 7.100579934607695876 ) ) ;
#22954 = CARTESIAN_POINT ( 'NONE',  ( -53.52287095715006160, -23.72747288104469732, -1.053458166803227458 ) ) ;
#22955 = ORIENTED_EDGE ( 'NONE', *, *, #31456, .T. ) ;
#22956 = CARTESIAN_POINT ( 'NONE',  ( -116.6622629653596448, -25.38372066892256740, 5.756446416874773320 ) ) ;
#22957 = CARTESIAN_POINT ( 'NONE',  ( -49.56823440250532542, -23.48786465467241058, 11.44779295918254824 ) ) ;
#22958 = FACE_OUTER_BOUND ( 'NONE', #85187, .T. ) ;
#22959 = CARTESIAN_POINT ( 'NONE',  ( -20.37482282770194075, 4.769447832466558346, 11.49999999999998934 ) ) ;
#22960 = ORIENTED_EDGE ( 'NONE', *, *, #85156, .T. ) ;
#22962 = ADVANCED_FACE ( 'NONE', ( #20088 ), #10182, .T. ) ;
#22961 = CARTESIAN_POINT ( 'NONE',  ( -98.62287095715005592, -23.47593901973091235, -1.443836447539001089 ) ) ;
#22963 = ORIENTED_EDGE ( 'NONE', *, *, #85517, .F. ) ;
#22964 = AXIS2_PLACEMENT_3D ( 'NONE', #74551, #98878, #52717 ) ;
#22965 = DIRECTION ( 'NONE',  ( -1.000000000000000000, -3.773278334444166432E-23, -8.201307841325785021E-29 ) ) ;
#22966 = CARTESIAN_POINT ( 'NONE',  ( -7.741094375770895653, -19.69850519626218599, -1.500000000000002220 ) ) ;
#22967 = ADVANCED_FACE ( 'NONE', ( #59165 ), #3890, .T. ) ;
#22968 = ORIENTED_EDGE ( 'NONE', *, *, #40369, .T. ) ;
#22969 = CARTESIAN_POINT ( 'NONE',  ( -117.5545766209327070, -24.15543982623907837, -0.2315651400026547124 ) ) ;
#22970 = DIRECTION ( 'NONE',  ( 0.000000000000000000, -0.000000000000000000, -1.000000000000000000 ) ) ;
#22971 = CARTESIAN_POINT ( 'NONE',  ( -14.02725853290852243, 16.66567569088042688, -1.500000000000002220 ) ) ;
#22972 = CARTESIAN_POINT ( 'NONE',  ( -37.62287095715007013, -23.47596703998600276, 11.44779298504227505 ) ) ;
#22973 = CARTESIAN_POINT ( 'NONE',  ( -41.52287095715006870, -24.33832256527048088, 0.1851278514138547937 ) ) ;
#22974 = CARTESIAN_POINT ( 'NONE',  ( -79.92287095715006728, -23.47593901973090169, -1.443836447538997092 ) ) ;
#22975 = CARTESIAN_POINT ( 'NONE',  ( -19.11951126197014261, -10.51958540666066533, -1.500000000000002220 ) ) ;
#22976 = CARTESIAN_POINT ( 'NONE',  ( -71.60837349177994327, -25.24674223047061261, 5.637668537290724480 ) ) ;
#22977 = VERTEX_POINT ( 'NONE', #58172 ) ;
#22978 = CARTESIAN_POINT ( 'NONE',  ( 25.43734433117264615, 5.179209770121858902, -8.122553904655967827 ) ) ;
#22979 = CARTESIAN_POINT ( 'NONE',  ( -117.5228709571500758, -23.47593901973090524, -1.443836447538996204 ) ) ;
#22980 = CARTESIAN_POINT ( 'NONE',  ( 30.79432203307449711, -6.272817126675294119, 0.6151397435758989563 ) ) ;
#22982 = ORIENTED_EDGE ( 'NONE', *, *, #65035, .F. ) ;
#22981 = EDGE_CURVE ( 'NONE', #34332, #66516, #44652, .T. ) ;
#22983 = EDGE_CURVE ( 'NONE', #38301, #37020, #4384, .T. ) ;
#22984 = ORIENTED_EDGE ( 'NONE', *, *, #71207, .F. ) ;
#22985 = EDGE_CURVE ( 'NONE', #80749, #59957, #80980, .T. ) ;
#22986 = EDGE_LOOP ( 'NONE', ( #85774, #13608, #55341, #46731 ) ) ;
#22987 = B_SPLINE_CURVE_WITH_KNOTS ( 'NONE', 3,
 ( #12684, #96433, #57893, #36026 ),
 .UNSPECIFIED., .F., .F.,
 ( 4, 4 ),
 ( 0.000000000000000000, 1.000000000000000000 ),
 .UNSPECIFIED. ) ;
#22988 = CARTESIAN_POINT ( 'NONE',  ( -63.58953762381671027, -23.48783264082478084, -1.443836473390069042 ) ) ;
#22989 = CARTESIAN_POINT ( 'NONE',  ( -1.563627757057377110, -21.15500258984412696, 11.49999999999998934 ) ) ;
#22990 = AXIS2_PLACEMENT_3D ( 'NONE', #95561, #25549, #65638 ) ;
#22991 = CARTESIAN_POINT ( 'NONE',  ( -95.62287095715005592, -23.47593901973091235, -1.443836447539001089 ) ) ;
#22992 = CARTESIAN_POINT ( 'NONE',  ( -80.47485683444980964, -25.03138299481809881, 7.562833672617995440 ) ) ;
#22993 = DIRECTION ( 'NONE',  ( -0.000000000000000000, -1.000000000000000000, -0.000000000000000000 ) ) ;
#22994 = CARTESIAN_POINT ( 'NONE',  ( -52.52287095715009713, -23.48783264083416356, -1.443836473375487151 ) ) ;
#22995 = CARTESIAN_POINT ( 'NONE',  ( -16.24122463664219396, 10.56255597858309869, -1.500000000000002220 ) ) ;
#22996 = ADVANCED_FACE ( 'NONE', ( #60174, #52547 ), #76359, .F. ) ;
#22997 = FACE_BOUND ( 'NONE', #17103, .T. ) ;
#22998 = ORIENTED_EDGE ( 'NONE', *, *, #84369, .F. ) ;
#22999 = CARTESIAN_POINT ( 'NONE',  ( -17.65537929698502495, 8.214918384300796461, 11.49999999999999645 ) ) ;
#23000 = PLANE ( 'NONE',  #16298 ) ;
#23001 = DIRECTION ( 'NONE',  ( -0.8264557562326033668, 6.845827386180409975E-16, -0.5630016722799281448 ) ) ;
#23002 = ORIENTED_EDGE ( 'NONE', *, *, #64627, .F. ) ;
#23003 = CARTESIAN_POINT ( 'NONE',  ( 23.57151214508650128, 3.870844576848782668E-15, 0.5000000000000000000 ) ) ;
#23004 = CARTESIAN_POINT ( 'NONE',  ( -70.43033145357846081, -25.30470252700990130, 4.855686547977941636 ) ) ;
#23005 = CARTESIAN_POINT ( 'NONE',  ( -31.52287095715006160, -29.50248528299804818, 1.056150453629029817 ) ) ;
#23006 = AXIS2_PLACEMENT_3D ( 'NONE', #63482, #9165, #24389 ) ;
#23007 = CARTESIAN_POINT ( 'NONE',  ( -34.55620429048339304, -23.48786465467240347, 11.44779295918255713 ) ) ;
#23008 = CARTESIAN_POINT ( 'NONE',  ( 5.117700956428186565, 18.95590836763280862, 11.49999999999998934 ) ) ;
#23009 = CARTESIAN_POINT ( 'NONE',  ( -40.99816688406356491, -25.27806108203015967, 4.936760908640943413 ) ) ;
#23011 = ORIENTED_EDGE ( 'NONE', *, *, #12539, .T. ) ;
#23010 = APPROVAL_PERSON_ORGANIZATION ( #43893, #488, #75324 ) ;
#23012 = CARTESIAN_POINT ( 'NONE',  ( 5.819084965910729323, 20.79142713412266730, -1.500000000000002220 ) ) ;
#23013 = CARTESIAN_POINT ( 'NONE',  ( 8.160000000000000142, -6.927494035009244411E-16, 6.788828319098143105 ) ) ;
#23014 = CARTESIAN_POINT ( 'NONE',  ( -40.57482487591116893, -24.92564183028978775, 1.928384488918254203 ) ) ;
#23015 = DIRECTION ( 'NONE',  ( 0.000000000000000000, 0.000000000000000000, 1.000000000000000000 ) ) ;
#23016 = CARTESIAN_POINT ( 'NONE',  ( -19.45891602060003578, 12.32625358835968576, -1.500000000000002220 ) ) ;
#23017 = APPROVAL_STATUS ( 'not_yet_approved' ) ;
#23018 = CARTESIAN_POINT ( 'NONE',  ( -126.6228709571500559, -23.47593901973091235, -1.443836447538995760 ) ) ;
#23019 = CARTESIAN_POINT ( 'NONE',  ( 4.415069475862049231, -6.376774720514424288, 21.13806644168711557 ) ) ;
#23020 = CARTESIAN_POINT ( 'NONE',  ( -121.5532436822344664, -24.66019654487200441, 8.947790411086119278 ) ) ;
#23021 = CARTESIAN_POINT ( 'NONE',  ( -101.8589946837564639, -25.21195325642122498, 6.589545632284776744 ) ) ;
#23022 = B_SPLINE_CURVE_WITH_KNOTS ( 'NONE', 3,
 ( #66929, #45583, #7007, #37954, #30338, #53698 ),
 .UNSPECIFIED., .F., .F.,
 ( 4, 2, 4 ),
 ( 0.000000000000000000, 0.001380764517853252287, 0.002761529035706504574 ),
 .UNSPECIFIED. ) ;
#23023 = CARTESIAN_POINT ( 'NONE',  ( -111.2413225215033634, -25.10921443801264985, 3.153769387664755008 ) ) ;
#23024 = CARTESIAN_POINT ( 'NONE',  ( -129.5558834519471247, -24.15543982623907482, -0.2315651400026527140 ) ) ;
#23025 = CARTESIAN_POINT ( 'NONE',  ( -99.12822588951706848, -25.26400712817571304, 4.142262319587673325 ) ) ;
#23026 = CARTESIAN_POINT ( 'NONE',  ( 12.81631318294326505, -15.22695477405695996, -1.500000000000002220 ) ) ;
#23027 = CARTESIAN_POINT ( 'NONE',  ( -32.62287095715004881, -29.50250786944525672, 11.44777988621624409 ) ) ;
#23028 = CARTESIAN_POINT ( 'NONE',  ( 10.49454761162020588, -16.79419365751139637, -1.500000000000002220 ) ) ;
#23029 = CARTESIAN_POINT ( 'NONE',  ( 0.3791100739519297491, -5.876774720514418959, 20.35309744218306349 ) ) ;
#23030 = CARTESIAN_POINT ( 'NONE',  ( 14.76093561896379214, 5.965225279485572685, -26.55548769130089681 ) ) ;
#23031 = CARTESIAN_POINT ( 'NONE',  ( -37.52287095715006870, -24.65952944569304250, 1.056160979905691910 ) ) ;
#23032 = CARTESIAN_POINT ( 'NONE',  ( -17.53982812869053731, -11.02811673548155902, 11.49999999999999645 ) ) ;
#23033 = CARTESIAN_POINT ( 'NONE',  ( -7.641025641025641413, -5.876774720514418071, 20.36458333333334636 ) ) ;
#23034 = B_SPLINE_CURVE_WITH_KNOTS ( 'NONE', 3,
 ( #37541, #68491, #35800, #1988, #32427, #63907, #33930, #72003 ),
 .UNSPECIFIED., .F., .F.,
 ( 4, 2, 2, 4 ),
 ( 0.003348119353445774479, 0.004405762884006169181, 0.005463406414566563882, 0.007578693475687353284 ),
 .UNSPECIFIED. ) ;
#23035 = CARTESIAN_POINT ( 'NONE',  ( -49.76870215116556295, -25.25138707665752236, 5.358736815735848147 ) ) ;
#23036 = CARTESIAN_POINT ( 'NONE',  ( 5.860688371469950475, 21.97560254587667217, 11.49999999999999645 ) ) ;
#23037 = VECTOR ( 'NONE', #25128, 1000.000000000000000 ) ;
#23039 = EDGE_CURVE ( 'NONE', #32574, #50853, #91099, .T. ) ;
#23038 = ORIENTED_EDGE ( 'NONE', *, *, #68951, .F. ) ;
#23040 = B_SPLINE_SURFACE_WITH_KNOTS ( 'NONE', 3, 1, ( 
 ( #8781, #85391 ),
 ( #15881, #46846 ),
 ( #77765, #661 ),
 ( #62575, #87910 ),
 ( #65099, #89405 ),
 ( #41749, #49866 ),
 ( #4175, #18885 ),
 ( #19877, #65597 ),
 ( #43243, #50852 ),
 ( #72192, #41237 ),
 ( #19385, #11775 ),
 ( #58470, #97511 ),
 ( #35125, #81291 ),
 ( #96018, #42259 ),
 ( #81791, #11278 ),
 ( #12264, #2681 ),
 ( #79783, #34628 ),
 ( #72690, #89903 ),
 ( #33620, #88914 ) ),
 .UNSPECIFIED., .F., .F., .F.,
 ( 4, 1, 1, 1, 1, 1, 1, 1, 1, 1, 1, 1, 1, 1, 1, 1, 4 ),
 ( 2, 2 ),
 ( 0.000000000000000000, 0.06795034759975315808, 0.1332598223836991558, 0.1978002967596463879, 0.2608458295516827841, 0.3233192927503678593, 0.3862817224595723742, 0.4500615162333133634, 0.5152075844858158282, 0.5796407692199310180, 0.6418172023841524076, 0.7016924412115357335, 0.7607690981778945094, 0.8192540511346849685, 0.8787376269055532374, 0.9381582970160912138, 1.000000000000000000 ),
 ( 0.000000000000000000, 1.000000000000000000 ),
 .UNSPECIFIED. ) ;
#23041 = DIRECTION ( 'NONE',  ( -0.000000000000000000, 1.000000000000000000, -0.000000000000000000 ) ) ;
#23043 = EDGE_CURVE ( 'NONE', #78121, #68153, #21573, .T. ) ;
#23042 = CARTESIAN_POINT ( 'NONE',  ( -52.58953762381671027, -23.47596703998600276, 11.44779298504227505 ) ) ;
#23044 = CARTESIAN_POINT ( 'NONE',  ( 20.19498477198788322, 0.2509159868347127231, 11.49999999999998934 ) ) ;
#23045 = CARTESIAN_POINT ( 'NONE',  ( -93.52287095715006160, -29.50250786944525672, 11.44777988621623344 ) ) ;
#23046 = ADVANCED_FACE ( 'NONE', ( #98201 ), #95253, .T. ) ;
#23047 = DIRECTION ( 'NONE',  ( 0.000000000000000000, 0.9999999999976377785, 2.173523156925979975E-06 ) ) ;
#23048 = EDGE_CURVE ( 'NONE', #33967, #17763, #36822, .T. ) ;
#23049 = ORIENTED_EDGE ( 'NONE', *, *, #48370, .F. ) ;
#23050 = EDGE_CURVE ( 'NONE', #2140, #6243, #98708, .T. ) ;
#23051 = ORIENTED_EDGE ( 'NONE', *, *, #98841, .T. ) ;
#23052 = CARTESIAN_POINT ( 'NONE',  ( -0.3225169060639742624, -6.376774720514411854, 19.46611907402017749 ) ) ;
#23053 = CARTESIAN_POINT ( 'NONE',  ( 2.875404258304424143, 22.71175023210845012, -1.500000000000002220 ) ) ;
#23054 = CARTESIAN_POINT ( 'NONE',  ( -51.15490599271181082, -25.27420631276300966, 3.607700143673106208 ) ) ;
#23055 = CARTESIAN_POINT ( 'NONE',  ( 9.069627533930374241, 19.64968329815391712, -1.500000000000002220 ) ) ;
#23056 = CARTESIAN_POINT ( 'NONE',  ( -100.6228709571500559, -29.50250243563736774, 8.947779886222138046 ) ) ;
#23057 = CARTESIAN_POINT ( 'NONE',  ( -114.6228709571500559, -23.72747288104470087, -1.053458166803225460 ) ) ;
#23058 = AXIS2_PLACEMENT_3D ( 'NONE', #89195, #33397, #64389 ) ;
#23059 = CARTESIAN_POINT ( 'NONE',  ( -11.35812032211249090, 17.58211214940072864, 11.49999999999999645 ) ) ;
#23060 = ORIENTED_EDGE ( 'NONE', *, *, #15558, .T. ) ;
#23061 = EDGE_CURVE ( 'NONE', #74171, #73980, #34942, .T. ) ;
#23062 = CARTESIAN_POINT ( 'NONE',  ( -69.08877929746488178, -25.24754397370021053, 5.548814464877763974 ) ) ;
#23063 = CARTESIAN_POINT ( 'NONE',  ( -19.13726171168348245, 10.91495894028074432, -1.500000000000002220 ) ) ;
#23064 = CARTESIAN_POINT ( 'NONE',  ( -105.5156638583312798, -24.15602025860896163, 10.28564288303535967 ) ) ;
#23065 = CARTESIAN_POINT ( 'NONE',  ( -30.47287095715006799, -24.76053341945900499, 1.389474774145630587 ) ) ;
#23066 = ORIENTED_EDGE ( 'NONE', *, *, #3044, .F. ) ;
#23067 = CARTESIAN_POINT ( 'NONE',  ( 4.821763668436347849, -6.376774720514406525, 18.93074869776452829 ) ) ;
#23068 = DIRECTION ( 'NONE',  ( -3.773278334444166432E-23, 1.000000000000000000, 0.000000000000000000 ) ) ;
#23069 = EDGE_LOOP ( 'NONE', ( #42231, #15020, #52072, #39307 ) ) ;
#23070 = CARTESIAN_POINT ( 'NONE',  ( -72.53829674254417625, -24.66019654487199730, 8.947790411086121054 ) ) ;
#23071 = ORIENTED_EDGE ( 'NONE', *, *, #58186, .T. ) ;
#23072 = ORIENTED_EDGE ( 'NONE', *, *, #67009, .F. ) ;
#23073 = CARTESIAN_POINT ( 'NONE',  ( -71.49517126166168168, -24.66019654487199730, 8.947790411086113949 ) ) ;
#23074 = CARTESIAN_POINT ( 'NONE',  ( -83.52287095715007581, -24.50321055353804667, 9.387540953477524042 ) ) ;
#23075 = CARTESIAN_POINT ( 'NONE',  ( -4.165021623707020559, -5.876774720514417183, 20.26087634804756377 ) ) ;
#23076 = CARTESIAN_POINT ( 'NONE',  ( -18.82070947631147106, 8.064391923812276985, -1.500000000000002220 ) ) ;
#23077 = EDGE_CURVE ( 'NONE', #64230, #29229, #8858, .T. ) ;
#23078 = ORIENTED_EDGE ( 'NONE', *, *, #30522, .F. ) ;
#23079 = CARTESIAN_POINT ( 'NONE',  ( -116.5562042904833788, -24.66019654487200086, 8.947790411086121054 ) ) ;
#23080 = CARTESIAN_POINT ( 'NONE',  ( -10.37843575862113887, 5.356774720514426491, 27.71903885537846435 ) ) ;
#23081 = LINE ( 'NONE', #54072, #62920 ) ;
#23082 = CARTESIAN_POINT ( 'NONE',  ( 13.76814385225720372, 17.53657229028232223, 11.49999999999998934 ) ) ;
#23083 = B_SPLINE_CURVE_WITH_KNOTS ( 'NONE', 3,
 ( #20513, #75300, #97645, #99133, #60108, #90532 ),
 .UNSPECIFIED., .F., .F.,
 ( 4, 2, 4 ),
 ( 6.391158118952235087E-06, 0.001387004593080770317, 0.002767618028042588118 ),
 .UNSPECIFIED. ) ;
#23085 = CARTESIAN_POINT ( 'NONE',  ( -4.358143420448500116, -6.376774720514413630, 19.75705121608222115 ) ) ;
#23084 = AXIS2_PLACEMENT_3D ( 'NONE', #76918, #31256, #812 ) ;
#23086 = DIRECTION ( 'NONE',  ( -0.5473879298857849962, 5.908253122965993883E-15, -0.8368789961609472972 ) ) ;
#23087 = EDGE_CURVE ( 'NONE', #89282, #70995, #7857, .T. ) ;
#23088 = ORIENTED_EDGE ( 'NONE', *, *, #71737, .T. ) ;
#23089 = CARTESIAN_POINT ( 'NONE',  ( -27.70544111104076990, -24.60484793945295934, 1.628749883096155981 ) ) ;
#23090 = CARTESIAN_POINT ( 'NONE',  ( -29.70813536620188700, -25.26247646271292524, 6.270927263681702613 ) ) ;
#23091 = LOCAL_TIME ( 0, 54, 15.00000000000000000, #92919 ) ;
#23092 = CARTESIAN_POINT ( 'NONE',  ( -12.40256906124370673, -16.71776976679197801, -1.500000000000002220 ) ) ;
#23093 = EDGE_LOOP ( 'NONE', ( #25835, #21738, #58089, #24515 ) ) ;
#23095 = ORIENTED_EDGE ( 'NONE', *, *, #71968, .T. ) ;
#23094 = LINE ( 'NONE', #100207, #63324 ) ;
#23096 = VECTOR ( 'NONE', #25151, 1000.000000000000000 ) ;
#23097 = DIRECTION ( 'NONE',  ( -0.1254312216594016538, 0.000000000000000000, -0.9921023176230513441 ) ) ;
#23098 = ORIENTED_EDGE ( 'NONE', *, *, #75938, .F. ) ;
#23099 = ORIENTED_EDGE ( 'NONE', *, *, #89542, .T. ) ;
#23100 = PLANE ( 'NONE',  #49532 ) ;
#23101 = DIRECTION ( 'NONE',  ( 1.000000000000000000, 0.000000000000000000, 0.000000000000000000 ) ) ;
#23102 = CARTESIAN_POINT ( 'NONE',  ( 5.109298100551870725, -3.316774720514426456, -27.55941679637892250 ) ) ;
#23103 = VECTOR ( 'NONE', #56076, 1000.000000000000000 ) ;
#23104 = CARTESIAN_POINT ( 'NONE',  ( 30.93860345374796594, 6.475225279485573360, 29.23160796525321814 ) ) ;
#23105 = CARTESIAN_POINT ( 'NONE',  ( -109.8721775411165424, -25.13089038914449347, 2.890306159589083101 ) ) ;
#23106 = CARTESIAN_POINT ( 'NONE',  ( -53.52287095715008292, -23.48783264082477018, -1.443836473390094799 ) ) ;
#23108 = ORIENTED_EDGE ( 'NONE', *, *, #62024, .T. ) ;
#23107 = CARTESIAN_POINT ( 'NONE',  ( 20.56832688555235222, -8.368550285707721414, 11.49999999999999645 ) ) ;
#23109 = CARTESIAN_POINT ( 'NONE',  ( -44.62287095715005592, -23.73934037231755667, 11.05740245334329508 ) ) ;
#23110 = ORIENTED_EDGE ( 'NONE', *, *, #81738, .F. ) ;
#23111 = CARTESIAN_POINT ( 'NONE',  ( 20.84710439121840864, 8.857176948214046774, -1.500000000000002220 ) ) ;
#23112 = EDGE_CURVE ( 'NONE', #62167, #96134, #56556, .T. ) ;
#23114 = ORIENTED_EDGE ( 'NONE', *, *, #35263, .T. ) ;
#23113 = CARTESIAN_POINT ( 'NONE',  ( -115.5956212965460850, -23.48786465467241769, 11.44779295918253581 ) ) ;
#23115 = ORIENTED_EDGE ( 'NONE', *, *, #40866, .F. ) ;
#23116 = CARTESIAN_POINT ( 'NONE',  ( -112.6228709571500559, -23.47596703998600631, 11.44779298504227860 ) ) ;
#23117 = EDGE_CURVE ( 'NONE', #65831, #61715, #38559, .T. ) ;
#23118 = AXIS2_PLACEMENT_3D ( 'NONE', #80194, #47751, #71088 ) ;
#23119 = CARTESIAN_POINT ( 'NONE',  ( -18.49208213979201076, -7.923680710433813168, -1.500000000000002220 ) ) ;
#23120 = LINE ( 'NONE', #92143, #24650 ) ;
#23121 = ORIENTED_EDGE ( 'NONE', *, *, #27927, .F. ) ;
#23122 = CARTESIAN_POINT ( 'NONE',  ( -37.62287095715005592, -29.50250243563736774, 8.947779886222148704 ) ) ;
#23123 = CARTESIAN_POINT ( 'NONE',  ( 22.31825301297700648, 1.237144038376295274, -1.500000000000002220 ) ) ;
#23124 = VERTEX_POINT ( 'NONE', #33195 ) ;
#23125 = ORIENTED_EDGE ( 'NONE', *, *, #79879, .T. ) ;
#23126 = DIRECTION ( 'NONE',  ( 0.000000000000000000, 0.000000000000000000, 1.000000000000000000 ) ) ;
#23128 = CARTESIAN_POINT ( 'NONE',  ( -94.54500761342549708, -24.66019654487199730, 8.947790411086121054 ) ) ;
#23127 = VECTOR ( 'NONE', #3788, 1000.000000000000114 ) ;
#23129 = FACE_OUTER_BOUND ( 'NONE', #56042, .T. ) ;
#23130 = CARTESIAN_POINT ( 'NONE',  ( -59.52287095715006160, -24.64898659630528854, 1.056161002820822592 ) ) ;
#23131 = CARTESIAN_POINT ( 'NONE',  ( 15.14080536460164517, 5.152774720514427642, -26.62908960815038384 ) ) ;
#23132 = CARTESIAN_POINT ( 'NONE',  ( 4.865394487973861537, 18.91859722749940786, -1.500000000000002220 ) ) ;
#23133 = AXIS2_PLACEMENT_3D ( 'NONE', #42420, #81950, #66755 ) ;
#23134 = PLANE ( 'NONE',  #73348 ) ;
#23135 = CARTESIAN_POINT ( 'NONE',  ( 21.49998558720804809, 0.1351929536555107336, -1.500000000000002220 ) ) ;
#23136 = CARTESIAN_POINT ( 'NONE',  ( -62.52287095715006160, -23.48786465467241058, 11.44779295918254824 ) ) ;
#23137 = FACE_OUTER_BOUND ( 'NONE', #97868, .T. ) ;
#23138 = LINE ( 'NONE', #24646, #68467 ) ;
#23139 = PLANE ( 'NONE',  #77918 ) ;
#23140 = CARTESIAN_POINT ( 'NONE',  ( 22.22072617242880455, -5.352622178732230118, -1.500000000000002220 ) ) ;
#23141 = APPROVAL_ROLE ( '' ) ;
#23142 = DIRECTION ( 'NONE',  ( 0.8219392559241307517, 0.08114015731558495148, 0.5637660281018078701 ) ) ;
#23143 = CYLINDRICAL_SURFACE ( 'NONE', #68502, 21.89999999999999858 ) ;
#23144 = CARTESIAN_POINT ( 'NONE',  ( -4.751880754313710042, -19.48972053015312866, 11.49999999999999645 ) ) ;
#23145 = CARTESIAN_POINT ( 'NONE',  ( -2.188401442307694289, -6.376774720514411854, 19.46153846153846700 ) ) ;
#23146 = CARTESIAN_POINT ( 'NONE',  ( -118.6228709571500559, -23.47593901973091235, -1.443836447538997536 ) ) ;
#23147 = CARTESIAN_POINT ( 'NONE',  ( 6.026614999332422182E-17, -23.47594215783195537, -5.102550391006585557E-05 ) ) ;
#23148 = DIRECTION ( 'NONE',  ( -0.000000000000000000, -0.000000000000000000, 1.000000000000000000 ) ) ;
#23149 = ORIENTED_EDGE ( 'NONE', *, *, #87032, .F. ) ;
#23150 = DIRECTION ( 'NONE',  ( -0.8246584009594636333, 0.5656310827093757876, 0.000000000000000000 ) ) ;
#23151 = SPHERICAL_SURFACE ( 'NONE', #63695, 6.600000000000001421 ) ;
#23152 = CARTESIAN_POINT ( 'NONE',  ( -1.994712787082457472, 21.64621699974126656, 11.49999999999998934 ) ) ;
#23153 = CARTESIAN_POINT ( 'NONE',  ( -24.90875734969025501, -6.376774720514426953, 26.43402280011862615 ) ) ;
#23154 = CARTESIAN_POINT ( 'NONE',  ( -19.37001648656083574, -3.113731218521536004, -1.500000000000002220 ) ) ;
#23155 = CARTESIAN_POINT ( 'NONE',  ( 30.56047832681635867, 2.297196155479663826, 24.67598410064777070 ) ) ;
#23156 = VECTOR ( 'NONE', #49648, 1000.000000000000114 ) ;
#23157 = CARTESIAN_POINT ( 'NONE',  ( -109.5669895805274336, -25.31698083318981318, 4.843009121909479298 ) ) ;
#23158 = PERSON_AND_ORGANIZATION ( #83885, #84739 ) ;
#23159 = LOCAL_TIME ( 0, 54, 15.00000000000000000, #89705 ) ;
#23160 = CARTESIAN_POINT ( 'NONE',  ( -91.50904508725861319, -24.35071581493543391, 9.817618358456025263 ) ) ;
#23161 = CARTESIAN_POINT ( 'NONE',  ( 3.552327343495968570, -5.876774720514427841, 21.81288606793570395 ) ) ;
#23162 = CARTESIAN_POINT ( 'NONE',  ( 7.506095096478735407, 19.11734572241606145, 11.49999999999999645 ) ) ;
#23163 = CARTESIAN_POINT ( 'NONE',  ( 30.61558314414154580, 3.638221654638376990, 27.34201279177319321 ) ) ;
#23164 = FACE_OUTER_BOUND ( 'NONE', #37612, .T. ) ;
#23165 = CIRCLE ( 'NONE', #79895, 19.00000000000000000 ) ;
#23166 = ADVANCED_FACE ( 'NONE', ( #46424 ), #34269, .T. ) ;
#23167 = ORIENTED_EDGE ( 'NONE', *, *, #19687, .F. ) ;
#23168 = CARTESIAN_POINT ( 'NONE',  ( -83.55620429048339304, -23.47596703998600276, 11.44779298504227683 ) ) ;
#23169 = CARTESIAN_POINT ( 'NONE',  ( -69.62287095715005592, -24.65952944569304961, 1.056160979905697017 ) ) ;
#23171 = EDGE_CURVE ( 'NONE', #14525, #22171, #245, .T. ) ;
#23170 = CARTESIAN_POINT ( 'NONE',  ( -125.5540156586789067, -25.00182538069147498, 7.747789668545045139 ) ) ;
#23172 = CARTESIAN_POINT ( 'NONE',  ( -67.62287095715005592, -29.50248528299804818, 1.056150453629036701 ) ) ;
#23173 = VECTOR ( 'NONE', #82515, 1000.000000000000000 ) ;
#23174 = B_SPLINE_CURVE_WITH_KNOTS ( 'NONE', 3,
 ( #64625, #41260, #93523, #95540, #15902, #62597, #16400, #78298, #39743, #94032, #24518, #55486, #81812, #35646, #58001, #88933 ),
 .UNSPECIFIED., .F., .F.,
 ( 4, 2, 2, 2, 2, 2, 2, 4 ),
 ( 0.000000000000000000, 0.0002240477605849928056, 0.0004480955211699856112, 0.0008961910423400092779, 0.001120238802925007694, 0.001344286563510006544, 0.001568334324095004961, 0.001792382084680003811 ),
 .UNSPECIFIED. ) ;
#23175 = CARTESIAN_POINT ( 'NONE',  ( -25.81215951358583993, -24.93063326169846761, 6.831251959621990721 ) ) ;
#23176 = EDGE_CURVE ( 'NONE', #83405, #79593, #5739, .T. ) ;
#23177 = PLANE ( 'NONE',  #25316 ) ;
#23178 = B_SPLINE_CURVE_WITH_KNOTS ( 'NONE', 3,
 ( #11391, #95129, #34239, #34734 ),
 .UNSPECIFIED., .F., .F.,
 ( 4, 4 ),
 ( 0.000000000000000000, 1.000000000000000000 ),
 .UNSPECIFIED. ) ;
#23179 = EDGE_CURVE ( 'NONE', #32453, #2424, #93243, .T. ) ;
#23180 = B_SPLINE_CURVE_WITH_KNOTS ( 'NONE', 3,
 ( #42017, #88182, #4447, #18651 ),
 .UNSPECIFIED., .F., .F.,
 ( 4, 4 ),
 ( 0.000000000000000000, 1.000000000000000000 ),
 .UNSPECIFIED. ) ;
#23181 = CARTESIAN_POINT ( 'NONE',  ( -22.28253579152010033, 6.022996098971622914, 11.49999999999999645 ) ) ;
#23182 = CARTESIAN_POINT ( 'NONE',  ( 17.57702471007113232, 14.52005670271990034, -1.500000000000002220 ) ) ;
#23183 = CARTESIAN_POINT ( 'NONE',  ( -33.92287095715005307, -23.47596703998600276, 11.44779298504227683 ) ) ;
#23184 = B_SPLINE_SURFACE_WITH_KNOTS ( 'NONE', 3, 3, ( 
 ( #15188, #100401, #30914, #68485 ),
 ( #30415, #91811, #31419, #15690 ),
 ( #99420, #93304, #46656, #62376 ),
 ( #61884, #22284, #23288, #23797 ),
 ( #77575, #92311, #16186, #47156 ),
 ( #7580, #31924, #70487, #46151 ),
 ( #78073, #8585, #29914, #8080 ),
 ( #52762, #53267, #77075, #38528 ),
 ( #93815, #92806, #69486, #39027 ),
 ( #39534, #83699, #84195, #6580 ) ),
 .UNSPECIFIED., .F., .F., .F.,
 ( 4, 3, 3, 4 ),
 ( 4, 4 ),
 ( 0.0004766839783815726879, 0.1491231665100170301, 0.2234464077758347433, 0.2977696490416524844 ),
 ( 0.4995543325860023476, 0.5008647392976423030 ),
 .UNSPECIFIED. ) ;
#23185 = EDGE_CURVE ( 'NONE', #55229, #68279, #39777, .T. ) ;
#23186 = CARTESIAN_POINT ( 'NONE',  ( -5.654682302363691626, -6.376774720514410077, 19.41635569784906323 ) ) ;
#23187 = CARTESIAN_POINT ( 'NONE',  ( -64.22287095715006444, -23.47593901973090169, -1.443836447538997536 ) ) ;
#23188 = CARTESIAN_POINT ( 'NONE',  ( -20.53624283083718893, 9.024085183690161216, 11.49999999999999645 ) ) ;
#23189 = EDGE_LOOP ( 'NONE', ( #84856, #64551, #52840, #74430 ) ) ;
#23190 = CARTESIAN_POINT ( 'NONE',  ( 3.509873074917118085, 5.965225279485572685, 29.15869884040363758 ) ) ;
#23191 = EDGE_CURVE ( 'NONE', #13722, #68021, #95098, .T. ) ;
#23192 = DIRECTION ( 'NONE',  ( 0.000000000000000000, -1.000000000000000000, 0.000000000000000000 ) ) ;
#23193 = CARTESIAN_POINT ( 'NONE',  ( 20.11839708684271244, 8.774209887332036217, -1.500000000000002220 ) ) ;
#23194 = CARTESIAN_POINT ( 'NONE',  ( -113.5228709571500616, -24.65952944569304961, 1.056160979905704123 ) ) ;
#23195 = CARTESIAN_POINT ( 'NONE',  ( -45.52287095715006160, -23.48786465467240347, 11.44779295918255002 ) ) ;
#23196 = CARTESIAN_POINT ( 'NONE',  ( -104.6235422183511758, -24.65952944569305316, 1.056160979905702346 ) ) ;
#23197 = CARTESIAN_POINT ( 'NONE',  ( -78.56384845838088893, -23.48783264082477018, -1.443836473390096797 ) ) ;
#23198 = FACE_OUTER_BOUND ( 'NONE', #42599, .T. ) ;
#23199 = ORIENTED_EDGE ( 'NONE', *, *, #45425, .F. ) ;
#23200 = CARTESIAN_POINT ( 'NONE',  ( -18.53176153473302179, -8.692061069824589481, -1.500000000000002220 ) ) ;
#23201 = ORIENTED_EDGE ( 'NONE', *, *, #69853, .T. ) ;
#23202 = VERTEX_POINT ( 'NONE', #93581 ) ;
#23203 = ORIENTED_EDGE ( 'NONE', *, *, #75831, .T. ) ;
#23204 = ORIENTED_EDGE ( 'NONE', *, *, #97162, .F. ) ;
#23205 = CARTESIAN_POINT ( 'NONE',  ( -17.14199295335891904, -15.44578658782692671, -1.500000000000002220 ) ) ;
#23206 = CARTESIAN_POINT ( 'NONE',  ( -40.79613026685809274, -25.30524842186639844, 5.093185296294494790 ) ) ;
#23207 = CARTESIAN_POINT ( 'NONE',  ( 0.7445296356392017145, -20.29553345556499622, -1.500000000000002220 ) ) ;
#23208 = AXIS2_PLACEMENT_3D ( 'NONE', #35111, #3664, #96999 ) ;
#23209 = VERTEX_POINT ( 'NONE', #40807 ) ;
#23210 = CARTESIAN_POINT ( 'NONE',  ( -29.26526703061216494, -25.20409411716389769, 4.938174481708933250 ) ) ;
#23211 = CARTESIAN_POINT ( 'NONE',  ( -92.59143168555947057, -24.15543982623908192, -0.2315651400026453588 ) ) ;
#23212 = CARTESIAN_POINT ( 'NONE',  ( -101.3562811213368775, -25.19976993852609937, 6.677978858547927388 ) ) ;
#23213 = CARTESIAN_POINT ( 'NONE',  ( -65.62287095715005592, -29.50247984919015209, -1.443849546365055359 ) ) ;
#23215 = ORIENTED_EDGE ( 'NONE', *, *, #80707, .F. ) ;
#23214 = CARTESIAN_POINT ( 'NONE',  ( -11.62584540149672385, -18.10649092712023389, 11.49999999999999645 ) ) ;
#23216 = CARTESIAN_POINT ( 'NONE',  ( -75.62935843874419106, -24.73486907724918282, 1.287355809206967683 ) ) ;
#23218 = AXIS2_PLACEMENT_3D ( 'NONE', #80469, #51526, #95697 ) ;
#23217 = CARTESIAN_POINT ( 'NONE',  ( -34.62287095715004881, -24.50216790748203266, 0.6166512839542577229 ) ) ;
#23219 = ORIENTED_EDGE ( 'NONE', *, *, #62509, .F. ) ;
#23220 = CARTESIAN_POINT ( 'NONE',  ( -7.464567774302189207, 19.34240081622845153, -1.500000000000002220 ) ) ;
#23221 = ORIENTED_EDGE ( 'NONE', *, *, #39535, .F. ) ;
#23223 = EDGE_LOOP ( 'NONE', ( #39946, #75889, #44133, #43667 ) ) ;
#23222 = LINE ( 'NONE', #21718, #97725 ) ;
#23224 = CARTESIAN_POINT ( 'NONE',  ( 27.86270917940689174, -0.3587747205144265483, 29.49402280011862487 ) ) ;
#23225 = ORIENTED_EDGE ( 'NONE', *, *, #23244, .F. ) ;
#23226 = EDGE_LOOP ( 'NONE', ( #70016, #95979, #67933, #13168 ) ) ;
#23227 = CARTESIAN_POINT ( 'NONE',  ( 4.115763745420833786, -6.376774720514402972, 18.20859014712428348 ) ) ;
#23228 = CARTESIAN_POINT ( 'NONE',  ( -116.6228709571500275, -23.47596703998600631, 11.44779298504227860 ) ) ;
#23229 = CARTESIAN_POINT ( 'NONE',  ( -76.52287095715007581, -23.48786465467241769, 11.44779295918254469 ) ) ;
#23230 = CARTESIAN_POINT ( 'NONE',  ( 15.37660858059359725, 15.65766701038582021, 11.49999999999999645 ) ) ;
#23231 = CARTESIAN_POINT ( 'NONE',  ( 13.91401389203221406, 3.316774720514426456, 158.0376437107427137 ) ) ;
#23232 = CARTESIAN_POINT ( 'NONE',  ( 18.83488669200175281, -12.41447709603701632, 11.49999999999998934 ) ) ;
#23233 = CARTESIAN_POINT ( 'NONE',  ( -8.674659061502078217, -19.08593140856894621, 11.49999999999998934 ) ) ;
#23234 = CARTESIAN_POINT ( 'NONE',  ( -48.52287095715004739, -23.48783264083430211, -1.443836473375264440 ) ) ;
#23235 = VECTOR ( 'NONE', #46659, 1000.000000000000114 ) ;
#23236 = PLANE ( 'NONE',  #94556 ) ;
#23237 = VERTEX_POINT ( 'NONE', #54538 ) ;
#23238 = ORIENTED_EDGE ( 'NONE', *, *, #96962, .F. ) ;
#23239 = ORIENTED_EDGE ( 'NONE', *, *, #19652, .F. ) ;
#23240 = CARTESIAN_POINT ( 'NONE',  ( -72.52287095715007581, -24.64898659630367916, 1.056161002820824368 ) ) ;
#23241 = ADVANCED_FACE ( 'NONE', ( #94089 ), #85476, .T. ) ;
#23242 = CARTESIAN_POINT ( 'NONE',  ( -18.53595284743415661, 10.95218985133829825, -1.500000000000002220 ) ) ;
#23243 = VECTOR ( 'NONE', #58025, 1000.000000000000114 ) ;
#23244 = EDGE_CURVE ( 'NONE', #69079, #74508, #70261, .T. ) ;
#23245 = DIRECTION ( 'NONE',  ( -3.773278334453080206E-23, 0.9999999999976377785, 2.173523156925979975E-06 ) ) ;
#23246 = ORIENTED_EDGE ( 'NONE', *, *, #68061, .T. ) ;
#23247 = CARTESIAN_POINT ( 'NONE',  ( 3.428800225705347149, -20.88102749682517612, -1.500000000000002220 ) ) ;
#23248 = CARTESIAN_POINT ( 'NONE',  ( -83.58953762381673869, -24.64898659630528854, 1.056161002820828587 ) ) ;
#23249 = CARTESIAN_POINT ( 'NONE',  ( -58.85933311957388980, -25.20144863547804803, 6.835696751361012957 ) ) ;
#23250 = CARTESIAN_POINT ( 'NONE',  ( -49.51097411295445028, -25.26741039762233498, 4.038287390307901958 ) ) ;
#23251 = DIRECTION ( 'NONE',  ( 3.773278334444167608E-23, -1.000000000000000000, 0.000000000000000000 ) ) ;
#23252 = LINE ( 'NONE', #32888, #9784 ) ;
#23253 = CARTESIAN_POINT ( 'NONE',  ( 17.03105324785762420, 14.15717209551829647, -1.500000000000002220 ) ) ;
#23254 = AXIS2_PLACEMENT_3D ( 'NONE', #87415, #63605, #95031 ) ;
#23255 = CARTESIAN_POINT ( 'NONE',  ( -7.999999999999996447, -5.876774720514426953, 22.50000000000000355 ) ) ;
#23256 = ORIENTED_EDGE ( 'NONE', *, *, #49670, .F. ) ;
#23257 = CARTESIAN_POINT ( 'NONE',  ( 8.071512145086531476, -9.528487854913507249, 1.638360241832205349E-16 ) ) ;
#23258 = CARTESIAN_POINT ( 'NONE',  ( 13.35520464978777788, 3.511397109468809674, -28.20545335007043164 ) ) ;
#23259 = CARTESIAN_POINT ( 'NONE',  ( -5.843762028675351772, -18.45606589188993141, 11.49999999999999645 ) ) ;
#23260 = DIRECTION ( 'NONE',  ( -0.000000000000000000, -1.000000000000000000, -0.000000000000000000 ) ) ;
#23261 = CARTESIAN_POINT ( 'NONE',  ( 19.29218144733592055, -2.436590042558338443, 11.49999999999998934 ) ) ;
#23262 = CARTESIAN_POINT ( 'NONE',  ( -15.71168838272081558, 14.50144224353281786, 11.49999999999998934 ) ) ;
#23263 = FACE_OUTER_BOUND ( 'NONE', #1510, .T. ) ;
#23264 = DIRECTION ( 'NONE',  ( -0.1875268396392987258, -0.000000000000000000, -0.9822594791677485837 ) ) ;
#23265 = CARTESIAN_POINT ( 'NONE',  ( -40.58953762381672448, -25.00158670708908559, 2.256160236439166411 ) ) ;
#23266 = CARTESIAN_POINT ( 'NONE',  ( -100.4839344043725333, -25.18440011564083747, 3.295732011862015032 ) ) ;
#23267 = CARTESIAN_POINT ( 'NONE',  ( -22.58250372949163420, -2.080990182559540269, -1.500000000000002220 ) ) ;
#23268 = B_SPLINE_SURFACE_WITH_KNOTS ( 'NONE', 3, 3, ( 
 ( #84749, #5256, #77626, #82379 ),
 ( #36214, #70028, #43826, #28103 ),
 ( #35719, #69538, #15237, #515 ),
 ( #91861, #22829, #53817, #20 ),
 ( #67178, #14731, #77125, #15738 ),
 ( #74761, #22333, #7632, #38580 ),
 ( #59061, #62429, #92858, #85755 ) ),
 .UNSPECIFIED., .F., .F., .F.,
 ( 4, 3, 4 ),
 ( 4, 4 ),
 ( 0.0004766839783819774206, 0.1029713700210896365, 0.2054660560637973088 ),
 ( 0.3895931030775385828, 0.3907855851754823417 ),
 .UNSPECIFIED. ) ;
#23269 = CARTESIAN_POINT ( 'NONE',  ( -106.5228709571500900, -23.47593901973090524, -1.443836447538996204 ) ) ;
#23270 = CARTESIAN_POINT ( 'NONE',  ( -57.62287095715004170, -23.73934037231756733, 11.05740245334329153 ) ) ;
#23271 = CARTESIAN_POINT ( 'NONE',  ( -6.239078800006583769, 18.87631364486404806, 11.49999999999999645 ) ) ;
#23272 = APPLICATION_CONTEXT ( 'configuration controlled 3d designs of mechanical parts and assemblies' ) ;
#23273 =( BOUNDED_SURFACE ( )  B_SPLINE_SURFACE ( 3, 2, ( 
 ( #43703, #52318, #44704 ),
 ( #75629, #75140, #50821 ),
 ( #11743, #74640, #12233 ),
 ( #42720, #43214, #82751 ),
 ( #67056, #66067, #4645 ),
 ( #73653, #4146, #58442 ),
 ( #59941, #97965, #35098 ),
 ( #96987, #66571, #89376 ) ),
 .UNSPECIFIED., .F., .F., .T. ) 
 B_SPLINE_SURFACE_WITH_KNOTS ( ( 4, 2, 2, 4 ),
 ( 3, 3 ),
 ( -2.579859069429257801E-16, 0.0001012599413938862529, 0.0002025198827880304918, 0.0004050397655763189695 ),
 ( 0.000000000000000000, 1.000000000000000000 ),
 .UNSPECIFIED. ) 
 GEOMETRIC_REPRESENTATION_ITEM ( )  RATIONAL_B_SPLINE_SURFACE ( (
 ( 1.000000000000000000, 0.8117984224358114620, 1.000000000000000000),
 ( 1.000000000000000000, 0.8431000163380804047, 1.000000000000000000),
 ( 1.000000000000000000, 0.8706302742274283357, 1.000000000000000000),
 ( 1.000000000000000000, 0.9180857590576141369, 1.000000000000000000),
 ( 1.000000000000000000, 0.9379650217683797031, 1.000000000000000000),
 ( 1.000000000000000000, 0.9847826944377771063, 1.000000000000000000),
 ( 1.000000000000000000, 1.000057331644988556, 1.000000000000000000),
 ( 1.000000000000000000, 1.000000000000000000, 1.000000000000000000) ) ) 
 REPRESENTATION_ITEM ( '' )  SURFACE ( )  );
#23274 = CARTESIAN_POINT ( 'NONE',  ( -73.62287095715004170, -23.72747288104441665, -1.053458166803662888 ) ) ;
#23275 = ORIENTED_EDGE ( 'NONE', *, *, #10265, .T. ) ;
#23276 = PLANE ( 'NONE',  #59119 ) ;
#23277 = DIRECTION ( 'NONE',  ( -4.522247983293619802E-39, -2.173523156893721996E-06, 0.9999999999976377785 ) ) ;
#23278 = DIRECTION ( 'NONE',  ( -3.773278334453079618E-23, 0.9999999999976377785, 2.173523156925979975E-06 ) ) ;
#23279 = CARTESIAN_POINT ( 'NONE',  ( 21.02075834227166951, -5.193550065563941942, 11.49999999999998934 ) ) ;
#23280 = DIRECTION ( 'NONE',  ( -0.7863974287229266169, -5.639749025771352497E-15, 0.6177208787939496570 ) ) ;
#23281 = CARTESIAN_POINT ( 'NONE',  ( 16.20606029192996900, -10.75321813762353251, -1.500000000000002220 ) ) ;
#23282 = DIRECTION ( 'NONE',  ( 0.000000000000000000, -1.000000000000000000, 0.000000000000000000 ) ) ;
#23283 = CARTESIAN_POINT ( 'NONE',  ( -55.53127495292982729, -24.83644354573578283, 8.397322867130096569 ) ) ;
#23284 = CARTESIAN_POINT ( 'NONE',  ( 18.55763160240848109, 7.024834138330111166, 11.49999999999998934 ) ) ;
#23285 = ORIENTED_EDGE ( 'NONE', *, *, #18163, .T. ) ;
#23286 = AXIS2_PLACEMENT_3D ( 'NONE', #32829, #64304, #1883 ) ;
#23287 = CARTESIAN_POINT ( 'NONE',  ( -9.641467040090685003, 17.89903724589931855, 11.49999999999999645 ) ) ;
#23288 = CARTESIAN_POINT ( 'NONE',  ( -80.54797791650044303, -24.40034930558991277, 0.3402023900116063482 ) ) ;
#23289 = CARTESIAN_POINT ( 'NONE',  ( -41.52287095715006870, -23.47593901973090169, -1.443836447538997092 ) ) ;
#23290 = EDGE_LOOP ( 'NONE', ( #97481, #21957, #81540, #36937 ) ) ;
#23291 = CARTESIAN_POINT ( 'NONE',  ( -41.05394856697249395, -25.21735233672366405, 3.457401395030163638 ) ) ;
#23292 = DIRECTION ( 'NONE',  ( 0.000000000000000000, 0.9513357669802769978, -0.3081562241202474572 ) ) ;
#23293 = CARTESIAN_POINT ( 'NONE',  ( -49.43920486724100982, -25.25214466810134795, 5.121422890020069119 ) ) ;
#23294 = EDGE_CURVE ( 'NONE', #96621, #27652, #70765, .T. ) ;
#23295 = CARTESIAN_POINT ( 'NONE',  ( -40.61243824264953872, -23.85049219812685095, 10.88485053497527488 ) ) ;
#23296 = CARTESIAN_POINT ( 'NONE',  ( -0.4362980769230789257, -6.376774720514411854, 19.46153846153846345 ) ) ;
#23297 = CARTESIAN_POINT ( 'NONE',  ( 16.71511084712224360, -11.16500066668146829, 11.49999999999998934 ) ) ;
#23298 = B_SPLINE_CURVE_WITH_KNOTS ( 'NONE', 3,
 ( #17660, #93273, #31889, #47625, #32893, #23763 ),
 .UNSPECIFIED., .F., .F.,
 ( 4, 2, 4 ),
 ( 0.000000000000000000, 0.001380901958385383991, 0.002761803916770767982 ),
 .UNSPECIFIED. ) ;
#23299 = FACE_OUTER_BOUND ( 'NONE', #23223, .T. ) ;
#23301 = VERTEX_POINT ( 'NONE', #9353 ) ;
#23300 = EDGE_CURVE ( 'NONE', #58202, #47484, #96502, .T. ) ;
#23302 = CARTESIAN_POINT ( 'NONE',  ( 27.53860345374808105, -5.356774720496559894, 0.000000000000000000 ) ) ;
#23303 = EDGE_CURVE ( 'NONE', #42203, #38912, #72252, .T. ) ;
#23304 = CARTESIAN_POINT ( 'NONE',  ( -17.51315278866654879, 14.73147661606379621, 11.49999999999999645 ) ) ;
#23305 = CARTESIAN_POINT ( 'NONE',  ( -13.58842472641693711, -18.21064416987719525, 11.49999999999998934 ) ) ;
#23306 = VERTEX_POINT ( 'NONE', #94593 ) ;
#23307 = CARTESIAN_POINT ( 'NONE',  ( -45.52287095715006870, -24.52232992886360918, 0.6492154411905974865 ) ) ;
#23308 = EDGE_CURVE ( 'NONE', #62785, #61654, #57999, .T. ) ;
#23309 = CARTESIAN_POINT ( 'NONE',  ( -126.5228709571499763, -23.73934037231757443, 11.05740245334327909 ) ) ;
#23310 = CARTESIAN_POINT ( 'NONE',  ( -38.56093905060389915, -23.73791477778911485, 11.05961554403170766 ) ) ;
#23311 = EDGE_CURVE ( 'NONE', #78575, #29423, #36237, .T. ) ;
#23312 = CARTESIAN_POINT ( 'NONE',  ( -30.57287095715006231, -23.48210175247266562, -1.443836490256470428 ) ) ;
#23313 = CARTESIAN_POINT ( 'NONE',  ( -128.6234765682969510, -24.66019654487200441, 8.947790411086108620 ) ) ;
#23314 = DIRECTION ( 'NONE',  ( 0.9980236263794188822, 0.000000000000000000, -0.06283980576413539243 ) ) ;
#23315 = EDGE_LOOP ( 'NONE', ( #62346, #74772, #41162, #99251 ) ) ;
#23316 = CARTESIAN_POINT ( 'NONE',  ( 8.549789220347504326, 18.50885834720105905, -1.500000000000002220 ) ) ;
#23317 = EDGE_LOOP ( 'NONE', ( #22558, #88667, #20463, #21602 ) ) ;
#23318 = EDGE_CURVE ( 'NONE', #89515, #55826, #66453, .T. ) ;
#23319 = CARTESIAN_POINT ( 'NONE',  ( 20.04565040668967413, 11.27863464804978477, 11.49999999999998934 ) ) ;
#23320 = CARTESIAN_POINT ( 'NONE',  ( -54.64430529514193324, -23.96169478059712787, 10.65365249895718947 ) ) ;
#23321 = ORIENTED_EDGE ( 'NONE', *, *, #86480, .T. ) ;
#23322 = CARTESIAN_POINT ( 'NONE',  ( -34.62287095715005592, -29.50248528299804818, 1.056150453629029817 ) ) ;
#23323 = CARTESIAN_POINT ( 'NONE',  ( -81.39414160900706463, -25.21421764495619300, 6.570651892964196605 ) ) ;
#23324 = DIRECTION ( 'NONE',  ( 6.030048488936326810E-14, 0.000000000000000000, -1.000000000000000000 ) ) ;
#23326 = VERTEX_POINT ( 'NONE', #65179 ) ;
#23325 = CARTESIAN_POINT ( 'NONE',  ( 9.569808575145499319, 19.01914523534739132, 11.49999999999999645 ) ) ;
#23327 = VERTEX_POINT ( 'NONE', #49441 ) ;
#23328 = CARTESIAN_POINT ( 'NONE',  ( 2.577866586777615154, 22.04066829813923789, -1.500000000000002220 ) ) ;
#23329 = CARTESIAN_POINT ( 'NONE',  ( -13.08992234710881064, 15.94516925376868244, 11.49999999999998934 ) ) ;
#23330 = B_SPLINE_CURVE_WITH_KNOTS ( 'NONE', 3,
 ( #78162, #32006, #71584, #62979 ),
 .UNSPECIFIED., .F., .F.,
 ( 4, 4 ),
 ( 0.000000000000000000, 9.999999999998897304E-05 ),
 .UNSPECIFIED. ) ;
#23331 = ORIENTED_EDGE ( 'NONE', *, *, #26580, .F. ) ;
#23332 = ORIENTED_EDGE ( 'NONE', *, *, #84921, .F. ) ;
#23333 = CARTESIAN_POINT ( 'NONE',  ( -65.05438548721849656, 5.356774720514425603, 24.50402280011859091 ) ) ;
#23334 = CARTESIAN_POINT ( 'NONE',  ( -95.62359480617779184, -25.00182538069147142, 7.747789668545044250 ) ) ;
#23335 = ORIENTED_EDGE ( 'NONE', *, *, #78969, .T. ) ;
#23336 = CARTESIAN_POINT ( 'NONE',  ( -51.62287095715006302, -23.96177878511307924, 10.65340807706330217 ) ) ;
#23337 = VERTEX_POINT ( 'NONE', #72774 ) ;
#23338 = CARTESIAN_POINT ( 'NONE',  ( -56.62287095715005592, -24.64965695001468404, 8.947790433994185832 ) ) ;
#23339 = DIRECTION ( 'NONE',  ( 1.000000000000000000, 3.773278334444166432E-23, 8.201307841325785021E-29 ) ) ;
#23340 = CARTESIAN_POINT ( 'NONE',  ( -20.21371806590929410, -4.994250807877889109, -1.500000000000002220 ) ) ;
#23341 = CARTESIAN_POINT ( 'NONE',  ( 17.22188757068894915, 13.35947340969901198, 11.49999999999999645 ) ) ;
#23342 = VECTOR ( 'NONE', #51168, 1000.000000000000227 ) ;
#23343 = CARTESIAN_POINT ( 'NONE',  ( 26.73860345374794534, -5.058662225110310828, -7.113848178280766099 ) ) ;
#23344 = CARTESIAN_POINT ( 'NONE',  ( -78.54012698005728055, -24.66019654487200441, 8.947790411086119278 ) ) ;
#23345 = CARTESIAN_POINT ( 'NONE',  ( -22.33494257564923302, 2.542849975942539587, -1.500000000000002220 ) ) ;
#23346 = CARTESIAN_POINT ( 'NONE',  ( -50.47686723370601669, -25.31296764644767094, 4.734242616601387788 ) ) ;
#23348 = ORIENTED_EDGE ( 'NONE', *, *, #78908, .T. ) ;
#23347 = EDGE_CURVE ( 'NONE', #57513, #33445, #48934, .T. ) ;
#23349 = PLANE ( 'NONE',  #45281 ) ;
#23350 = CARTESIAN_POINT ( 'NONE',  ( 4.527536911777373163, -5.876774720514422512, 21.53954785142818196 ) ) ;
#23351 = AXIS2_PLACEMENT_3D ( 'NONE', #79367, #77855, #85987 ) ;
#23352 = VERTEX_POINT ( 'NONE', #43320 ) ;
#23353 = VERTEX_POINT ( 'NONE', #79864 ) ;
#23354 = EDGE_CURVE ( 'NONE', #62407, #9013, #26534, .T. ) ;
#23355 = VERTEX_POINT ( 'NONE', #34703 ) ;
#23356 = CARTESIAN_POINT ( 'NONE',  ( 19.59546714036918758, 8.467717511154198462, -1.500000000000002220 ) ) ;
#23357 = EDGE_LOOP ( 'NONE', ( #62315, #78102, #614, #61698 ) ) ;
#23358 = CARTESIAN_POINT ( 'NONE',  ( 18.99863377428308198, 9.053671573812124507, -1.500000000000002220 ) ) ;
#23359 = CARTESIAN_POINT ( 'NONE',  ( -30.44999254588300985, -24.04395793212950849, -0.4713115009884517037 ) ) ;
#23360 = CARTESIAN_POINT ( 'NONE',  ( -110.9769629572514447, -25.22239614775561023, 3.498991103823542836 ) ) ;
#23361 = CARTESIAN_POINT ( 'NONE',  ( 2.976770017179964700, -5.876774720514419847, 20.68690469677381927 ) ) ;
#23362 = CARTESIAN_POINT ( 'NONE',  ( 19.92286461850947887, -9.344431347164146473, -1.500000000000002220 ) ) ;
#23363 = DIRECTION ( 'NONE',  ( -1.000000000000000000, -0.000000000000000000, -0.000000000000000000 ) ) ;
#23364 = VERTEX_POINT ( 'NONE', #42825 ) ;
#23365 = FACE_OUTER_BOUND ( 'NONE', #69719, .T. ) ;
#23366 = CARTESIAN_POINT ( 'NONE',  ( -121.5228709571500474, -23.72747288104470442, -1.053458166803224794 ) ) ;
#23367 = CARTESIAN_POINT ( 'NONE',  ( -20.21371806590929410, -4.994250807877889109, 11.49999999999999645 ) ) ;
#23368 = CARTESIAN_POINT ( 'NONE',  ( -74.58953762381673869, -24.65952944569304606, 1.056160979905703234 ) ) ;
#23369 = CARTESIAN_POINT ( 'NONE',  ( -108.6228709571500417, -23.48786465467242479, 11.44779295918253759 ) ) ;
#23370 = B_SPLINE_CURVE_WITH_KNOTS ( 'NONE', 3,
 ( #85291, #69070, #45244, #99503 ),
 .UNSPECIFIED., .F., .F.,
 ( 4, 4 ),
 ( 0.000000000000000000, 0.0001000000000000167422 ),
 .UNSPECIFIED. ) ;
#23371 = CARTESIAN_POINT ( 'NONE',  ( -10.22955294603096732, -23.25643961109228641, 8.370978854367626454 ) ) ;
#23372 = CARTESIAN_POINT ( 'NONE',  ( 14.87313431965483801, 15.23822737908125902, -1.500000000000002220 ) ) ;
#23373 = CARTESIAN_POINT ( 'NONE',  ( -98.63501790545433323, -23.73791477778911840, 11.05961554403170410 ) ) ;
#23374 = CARTESIAN_POINT ( 'NONE',  ( -107.6317652604150936, -23.73791477778912196, 11.05961554403169700 ) ) ;
#23375 = DIRECTION ( 'NONE',  ( -1.000000000000000000, -1.655121434032222977E-15, 0.000000000000000000 ) ) ;
#23376 = CARTESIAN_POINT ( 'NONE',  ( -71.31920756328558753, -25.12112739299269037, 7.112216829152949948 ) ) ;
#23377 = CC_DESIGN_DATE_AND_TIME_ASSIGNMENT ( #73349, #10435, ( #60221 ) ) ;
#23378 = CARTESIAN_POINT ( 'NONE',  ( -22.13300264024875119, -4.194623038110560032, -1.500000000000002220 ) ) ;
#23379 = CARTESIAN_POINT ( 'NONE',  ( -65.52287095715006160, -25.00158670708909625, 2.256160236439166411 ) ) ;
#23380 = ORIENTED_EDGE ( 'NONE', *, *, #39012, .T. ) ;
#23381 = CARTESIAN_POINT ( 'NONE',  ( -123.5228709571500616, -24.64898659630368627, 1.056161002820833028 ) ) ;
#23382 = CARTESIAN_POINT ( 'NONE',  ( 16.12930680145378304, -11.13525102954884893, 11.49999999999999645 ) ) ;
#23383 = CARTESIAN_POINT ( 'NONE',  ( 8.971512145086503409, -1.028487854913504362, -3.750000000000000000 ) ) ;
#23384 = CARTESIAN_POINT ( 'NONE',  ( -32.52287095715004739, -23.96177878511307213, 10.65340807706330750 ) ) ;
#23385 = ORIENTED_EDGE ( 'NONE', *, *, #37188, .F. ) ;
#23386 = LINE ( 'NONE', #77677, #89535 ) ;
#23387 = PLANE ( 'NONE',  #10816 ) ;
#23388 = CARTESIAN_POINT ( 'NONE',  ( -90.93395226104127005, -25.22174524493127379, 6.695141717414600180 ) ) ;
#23389 = CARTESIAN_POINT ( 'NONE',  ( 19.26447527235507451, 4.322997736827044690, -1.500000000000002220 ) ) ;
#23390 = EDGE_LOOP ( 'NONE', ( #21428, #66236, #51099, #9334 ) ) ;
#23391 = CARTESIAN_POINT ( 'NONE',  ( 8.616046215355789073, 6.376774720514426065, -25.03514012577542758 ) ) ;
#23392 = VECTOR ( 'NONE', #45655, 1000.000000000000000 ) ;
#23393 = B_SPLINE_CURVE_WITH_KNOTS ( 'NONE', 3,
 ( #52208, #98363, #35976, #11634 ),
 .UNSPECIFIED., .F., .F.,
 ( 4, 4 ),
 ( 1.387778780781445521E-17, 0.0001000000000000028644 ),
 .UNSPECIFIED. ) ;
#23394 = CALENDAR_DATE ( 2026, 9, 10 ) ;
#23395 = ORIENTED_EDGE ( 'NONE', *, *, #79345, .F. ) ;
#23396 = PLANE ( 'NONE',  #51596 ) ;
#23397 = CARTESIAN_POINT ( 'NONE',  ( 21.57151214508649772, 3.625915217019311583E-15, -2.299999999999999822 ) ) ;
#23398 = CARTESIAN_POINT ( 'NONE',  ( -55.48264273398157798, -24.83618233451448987, 1.606449574219538379 ) ) ;
#23399 = CARTESIAN_POINT ( 'NONE',  ( 32.40823333110732563, -4.442403080972329832, -4.096588619916003537 ) ) ;
#23400 = CARTESIAN_POINT ( 'NONE',  ( -2.243088942307695177, -5.876774720514409189, 19.14743589743590491 ) ) ;
#23401 = CARTESIAN_POINT ( 'NONE',  ( -44.62287095715004881, -24.64965695001468404, 8.947790433994187609 ) ) ;
#23402 = CARTESIAN_POINT ( 'NONE',  ( -107.5502841407374035, -24.51314013834316086, 0.6176544820404228364 ) ) ;
#23404 = ADVANCED_FACE ( 'NONE', ( #73269 ), #70928, .T. ) ;
#23403 = CARTESIAN_POINT ( 'NONE',  ( -19.89792590360708147, -2.209704250470923892, 11.49999999999998934 ) ) ;
#23405 = VECTOR ( 'NONE', #74883, 1000.000000000000000 ) ;
#23406 = CARTESIAN_POINT ( 'NONE',  ( -6.660000000000001030, 8.793627758918228565, -2.994553991265763049 ) ) ;
#23407 = CARTESIAN_POINT ( 'NONE',  ( -45.52502077163275374, -24.92592662359561118, 8.075495903018000021 ) ) ;
#23408 = ORIENTED_EDGE ( 'NONE', *, *, #55125, .T. ) ;
#23409 = DIRECTION ( 'NONE',  ( -3.773278334453079030E-23, 0.9999999999976377785, 2.173523156925979128E-06 ) ) ;
#23410 = DIRECTION ( 'NONE',  ( -3.773278334453079618E-23, 0.9999999999976377785, 2.173523156925979975E-06 ) ) ;
#23411 = EDGE_CURVE ( 'NONE', #33324, #12246, #83355, .T. ) ;
#23412 = CARTESIAN_POINT ( 'NONE',  ( 29.73860345376319358, 5.356653621633795659, 18.57591161935199153 ) ) ;
#23413 = CARTESIAN_POINT ( 'NONE',  ( 32.53135143123563466, 0.3587747205144265483, 6.926385399448451885 ) ) ;
#23414 = EDGE_CURVE ( 'NONE', #21242, #58098, #89982, .T. ) ;
#23415 = CARTESIAN_POINT ( 'NONE',  ( -116.4728709571500360, -25.40558663563427189, 5.000950442582703381 ) ) ;
#23416 = B_SPLINE_CURVE_WITH_KNOTS ( 'NONE', 3,
 ( #10021, #87655, #2930, #70428 ),
 .UNSPECIFIED., .F., .F.,
 ( 4, 4 ),
 ( 3.244156161651605912E-05, 0.008792202774406619389 ),
 .UNSPECIFIED. ) ;
#23417 = CARTESIAN_POINT ( 'NONE',  ( -83.58828318951894687, -24.34968618360933235, 0.1864209137778810865 ) ) ;
#23418 = CARTESIAN_POINT ( 'NONE',  ( 11.62916340711181284, -0.3587747205144265483, 28.75961759920349792 ) ) ;
#23419 = PLANE ( 'NONE',  #58267 ) ;
#23420 = ORIENTED_EDGE ( 'NONE', *, *, #3715, .F. ) ;
#23421 = CARTESIAN_POINT ( 'NONE',  ( 16.58868386459195676, 11.68684615565071283, 11.49999999999998934 ) ) ;
#23422 = EDGE_CURVE ( 'NONE', #6116, #9400, #62857, .T. ) ;
#23423 = DIRECTION ( 'NONE',  ( -2.145277261456712182E-39, -2.173523156925979128E-06, 0.9999999999976378895 ) ) ;
#23424 = DIRECTION ( 'NONE',  ( -3.773278334444167608E-23, 1.000000000000000000, 0.000000000000000000 ) ) ;
#23425 = ORIENTED_EDGE ( 'NONE', *, *, #81428, .F. ) ;
#23426 = CARTESIAN_POINT ( 'NONE',  ( -86.52287095715009002, -24.51387760970724727, 9.387446482453409402 ) ) ;
#23427 = CARTESIAN_POINT ( 'NONE',  ( -7.807601069497579260, -18.53474111305376937, -1.500000000000002220 ) ) ;
#23428 = CARTESIAN_POINT ( 'NONE',  ( 14.35337761433406811, 15.45585641580067104, 11.49999999999999645 ) ) ;
#23429 = VECTOR ( 'NONE', #87699, 1000.000000000000000 ) ;
#23430 = CARTESIAN_POINT ( 'NONE',  ( 1.014068502963303864, -22.09113584270698993, 11.49999999999998934 ) ) ;
#23431 = CARTESIAN_POINT ( 'NONE',  ( -9.284664653622879626, 18.31210316397345395, 11.49999999999998934 ) ) ;
#23432 = CARTESIAN_POINT ( 'NONE',  ( -65.62287095715005592, -25.00182538069145721, 7.747789668545100206 ) ) ;
#23433 = CARTESIAN_POINT ( 'NONE',  ( -60.65501980248554048, -23.85016227208579664, -0.8807180028928355275 ) ) ;
#23434 = ORIENTED_EDGE ( 'NONE', *, *, #33159, .F. ) ;
#23435 = LINE ( 'NONE', #93461, #49316 ) ;
#23436 = EDGE_LOOP ( 'NONE', ( #84410, #90331, #75992, #56922 ) ) ;
#23437 = DIRECTION ( 'NONE',  ( 0.000000000000000000, 0.9999999999976377785, 2.173523156925979975E-06 ) ) ;
#23439 = B_SPLINE_CURVE_WITH_KNOTS ( 'NONE', 3,
 ( #39098, #55348, #16762, #48233, #79164, #40113 ),
 .UNSPECIFIED., .F., .F.,
 ( 4, 2, 4 ),
 ( 1.570755371633816901E-05, 0.001396183895866085368, 0.002776660238015832543 ),
 .UNSPECIFIED. ) ;
#23438 = B_SPLINE_SURFACE_WITH_KNOTS ( 'NONE', 3, 3, ( 
 ( #93865, #2039, #2535, #70535 ),
 ( #17242, #31469, #62431, #16739 ),
 ( #77629, #32981, #54822, #25356 ),
 ( #70032, #56334, #85758, #63956 ),
 ( #63446, #1532, #15741, #33467 ),
 ( #86259, #93357, #87254, #46706 ),
 ( #518, #71545, #40088, #41097 ) ),
 .UNSPECIFIED., .F., .F., .F.,
 ( 4, 3, 4 ),
 ( 4, 4 ),
 ( 0.7945040050992243641, 0.8970133687736503436, 0.9995227324480763231 ),
 ( 0.7196768771113082330, 0.7210218522699133326 ),
 .UNSPECIFIED. ) ;
#23440 = CARTESIAN_POINT ( 'NONE',  ( -85.62287095714999907, -24.15516710230295772, 10.28746687063726739 ) ) ;
#23441 = ORIENTED_EDGE ( 'NONE', *, *, #84921, .T. ) ;
#23442 = ORIENTED_EDGE ( 'NONE', *, *, #17341, .F. ) ;
#23443 = VERTEX_POINT ( 'NONE', #99561 ) ;
#23444 = CARTESIAN_POINT ( 'NONE',  ( -27.61845239340658154, -5.965225279485594001, -10.37513603161905351 ) ) ;
#23445 = CARTESIAN_POINT ( 'NONE',  ( -31.58953762381672092, -23.47593901973091235, -1.443836447539013301 ) ) ;
#23446 = PLANE ( 'NONE',  #40658 ) ;
#23447 = CARTESIAN_POINT ( 'NONE',  ( -1.706377481887368486, -20.59057665607738130, -1.500000000000002220 ) ) ;
#23448 = ADVANCED_FACE ( 'NONE', ( #5241 ), #29073, .T. ) ;
#23449 = CARTESIAN_POINT ( 'NONE',  ( -19.46174652491427182, -9.421329337880418819, 11.49999999999999645 ) ) ;
#23450 = ORIENTED_EDGE ( 'NONE', *, *, #79079, .F. ) ;
#23451 = DIRECTION ( 'NONE',  ( 0.000000000000000000, 0.000000000000000000, 1.000000000000000000 ) ) ;
#23452 = DIRECTION ( 'NONE',  ( -0.9952638024365005887, 0.000000000000000000, -0.09721092304694053943 ) ) ;
#23453 = CARTESIAN_POINT ( 'NONE',  ( -8.633843874998758494, 20.65557450359631630, 11.49999999999998934 ) ) ;
#23454 = CARTESIAN_POINT ( 'NONE',  ( -47.51395832360446292, -23.73791477778911485, 11.05961554403170766 ) ) ;
#23455 = CARTESIAN_POINT ( 'NONE',  ( 26.74698519091204574, 1.477225279485574028, -10.98683230472874151 ) ) ;
#23456 = ORIENTED_EDGE ( 'NONE', *, *, #45420, .T. ) ;
#23457 = B_SPLINE_CURVE_WITH_KNOTS ( 'NONE', 3,
 ( #97872, #37487, #13136, #67447, #52221, #28370 ),
 .UNSPECIFIED., .F., .F.,
 ( 4, 2, 4 ),
 ( 1.570887131794333942E-05, 0.001396322306279760422, 0.002776935741241577573 ),
 .UNSPECIFIED. ) ;
#23458 = CARTESIAN_POINT ( 'NONE',  ( -116.4728709572980847, -25.40561136713226276, 5.197834629370922777 ) ) ;
#23459 = LINE ( 'NONE', #98604, #24808 ) ;
#23460 = CARTESIAN_POINT ( 'NONE',  ( 8.971512145086530055, -9.528487854913503696, -4.499999999999994671 ) ) ;
#23461 = CARTESIAN_POINT ( 'NONE',  ( -19.94816486946033507, 6.322790147265108018, -1.500000000000002220 ) ) ;
#23462 = EDGE_LOOP ( 'NONE', ( #13677, #8859, #6994, #57675 ) ) ;
#23463 = VECTOR ( 'NONE', #15208, 1000.000000000000000 ) ;
#23464 = CARTESIAN_POINT ( 'NONE',  ( -67.56551492114158464, -23.48786465467241058, 11.44779295918254824 ) ) ;
#23465 = EDGE_LOOP ( 'NONE', ( #62808, #32197, #63542, #6058 ) ) ;
#23466 = EDGE_CURVE ( 'NONE', #83268, #3631, #70007, .T. ) ;
#23467 = FACE_OUTER_BOUND ( 'NONE', #38011, .T. ) ;
#23468 = CARTESIAN_POINT ( 'NONE',  ( -21.15187133135857422, -0.9709546189074961253, -1.500000000000002220 ) ) ;
#23469 = VERTEX_POINT ( 'NONE', #14334 ) ;
#23470 = CARTESIAN_POINT ( 'NONE',  ( -50.50118616174772512, -24.15503026093912808, -0.2815557561904566963 ) ) ;
#23471 = CARTESIAN_POINT ( 'NONE',  ( -14.02725853290852243, 16.66567569088042688, 11.49999999999998934 ) ) ;
#23472 = DIRECTION ( 'NONE',  ( 0.000000000000000000, -0.9999999999976377785, -2.173523156925979128E-06 ) ) ;
#23473 = CARTESIAN_POINT ( 'NONE',  ( -84.52287095715006160, -23.47593901973090524, -1.443836447538996648 ) ) ;
#23474 = CARTESIAN_POINT ( 'NONE',  ( -35.52287095715008292, -24.14406661686761524, 10.28769366194079282 ) ) ;
#23475 = CARTESIAN_POINT ( 'NONE',  ( -8.041798833237560729, -20.28069125152608976, -1.500000000000002220 ) ) ;
#23476 = CARTESIAN_POINT ( 'NONE',  ( -95.52287095715011844, -24.92579138211019796, 1.929029949965664459 ) ) ;
#23477 = EDGE_LOOP ( 'NONE', ( #89234, #93385, #41527, #10108 ) ) ;
#23478 = CARTESIAN_POINT ( 'NONE',  ( 7.460332110455646593, -5.876774720514418959, 20.55293369838740247 ) ) ;
#23479 = CARTESIAN_POINT ( 'NONE',  ( -15.87499999999997868, 1.530808498934188612E-16, -1.249999999999997558 ) ) ;
#23480 = ORIENTED_EDGE ( 'NONE', *, *, #95490, .T. ) ;
#23481 = VECTOR ( 'NONE', #72787, 1000.000000000000000 ) ;
#23482 = AXIS2_PLACEMENT_3D ( 'NONE', #1759, #63167, #63678 ) ;
#23483 = ORIENTED_EDGE ( 'NONE', *, *, #81654, .T. ) ;
#23484 = B_SPLINE_CURVE_WITH_KNOTS ( 'NONE', 3,
 ( #75919, #82051, #68325, #90164 ),
 .UNSPECIFIED., .F., .F.,
 ( 4, 4 ),
 ( 0.000000000000000000, 0.0001000000000000028644 ),
 .UNSPECIFIED. ) ;
#23485 = ORIENTED_EDGE ( 'NONE', *, *, #18656, .F. ) ;
#23486 = CARTESIAN_POINT ( 'NONE',  ( -17.97250661212648026, 5.965225279485594001, -23.43622901028613015 ) ) ;
#23487 = CARTESIAN_POINT ( 'NONE',  ( -39.62287095715005592, -23.47593901973091235, -1.443836447539011525 ) ) ;
#23488 = CARTESIAN_POINT ( 'NONE',  ( -19.34623641613454836, -8.721557147202650739, 11.49999999999998934 ) ) ;
#23489 = CARTESIAN_POINT ( 'NONE',  ( -121.6228709571500701, -24.33832256526968862, 0.1851278514119947260 ) ) ;
#23490 = CARTESIAN_POINT ( 'NONE',  ( -79.32136430576915131, -25.27791861366366533, 7.049788063976406782 ) ) ;
#23491 = CARTESIAN_POINT ( 'NONE',  ( -104.6228709571500559, -23.48783264082478794, -1.443836473390062158 ) ) ;
#23492 = CARTESIAN_POINT ( 'NONE',  ( -99.52287095715009002, -23.47593901973090524, -1.443836447538996648 ) ) ;
#23493 = ADVANCED_FACE ( 'NONE', ( #69132 ), #99071, .T. ) ;
#23494 = PERSON ( 'NAUO-PER3', 'UNSPECIFIED', 'UNSPECIFIED', ('UNSPECIFIED'), ('UNSPECIFIED'), ('UNSPECIFIED') ) ;
#23495 = CARTESIAN_POINT ( 'NONE',  ( 14.41255161864883583, -12.98630880007775268, -1.500000000000002220 ) ) ;
#23496 = CARTESIAN_POINT ( 'NONE',  ( -39.02522392549908403, -25.31392318313163159, 5.203682277190879724 ) ) ;
#23497 = ORIENTED_EDGE ( 'NONE', *, *, #17910, .F. ) ;
#23498 = CARTESIAN_POINT ( 'NONE',  ( 8.422564666779264186, -17.53554878399664574, 11.49999999999999645 ) ) ;
#23499 = DIRECTION ( 'NONE',  ( -0.1489078231574191280, 0.000000000000000000, 0.9888510809027406534 ) ) ;
#23500 = EDGE_CURVE ( 'NONE', #95766, #19712, #92997, .T. ) ;
#23501 = PLANE ( 'NONE',  #57642 ) ;
#23502 = ORIENTED_EDGE ( 'NONE', *, *, #48148, .T. ) ;
#23503 = CARTESIAN_POINT ( 'NONE',  ( 2.993128331772667572, -6.376774720514402972, 18.53171057923899312 ) ) ;
#23504 = EDGE_CURVE ( 'NONE', #93563, #59914, #31379, .T. ) ;
#23505 = CARTESIAN_POINT ( 'NONE',  ( -65.52287095715006160, -29.50250243563736774, 8.947779886222143375 ) ) ;
#23506 = ADVANCED_FACE ( 'NONE', ( #52925 ), #59541, .F. ) ;
#23507 = CARTESIAN_POINT ( 'NONE',  ( -7.160000000000000142, -9.123836073446797812, -2.666350264951732552 ) ) ;
#23508 = FACE_BOUND ( 'NONE', #40067, .T. ) ;
#23509 = CARTESIAN_POINT ( 'NONE',  ( 5.239555828037883778, -18.94419173073049478, -1.500000000000002220 ) ) ;
#23510 = CARTESIAN_POINT ( 'NONE',  ( -41.39099037118809576, -25.27806020386471531, 4.532732343367795735 ) ) ;
#23512 = EDGE_CURVE ( 'NONE', #7527, #25743, #98072, .T. ) ;
#23511 = EDGE_LOOP ( 'NONE', ( #69554, #14867, #1313, #14115, #12561 ) ) ;
#23513 = VECTOR ( 'NONE', #64029, 1000.000000000000000 ) ;
#23514 = CARTESIAN_POINT ( 'NONE',  ( 10.40854797073303395, 18.91789161722374146, 11.49999999999998934 ) ) ;
#23515 = CARTESIAN_POINT ( 'NONE',  ( -40.64049736129675949, -24.52300882791530157, 0.6510814631126359275 ) ) ;
#23516 = CARTESIAN_POINT ( 'NONE',  ( -121.5228709571500616, -24.64898659630529565, 1.056161002820833028 ) ) ;
#23517 = CARTESIAN_POINT ( 'NONE',  ( -17.35246277222573141, 15.15038115719275424, -1.500000000000002220 ) ) ;
#23518 = B_SPLINE_CURVE_WITH_KNOTS ( 'NONE', 3,
 ( #86994, #23079, #16473, #56065 ),
 .UNSPECIFIED., .F., .F.,
 ( 4, 4 ),
 ( 2.775557561562891043E-17, 9.999999999998898659E-05 ),
 .UNSPECIFIED. ) ;
#23519 = MECHANICAL_CONTEXT ( 'NONE', #42716, 'mechanical' ) ;
#23520 = CARTESIAN_POINT ( 'NONE',  ( -126.5228709571500616, -29.50250243563736774, 8.947779886222132717 ) ) ;
#23521 = CARTESIAN_POINT ( 'NONE',  ( -115.6228709571500559, -23.47593901973091235, -1.443836447538997536 ) ) ;
#23522 = CARTESIAN_POINT ( 'NONE',  ( -121.5186303220462776, -24.51419770103157347, 9.386484678747175181 ) ) ;
#23523 = DIRECTION ( 'NONE',  ( 0.000000000000000000, 0.000000000000000000, 1.000000000000000000 ) ) ;
#23524 = CARTESIAN_POINT ( 'NONE',  ( -111.7148472136480990, -25.29824037455150076, 3.873545699286501165 ) ) ;
#23525 = FACE_OUTER_BOUND ( 'NONE', #4159, .T. ) ;
#23526 = B_SPLINE_CURVE_WITH_KNOTS ( 'NONE', 3,
 ( #4684, #88922, #26010, #20380 ),
 .UNSPECIFIED., .F., .F.,
 ( 4, 4 ),
 ( 0.9794846856643069088, 0.9804854327050720464 ),
 .UNSPECIFIED. ) ;
#23527 = CARTESIAN_POINT ( 'NONE',  ( -114.6254316867186844, -24.35071581493544102, 9.817618358456016381 ) ) ;
#23529 = EDGE_CURVE ( 'NONE', #77894, #77030, #43061, .T. ) ;
#23528 = CARTESIAN_POINT ( 'NONE',  ( -9.044204435542846809, 17.70297415775587169, 11.49999999999998934 ) ) ;
#23530 = LINE ( 'NONE', #76323, #82435 ) ;
#23531 = CARTESIAN_POINT ( 'NONE',  ( 10.41257876278241845, -16.90412932818451353, -1.500000000000002220 ) ) ;
#23532 = DIRECTION ( 'NONE',  ( 2.313651251573820309E-16, -1.000000000000000000, 8.068660792749117443E-16 ) ) ;
#23533 = UNCERTAINTY_MEASURE_WITH_UNIT (LENGTH_MEASURE( 1.000000000000000082E-05 ), #61271, 'distance_accuracy_value', 'NONE');
#23534 = CARTESIAN_POINT ( 'NONE',  ( -39.04303308397305727, -25.29116819090583235, 4.215216924258844422 ) ) ;
#23535 = DIRECTION ( 'NONE',  ( 1.000000000000000000, 0.000000000000000000, 0.000000000000000000 ) ) ;
#23536 = CARTESIAN_POINT ( 'NONE',  ( 4.358738815032396907, -20.29635662749097236, 11.49999999999999645 ) ) ;
#23537 = CARTESIAN_POINT ( 'NONE',  ( -94.52287095715007581, -23.47593901973090524, -1.443836447538996648 ) ) ;
#23538 = AXIS2_PLACEMENT_3D ( 'NONE', #73018, #89230, #72517 ) ;
#23539 = EDGE_CURVE ( 'NONE', #80523, #88227, #94273, .T. ) ;
#23540 = CARTESIAN_POINT ( 'NONE',  ( -106.5551948350586429, -23.96119346886880663, -0.6495511937832030291 ) ) ;
#23541 = CARTESIAN_POINT ( 'NONE',  ( -20.37646751746074969, -10.17465561509698979, 11.49999999999999645 ) ) ;
#23542 = AXIS2_PLACEMENT_3D ( 'NONE', #91464, #21939, #36200 ) ;
#23543 = ORIENTED_EDGE ( 'NONE', *, *, #30441, .F. ) ;
#23544 = CARTESIAN_POINT ( 'NONE',  ( -69.55927295150912926, -23.73766607897669445, -1.055555164236460008 ) ) ;
#23545 = EDGE_CURVE ( 'NONE', #35163, #53312, #83532, .T. ) ;
#23546 = CARTESIAN_POINT ( 'NONE',  ( -92.52287095715010423, -24.33927499327853994, 9.819080762295806508 ) ) ;
#23547 = VERTEX_POINT ( 'NONE', #45312 ) ;
#23548 = CIRCLE ( 'NONE', #78672, 28.96799999999999287 ) ;
#23549 = CARTESIAN_POINT ( 'NONE',  ( -19.56588111578679090, -4.897929960003377658, 11.49999999999998934 ) ) ;
#23550 = PLANE ( 'NONE',  #48417 ) ;
#23551 = EDGE_CURVE ( 'NONE', #56734, #3816, #99110, .T. ) ;
#23552 = CIRCLE ( 'NONE', #59221, 28.96799999999999287 ) ;
#23553 = CARTESIAN_POINT ( 'NONE',  ( -52.52287095715005449, -23.95044443724991723, 10.65354141964649592 ) ) ;
#23554 = ORIENTED_EDGE ( 'NONE', *, *, #42120, .T. ) ;
#23555 = AXIS2_PLACEMENT_3D ( 'NONE', #20335, #59934, #14224 ) ;
#23556 = EDGE_CURVE ( 'NONE', #24603, #45647, #25341, .T. ) ;
#23557 = B_SPLINE_CURVE_WITH_KNOTS ( 'NONE', 3,
 ( #45270, #20912, #68110, #89939 ),
 .UNSPECIFIED., .F., .F.,
 ( 4, 4 ),
 ( 0.000000000000000000, 9.999999999998900014E-05 ),
 .UNSPECIFIED. ) ;
#23558 = VERTEX_POINT ( 'NONE', #80132 ) ;
#23559 = CARTESIAN_POINT ( 'NONE',  ( -101.6228709571500701, -23.47596703998600631, 11.44779298504227683 ) ) ;
#23560 = CARTESIAN_POINT ( 'NONE',  ( 1.119804705421552748, 22.86502198858056545, -1.500000000000002220 ) ) ;
#23562 = ADVANCED_FACE ( 'NONE', ( #72531 ), #62032, .T. ) ;
#23561 = CARTESIAN_POINT ( 'NONE',  ( -50.49777224651334961, -25.18439650350726922, 3.296419330453493224 ) ) ;
#23563 = CARTESIAN_POINT ( 'NONE',  ( 21.13687465659472409, 4.681744431724916389, -1.500000000000002220 ) ) ;
#23564 = CARTESIAN_POINT ( 'NONE',  ( -123.6234902428110303, -24.65952944569305316, 1.056160979905707897 ) ) ;
#23565 = CARTESIAN_POINT ( 'NONE',  ( 8.587038044527741221, -19.06309208085484386, 11.49999999999999645 ) ) ;
#23566 = ORIENTED_EDGE ( 'NONE', *, *, #22270, .T. ) ;
#23567 = CARTESIAN_POINT ( 'NONE',  ( -124.5895435931244322, -24.34968618360933945, 0.1864209137778899961 ) ) ;
#23568 = CARTESIAN_POINT ( 'NONE',  ( -12.30081598482267680, 18.28176383447183895, -1.500000000000002220 ) ) ;
#23569 = DIRECTION ( 'NONE',  ( -0.000000000000000000, -1.000000000000000000, 0.000000000000000000 ) ) ;
#23570 = CARTESIAN_POINT ( 'NONE',  ( -65.62287095715004170, -24.91570333823099759, 8.075032458375558164 ) ) ;
#23571 = ORIENTED_EDGE ( 'NONE', *, *, #3070, .T. ) ;
#23572 = DIRECTION ( 'NONE',  ( 0.000000000000000000, -0.9999999999976377785, -2.173523156925979975E-06 ) ) ;
#23573 = PLANE ( 'NONE',  #17059 ) ;
#23574 = EDGE_LOOP ( 'NONE', ( #64434, #85695 ) ) ;
#23575 = DIRECTION ( 'NONE',  ( 3.773278334444167608E-23, -1.000000000000000000, 0.000000000000000000 ) ) ;
#23576 = ORIENTED_EDGE ( 'NONE', *, *, #50288, .F. ) ;
#23577 = ORIENTED_EDGE ( 'NONE', *, *, #61355, .T. ) ;
#23578 = CARTESIAN_POINT ( 'NONE',  ( -71.60771150786226258, -23.48786465467241058, 11.44779295918254824 ) ) ;
#23579 = CARTESIAN_POINT ( 'NONE',  ( -101.3783285514244028, -25.27404712219727401, 3.208885956357566460 ) ) ;
#23580 = CARTESIAN_POINT ( 'NONE',  ( -100.5228709571500758, -24.62285846331434058, 9.038163153548365969 ) ) ;
#23581 = CARTESIAN_POINT ( 'NONE',  ( -3.437008290023895185, 20.19323497536227663, -1.500000000000002220 ) ) ;
#23582 = ORIENTED_EDGE ( 'NONE', *, *, #73377, .T. ) ;
#23583 = CARTESIAN_POINT ( 'NONE',  ( -79.52287095715006160, -24.64898659630367916, 1.056161002820826145 ) ) ;
#23584 = CARTESIAN_POINT ( 'NONE',  ( -44.63404635305053603, -24.34968618360933235, 0.1864209137778787551 ) ) ;
#23585 = LINE ( 'NONE', #69281, #72620 ) ;
#23586 = CARTESIAN_POINT ( 'NONE',  ( -14.60993195340527251, 16.82711592829100411, -1.500000000000002220 ) ) ;
#23587 = CARTESIAN_POINT ( 'NONE',  ( -71.29814285433251086, -25.24267958441406634, 6.333824918460533304 ) ) ;
#23588 = CYLINDRICAL_SURFACE ( 'NONE', #46384, 2.899999999999999911 ) ;
#23589 = EDGE_LOOP ( 'NONE', ( #7502, #4862, #10069, #79369 ) ) ;
#23590 = DIRECTION ( 'NONE',  ( -3.773278334453079618E-23, 0.9999999999976377785, 2.173523156925979975E-06 ) ) ;
#23591 = DIRECTION ( 'NONE',  ( -0.000000000000000000, 1.000000000000000000, -0.000000000000000000 ) ) ;
#23592 = VECTOR ( 'NONE', #23041, 1000.000000000000000 ) ;
#23593 = CARTESIAN_POINT ( 'NONE',  ( 5.313885144808909722, 20.14914662543312929, -1.500000000000002220 ) ) ;
#23594 = ORIENTED_EDGE ( 'NONE', *, *, #76958, .T. ) ;
#23596 = ORIENTED_EDGE ( 'NONE', *, *, #47945, .T. ) ;
#23595 = CARTESIAN_POINT ( 'NONE',  ( -95.52287095715010423, -25.00182538069145366, 7.747789668545101982 ) ) ;
#23597 = VERTEX_POINT ( 'NONE', #3023 ) ;
#23598 = CARTESIAN_POINT ( 'NONE',  ( 9.402885806365684829, 5.965225279485572685, 29.04108526060719342 ) ) ;
#23599 = CARTESIAN_POINT ( 'NONE',  ( -8.441512789788195192, 19.21024974253229800, -1.500000000000002220 ) ) ;
#23600 = ORIENTED_EDGE ( 'NONE', *, *, #14221, .F. ) ;
#23601 = CARTESIAN_POINT ( 'NONE',  ( 8.133973695506851342, 10.05415566027042829, -0.8796246415986995748 ) ) ;
#23602 = CARTESIAN_POINT ( 'NONE',  ( -50.44065031394416820, -25.27412228105976055, 2.834208053142886818 ) ) ;
#23603 = B_SPLINE_CURVE_WITH_KNOTS ( 'NONE', 3,
 ( #12039, #43007, #43990, #5923 ),
 .UNSPECIFIED., .F., .F.,
 ( 4, 4 ),
 ( 0.000000000000000000, 1.000000000000000000 ),
 .UNSPECIFIED. ) ;
#23604 = CARTESIAN_POINT ( 'NONE',  ( 8.476323908354110870, -5.356774720513951316, -27.09030197689322961 ) ) ;
#23605 = LINE ( 'NONE', #282, #3229 ) ;
#23606 = CARTESIAN_POINT ( 'NONE',  ( -92.54439753425451443, -24.66019654487200441, 8.947790411086117501 ) ) ;
#23607 = CARTESIAN_POINT ( 'NONE',  ( -65.62287095715005592, -23.85229601348996198, 10.88205029486208986 ) ) ;
#23609 = VERTEX_POINT ( 'NONE', #23432 ) ;
#23608 = CARTESIAN_POINT ( 'NONE',  ( -4.330935931041660858, -21.79039167146679290, 11.49999999999999645 ) ) ;
#23610 = CARTESIAN_POINT ( 'NONE',  ( 0.000000000000000000, -2.056774720514426669, 0.000000000000000000 ) ) ;
#23611 = CARTESIAN_POINT ( 'NONE',  ( -61.62287095715004881, -29.50248528299804818, 1.056150453629034924 ) ) ;
#23612 = EDGE_LOOP ( 'NONE', ( #39454, #99369, #22821, #67410 ) ) ;
#23613 = CARTESIAN_POINT ( 'NONE',  ( 9.629844747126790949, -20.51516216672183290, 11.49999999999998934 ) ) ;
#23615 = EDGE_LOOP ( 'NONE', ( #8271, #10917, #80162, #65330, #17290, #80662 ) ) ;
#23614 = CARTESIAN_POINT ( 'NONE',  ( -28.94417065657630062, -25.04901277059179776, 6.781005994535155068 ) ) ;
#23616 = ORIENTED_EDGE ( 'NONE', *, *, #92847, .F. ) ;
#23617 = CARTESIAN_POINT ( 'NONE',  ( -67.92287095715008149, -23.47596703998600276, 11.44779298504227683 ) ) ;
#23618 = VECTOR ( 'NONE', #54172, 1000.000000000000114 ) ;
#23619 = EDGE_CURVE ( 'NONE', #24603, #49218, #41586, .T. ) ;
#23620 = CARTESIAN_POINT ( 'NONE',  ( 19.31759285448427477, -5.727529672960866236, 11.49999999999998934 ) ) ;
#23621 = CARTESIAN_POINT ( 'NONE',  ( -81.62287095715004170, -23.48786465467241058, 11.44779295918254647 ) ) ;
#23622 = VERTEX_POINT ( 'NONE', #41081 ) ;
#23623 = VECTOR ( 'NONE', #93254, 1000.000000000000114 ) ;
#23624 = CARTESIAN_POINT ( 'NONE',  ( 8.160000000000000142, -2.890508098367099432, -0.2344417481469836528 ) ) ;
#23625 = CARTESIAN_POINT ( 'NONE',  ( -15.27869365379592281, -16.34152646814254339, -1.500000000000002220 ) ) ;
#23626 = VECTOR ( 'NONE', #90797, 1000.000000000000114 ) ;
#23627 = VECTOR ( 'NONE', #96336, 1000.000000000000000 ) ;
#23628 = VERTEX_POINT ( 'NONE', #87750 ) ;
#23629 = ORIENTED_EDGE ( 'NONE', *, *, #85983, .T. ) ;
#23630 = DIRECTION ( 'NONE',  ( 1.286817348990133408E-16, 0.000000000000000000, -1.000000000000000000 ) ) ;
#23631 = CARTESIAN_POINT ( 'NONE',  ( -94.54704744228577340, -24.51419770103156281, 9.386484678747184063 ) ) ;
#23632 = CARTESIAN_POINT ( 'NONE',  ( -85.55620429048339304, -23.47596703998600631, 11.44779298504227683 ) ) ;
#23633 = EDGE_CURVE ( 'NONE', #73650, #71376, #59242, .T. ) ;
#23634 = ADVANCED_FACE ( 'NONE', ( #88251, #57322 ), #61540, .F. ) ;
#23635 = DIRECTION ( 'NONE',  ( 0.000000000000000000, -0.000000000000000000, -1.000000000000000000 ) ) ;
#23636 = VECTOR ( 'NONE', #41426, 1000.000000000000114 ) ;
#23637 = EDGE_CURVE ( 'NONE', #7900, #78003, #71274, .T. ) ;
#23638 = CARTESIAN_POINT ( 'NONE',  ( 5.085443162053245203, 3.316774720514426456, -27.56355752155217331 ) ) ;
#23639 = CARTESIAN_POINT ( 'NONE',  ( 19.54226456527178257, 0.3027743077981833730, -1.500000000000002220 ) ) ;
#23640 = CARTESIAN_POINT ( 'NONE',  ( -39.22287095715006444, -23.47596703998600276, 11.44779298504227683 ) ) ;
#23641 = EDGE_CURVE ( 'NONE', #67908, #71832, #92458, .T. ) ;
#23642 = CARTESIAN_POINT ( 'NONE',  ( 11.78165356204951131, -17.99452314462042324, -1.500000000000002220 ) ) ;
#23643 = B_SPLINE_CURVE_WITH_KNOTS ( 'NONE', 3,
 ( #54408, #1632, #9733, #63543, #87351, #55417 ),
 .UNSPECIFIED., .F., .F.,
 ( 4, 2, 4 ),
 ( 1.570755371634013412E-05, 0.001396183895866088187, 0.002776660238015836012 ),
 .UNSPECIFIED. ) ;
#23644 = LINE ( 'NONE', #71341, #62540 ) ;
#23645 = CARTESIAN_POINT ( 'NONE',  ( -114.5228709571500616, -24.64898659630529565, 1.056161002820831474 ) ) ;
#23646 = CARTESIAN_POINT ( 'NONE',  ( -91.52287095715006160, -24.64965694238575011, 8.947790433994196491 ) ) ;
#23647 = LINE ( 'NONE', #38381, #89325 ) ;
#23648 = CARTESIAN_POINT ( 'NONE',  ( -22.23020047961643186, 5.420056861400933457, -1.500000000000002220 ) ) ;
#23649 = DATE_AND_TIME ( #16039, #63483 ) ;
#23650 = CARTESIAN_POINT ( 'NONE',  ( -53.01255352321339842, -14.82721238576461609, 35.59556822165056644 ) ) ;
#23651 = CARTESIAN_POINT ( 'NONE',  ( -71.29940687171418290, -25.26721001298331970, 6.088028500398946719 ) ) ;
#23652 = CARTESIAN_POINT ( 'NONE',  ( -11.57650325489309395, -16.32560983125179277, 11.49999999999999645 ) ) ;
#23653 = CARTESIAN_POINT ( 'NONE',  ( -80.06557898417501917, -25.31594321096806510, 4.529242715578940093 ) ) ;
#23654 = CARTESIAN_POINT ( 'NONE',  ( 19.72776355195876619, 6.376774720514426953, 28.39950002376592764 ) ) ;
#23655 = DIRECTION ( 'NONE',  ( 2.567145104890970367E-18, -0.9999999999976378895, -2.173523156893722419E-06 ) ) ;
#23656 = LINE ( 'NONE', #94174, #65128 ) ;
#23657 = ORIENTED_EDGE ( 'NONE', *, *, #58171, .T. ) ;
#23658 = CARTESIAN_POINT ( 'NONE',  ( -50.62287095715005592, -25.00182538069145011, 7.747789668545097541 ) ) ;
#23659 = EDGE_CURVE ( 'NONE', #44696, #6687, #13206, .T. ) ;
#23660 = CARTESIAN_POINT ( 'NONE',  ( 22.02124265030973760, 7.743225279485574042, 14.80402280011862359 ) ) ;
#23661 = CARTESIAN_POINT ( 'NONE',  ( -16.08361747308824263, -14.67194924222005170, -1.500000000000002220 ) ) ;
#23662 = CARTESIAN_POINT ( 'NONE',  ( -45.52287095715007581, -25.00182538069144655, 7.747789668545101094 ) ) ;
#23663 = CARTESIAN_POINT ( 'NONE',  ( -19.15055961920884542, -4.482958728538418924, -1.500000000000002220 ) ) ;
#23664 = CARTESIAN_POINT ( 'NONE',  ( -128.5228709571500758, -24.64898659630368627, 1.056161002820834804 ) ) ;
#23665 = EDGE_CURVE ( 'NONE', #21356, #28727, #7732, .T. ) ;
#23666 = CARTESIAN_POINT ( 'NONE',  ( -109.3640311185025098, -25.27925697487621548, 4.352105652871627761 ) ) ;
#23667 = COORDINATED_UNIVERSAL_TIME_OFFSET ( 0, 0, .AHEAD. ) ;
#23668 = CARTESIAN_POINT ( 'NONE',  ( -66.62287095715005592, -29.50250243563736774, 8.947779886222143375 ) ) ;
#23669 = DIRECTION ( 'NONE',  ( -3.773278334453079618E-23, 0.9999999999976377785, 2.173523156925979975E-06 ) ) ;
#23670 = CARTESIAN_POINT ( 'NONE',  ( 7.647619880454145758, 19.11525441646967849, 11.49999999999999645 ) ) ;
#23671 = CARTESIAN_POINT ( 'NONE',  ( -39.04717630401307105, -25.29744946566268382, 4.335755123932833577 ) ) ;
#23672 = EDGE_CURVE ( 'NONE', #41110, #53182, #18234, .T. ) ;
#23673 = CARTESIAN_POINT ( 'NONE',  ( -120.6228709571500417, -24.99132157543166954, 2.256160258750667502 ) ) ;
#23674 = ORIENTED_EDGE ( 'NONE', *, *, #47785, .F. ) ;
#23675 = CARTESIAN_POINT ( 'NONE',  ( -100.6814946224345846, -25.26387453836298747, 4.736250637429614940 ) ) ;
#23676 = CARTESIAN_POINT ( 'NONE',  ( -27.53137588795584634, -24.79921317967766825, 7.599174398616137971 ) ) ;
#23677 = CARTESIAN_POINT ( 'NONE',  ( -125.5543383043813463, -24.83644354573579349, 8.397322867130096569 ) ) ;
#23678 = CARTESIAN_POINT ( 'NONE',  ( 14.88911825943084111, -3.458829258258214523, -27.36295217134173541 ) ) ;
#23679 = CARTESIAN_POINT ( 'NONE',  ( 6.573941812937369455, -0.2639660507643297183, -9.295380466955404257E-16 ) ) ;
#23680 = EDGE_CURVE ( 'NONE', #41863, #5922, #33452, .T. ) ;
#23681 = CARTESIAN_POINT ( 'NONE',  ( -43.62287095715004881, -29.50250786944525672, 11.44777988621624232 ) ) ;
#23682 = AXIS2_PLACEMENT_3D ( 'NONE', #90689, #20670, #74466 ) ;
#23683 = ADVANCED_FACE ( 'NONE', ( #69643 ), #94412, .T. ) ;
#23684 = VERTEX_POINT ( 'NONE', #75004 ) ;
#23685 = CARTESIAN_POINT ( 'NONE',  ( 22.88022663504679599, 2.825535151426334934, 11.49999999999999645 ) ) ;
#23686 = CARTESIAN_POINT ( 'NONE',  ( 17.58993269669914383, -14.52173041563253975, -1.500000000000002220 ) ) ;
#23687 = CARTESIAN_POINT ( 'NONE',  ( 4.627238781264984446, -5.876774720514409189, 19.49219360614394247 ) ) ;
#23688 = CARTESIAN_POINT ( 'NONE',  ( -96.52217812738990688, -23.48783264082477018, -1.443836473390089914 ) ) ;
#23689 = CARTESIAN_POINT ( 'NONE',  ( -57.52287095715004739, -23.94994826722564696, -0.6494450866342742490 ) ) ;
#23690 = CARTESIAN_POINT ( 'NONE',  ( 22.22467975111640470, 2.813832150844377100, 11.49999999999999645 ) ) ;
#23691 = VERTEX_POINT ( 'NONE', #97844 ) ;
#23692 = LINE ( 'NONE', #92702, #86527 ) ;
#23693 = FACE_OUTER_BOUND ( 'NONE', #85112, .T. ) ;
#23694 = EDGE_CURVE ( 'NONE', #85301, #7254, #74024, .T. ) ;
#23695 = CARTESIAN_POINT ( 'NONE',  ( 1.885617179787854036, 21.85875792104173598, 11.49999999999998934 ) ) ;
#23696 = DIRECTION ( 'NONE',  ( 0.000000000000000000, -1.000000000000000000, -0.000000000000000000 ) ) ;
#23697 = VECTOR ( 'NONE', #74976, 1000.000000000000114 ) ;
#23698 = DIRECTION ( 'NONE',  ( 0.000000000000000000, -0.000000000000000000, 1.000000000000000000 ) ) ;
#23699 = LINE ( 'NONE', #95225, #3309 ) ;
#23700 = EDGE_LOOP ( 'NONE', ( #26979, #59168, #99518, #69319, #83363 ) ) ;
#23701 = CARTESIAN_POINT ( 'NONE',  ( -125.6228709571500559, -24.99156045073393173, 7.747789690856161648 ) ) ;
#23702 = DIRECTION ( 'NONE',  ( 0.000000000000000000, 0.000000000000000000, -1.000000000000000000 ) ) ;
#23703 = VERTEX_POINT ( 'NONE', #57814 ) ;
#23704 = VECTOR ( 'NONE', #94852, 1000.000000000000000 ) ;
#23705 = CARTESIAN_POINT ( 'NONE',  ( 12.80116962295325322, 15.99954467330607244, -1.500000000000002220 ) ) ;
#23706 = VERTEX_POINT ( 'NONE', #5502 ) ;
#23707 = VECTOR ( 'NONE', #9371, 1000.000000000000000 ) ;
#23708 = VERTEX_POINT ( 'NONE', #21217 ) ;
#23709 = ORIENTED_EDGE ( 'NONE', *, *, #74744, .T. ) ;
#23710 = ORIENTED_EDGE ( 'NONE', *, *, #81807, .F. ) ;
#23711 = CARTESIAN_POINT ( 'NONE',  ( 0.1381291366035634904, -23.06709338131901532, 11.49999999999998934 ) ) ;
#23712 = CARTESIAN_POINT ( 'NONE',  ( -39.43380829106687457, -25.30524842186639844, 5.093185296294494790 ) ) ;
#23713 = CARTESIAN_POINT ( 'NONE',  ( 2.303441031721801480, -20.17751241584783628, -1.500000000000002220 ) ) ;
#23714 = AXIS2_PLACEMENT_3D ( 'NONE', #26913, #12675, #97419 ) ;
#23715 = ORIENTED_EDGE ( 'NONE', *, *, #47259, .F. ) ;
#23716 = CARTESIAN_POINT ( 'NONE',  ( -65.05438548721848235, -3.316774720514426456, 29.49402280011861777 ) ) ;
#23717 = LINE ( 'NONE', #31336, #77354 ) ;
#23718 = AXIS2_PLACEMENT_3D ( 'NONE', #77950, #54156, #85080 ) ;
#23719 = CARTESIAN_POINT ( 'NONE',  ( -89.81226385320384509, -25.32787472568953646, 4.644766527794375044 ) ) ;
#23720 = CARTESIAN_POINT ( 'NONE',  ( 4.451706829556401956, -6.376774720514406525, 18.91922570401084513 ) ) ;
#23722 = ORIENTED_EDGE ( 'NONE', *, *, #84884, .F. ) ;
#23721 = CARTESIAN_POINT ( 'NONE',  ( -0.9917595143200197416, 21.46465604038169772, 11.49999999999999645 ) ) ;
#23723 = CARTESIAN_POINT ( 'NONE',  ( -75.49989344710095907, -24.52300882791530157, 0.6510814631126414787 ) ) ;
#23724 = CARTESIAN_POINT ( 'NONE',  ( -61.63194629385022694, -24.35071581493543036, 9.817618358456030592 ) ) ;
#23725 = ORIENTED_EDGE ( 'NONE', *, *, #56789, .T. ) ;
#23726 = CARTESIAN_POINT ( 'NONE',  ( 12.91705851660734972, -16.24616318834520001, 11.49999999999998934 ) ) ;
#23727 = ORIENTED_EDGE ( 'NONE', *, *, #68355, .T. ) ;
#23728 = B_SPLINE_CURVE_WITH_KNOTS ( 'NONE', 3,
 ( #31995, #55349, #40620, #16268, #86281, #62965 ),
 .UNSPECIFIED., .F., .F.,
 ( 4, 2, 4 ),
 ( 6.391158118952234240E-06, 0.001387004593080773352, 0.002767618028042594189 ),
 .UNSPECIFIED. ) ;
#23730 = ORIENTED_EDGE ( 'NONE', *, *, #31345, .T. ) ;
#23729 = LINE ( 'NONE', #16118, #37750 ) ;
#23731 = CARTESIAN_POINT ( 'NONE',  ( -75.62287095715004170, -24.82576562982390911, 8.398263435472971494 ) ) ;
#23732 = CARTESIAN_POINT ( 'NONE',  ( -53.52287095715007581, -24.51283580621364777, 0.6167428607019670439 ) ) ;
#23733 = ORIENTED_EDGE ( 'NONE', *, *, #33286, .T. ) ;
#23734 = ORIENTED_EDGE ( 'NONE', *, *, #81996, .T. ) ;
#23735 = LINE ( 'NONE', #55716, #89926 ) ;
#23736 = CARTESIAN_POINT ( 'NONE',  ( -77.62287095715007013, -24.33927499327854704, 9.819080762295822495 ) ) ;
#23737 = B_SPLINE_CURVE_WITH_KNOTS ( 'NONE', 3,
 ( #90934, #92923, #92427, #15804 ),
 .UNSPECIFIED., .F., .F.,
 ( 4, 4 ),
 ( 1.387778780781445676E-17, 0.0004038461538461435296 ),
 .UNSPECIFIED. ) ;
#23738 = CARTESIAN_POINT ( 'NONE',  ( -65.58378039220416156, -24.73486907724918282, 1.287355809206962354 ) ) ;
#23739 = CARTESIAN_POINT ( 'NONE',  ( -6.199593828526920092, 21.14725108817225419, 11.49999999999999645 ) ) ;
#23740 = CARTESIAN_POINT ( 'NONE',  ( 33.69795529655567634, -5.515143950957555496, 14.99689261510125249 ) ) ;
#23741 = CARTESIAN_POINT ( 'NONE',  ( 15.74396088501716839, 16.14010210793005839, -1.500000000000002220 ) ) ;
#23742 = VECTOR ( 'NONE', #77994, 1000.000000000000000 ) ;
#23743 = CARTESIAN_POINT ( 'NONE',  ( 11.23609023086081038, -17.74952302366565604, 11.49999999999998934 ) ) ;
#23744 = CARTESIAN_POINT ( 'NONE',  ( -105.5895376238167387, -23.47593901973091235, -1.443836447538999312 ) ) ;
#23745 = EDGE_LOOP ( 'NONE', ( #62988, #12508, #85750, #48629 ) ) ;
#23746 = ORIENTED_EDGE ( 'NONE', *, *, #5089, .T. ) ;
#23747 = CARTESIAN_POINT ( 'NONE',  ( -53.52287095715008292, -23.48783264082477018, -1.443836473390094799 ) ) ;
#23748 = DIRECTION ( 'NONE',  ( 0.000000000000000000, 0.000000000000000000, 1.000000000000000000 ) ) ;
#23749 = VERTEX_POINT ( 'NONE', #73525 ) ;
#23750 = CARTESIAN_POINT ( 'NONE',  ( -1.424071398598787397, -21.11453822904667277, -1.500000000000002220 ) ) ;
#23751 = DIRECTION ( 'NONE',  ( -1.000000000000000000, -3.773278334444167608E-23, -8.201307833595939069E-29 ) ) ;
#23752 = EDGE_CURVE ( 'NONE', #37372, #73685, #28338, .T. ) ;
#23753 = CARTESIAN_POINT ( 'NONE',  ( -59.79414125094724852, -25.20144863547804803, 6.835696751361012957 ) ) ;
#23754 = LINE ( 'NONE', #94270, #14 ) ;
#23755 = LINE ( 'NONE', #69444, #83226 ) ;
#23756 = CARTESIAN_POINT ( 'NONE',  ( -47.62287095715005592, -23.95044443724990657, 10.65354141964650125 ) ) ;
#23757 = CARTESIAN_POINT ( 'NONE',  ( 21.55033589006239936, 5.121329677682045833, -1.500000000000002220 ) ) ;
#23758 = EDGE_CURVE ( 'NONE', #27620, #28558, #21451, .T. ) ;
#23759 = CARTESIAN_POINT ( 'NONE',  ( -71.55402992468556533, -23.96119346886880308, -0.6495511937832095795 ) ) ;
#23760 = EDGE_CURVE ( 'NONE', #57700, #78091, #83115, .T. ) ;
#23761 = EDGE_LOOP ( 'NONE', ( #20910, #39936, #20462, #90927 ) ) ;
#23762 = CARTESIAN_POINT ( 'NONE',  ( -51.72290159494567519, -25.24860110716892692, 5.484618035424846383 ) ) ;
#23763 = CARTESIAN_POINT ( 'NONE',  ( -64.62287095715005592, -24.64965695001468404, 8.947790433994185832 ) ) ;
#23764 = CARTESIAN_POINT ( 'NONE',  ( -126.5558604981289790, -23.96119346886880663, -0.6495511937832031402 ) ) ;
#23765 = ADVANCED_FACE ( 'NONE', ( #19226 ), #28847, .F. ) ;
#23766 = VECTOR ( 'NONE', #29151, 1000.000000000000000 ) ;
#23767 = CARTESIAN_POINT ( 'NONE',  ( -28.47875734969026240, 6.475225279485573360, 26.43402280011862615 ) ) ;
#23768 = B_SPLINE_CURVE_WITH_KNOTS ( 'NONE', 3,
 ( #83176, #60376, #45634, #44632 ),
 .UNSPECIFIED., .F., .F.,
 ( 4, 4 ),
 ( 0.000000000000000000, 0.0001000000000000167422 ),
 .UNSPECIFIED. ) ;
#23769 = CARTESIAN_POINT ( 'NONE',  ( -84.62287095715007013, -23.48786465467241769, 11.44779295918254469 ) ) ;
#23770 = CARTESIAN_POINT ( 'NONE',  ( 18.80106323769845389, 4.952424739525837616, -1.500000000000002220 ) ) ;
#23771 = CARTESIAN_POINT ( 'NONE',  ( 17.72605931280000391, -11.99821887194124770, 11.49999999999998934 ) ) ;
#23772 = CARTESIAN_POINT ( 'NONE',  ( -38.52287095715007581, -24.51387760970724372, 9.387446482453404073 ) ) ;
#23773 = CARTESIAN_POINT ( 'NONE',  ( -110.2093792378192063, -25.30161501422653814, 5.585409209247975681 ) ) ;
#23774 = CARTESIAN_POINT ( 'NONE',  ( 30.53060340732035982, 2.682774720514426559, 19.84760796525321780 ) ) ;
#23775 = CARTESIAN_POINT ( 'NONE',  ( -101.0947412695425385, -25.27360029102344896, 3.544729148234888161 ) ) ;
#23776 = CARTESIAN_POINT ( 'NONE',  ( -18.33335541821337245, -13.34141728429830742, -1.500000000000002220 ) ) ;
#23777 = AXIS2_PLACEMENT_3D ( 'NONE', #98404, #97907, #96428 ) ;
#23778 = EDGE_CURVE ( 'NONE', #50658, #30492, #4519, .T. ) ;
#23779 = AXIS2_PLACEMENT_3D ( 'NONE', #84521, #69301, #76889 ) ;
#23780 = CARTESIAN_POINT ( 'NONE',  ( -110.6228709571500701, -25.00182538069145011, 7.747789668545099317 ) ) ;
#23781 = CARTESIAN_POINT ( 'NONE',  ( 0.000000000000000000, -2.682774720514426559, 0.000000000000000000 ) ) ;
#23782 = CARTESIAN_POINT ( 'NONE',  ( -18.60049703728633474, -6.982253431394513932, 11.49999999999999645 ) ) ;
#23783 = CARTESIAN_POINT ( 'NONE',  ( -123.6259827803453959, -23.73791477778912551, 11.05961554403169878 ) ) ;
#23784 = VECTOR ( 'NONE', #8394, 1000.000000000000000 ) ;
#23785 = CARTESIAN_POINT ( 'NONE',  ( -115.5228709571500616, -23.47596703998600631, 11.44779298504227860 ) ) ;
#23786 = ORIENTED_EDGE ( 'NONE', *, *, #64512, .F. ) ;
#23787 = FACE_OUTER_BOUND ( 'NONE', #66423, .T. ) ;
#23788 = CARTESIAN_POINT ( 'NONE',  ( -12.84880425037202656, -0.3587747205143964613, -26.59900746623529244 ) ) ;
#23789 = PLANE ( 'NONE',  #64270 ) ;
#23790 = CARTESIAN_POINT ( 'NONE',  ( -11.49108604648090548, 18.38894055434275643, 11.49999999999998934 ) ) ;
#23791 = LINE ( 'NONE', #40026, #69038 ) ;
#23793 = VECTOR ( 'NONE', #97195, 1000.000000000000000 ) ;
#23792 = CARTESIAN_POINT ( 'NONE',  ( -18.68671320864135765, 5.291888989699490509, -1.500000000000002220 ) ) ;
#23794 = FACE_OUTER_BOUND ( 'NONE', #85393, .T. ) ;
#23795 = ORIENTED_EDGE ( 'NONE', *, *, #23294, .F. ) ;
#23796 = CARTESIAN_POINT ( 'NONE',  ( 19.91419669613914678, 4.404666692190684962, 11.49999999999999645 ) ) ;
#23797 = CARTESIAN_POINT ( 'NONE',  ( -80.50431331750769459, -24.40034930558991277, 0.3402023900116063482 ) ) ;
#23798 = DIRECTION ( 'NONE',  ( 2.327730190238734579E-16, 1.000000000000000000, -8.064610422320895277E-16 ) ) ;
#23799 = B_SPLINE_CURVE_WITH_KNOTS ( 'NONE', 3,
 ( #7556, #53745, #84675, #91779 ),
 .UNSPECIFIED., .F., .F.,
 ( 4, 4 ),
 ( 0.000000000000000000, 9.999999999998897304E-05 ),
 .UNSPECIFIED. ) ;
#23800 = VERTEX_POINT ( 'NONE', #27842 ) ;
#23801 = CARTESIAN_POINT ( 'NONE',  ( -40.76800260471102177, -25.20049804043521036, 3.332830128871373088 ) ) ;
#23802 = CARTESIAN_POINT ( 'NONE',  ( 13.91401389203221406, -6.475225279485573360, 158.0376437107427137 ) ) ;
#23803 = CARTESIAN_POINT ( 'NONE',  ( -96.62287095715005592, -24.64965695001468404, 8.947790433994178727 ) ) ;
#23804 = B_SPLINE_CURVE_WITH_KNOTS ( 'NONE', 3,
 ( #57738, #3947, #64366, #42016 ),
 .UNSPECIFIED., .F., .F.,
 ( 4, 4 ),
 ( 0.5008576501881971677, 0.5098640814603130345 ),
 .UNSPECIFIED. ) ;
#23805 = CARTESIAN_POINT ( 'NONE',  ( -40.52054363820756322, -25.00182538069146432, 7.747789668545040698 ) ) ;
#23806 = LINE ( 'NONE', #8089, #31641 ) ;
#23807 = CARTESIAN_POINT ( 'NONE',  ( 1.236116150138429903, -20.07036509671028668, -1.500000000000002220 ) ) ;
#23808 = FACE_BOUND ( 'NONE', #86633, .T. ) ;
#23809 = VERTEX_POINT ( 'NONE', #58798 ) ;
#23810 = CARTESIAN_POINT ( 'NONE',  ( 22.81105451610979173, -2.682774720514426559, -18.46691820600746681 ) ) ;
#23811 = VECTOR ( 'NONE', #45353, 1000.000000000000114 ) ;
#23812 = EDGE_CURVE ( 'NONE', #3669, #642, #49358, .T. ) ;
#23813 = CARTESIAN_POINT ( 'NONE',  ( 2.875404258304424143, 22.71175023210845012, 11.49999999999999645 ) ) ;
#23814 = CARTESIAN_POINT ( 'NONE',  ( -22.67762270672801250, 1.536325718666671225, 11.49999999999998934 ) ) ;
#23815 = ORIENTED_EDGE ( 'NONE', *, *, #5552, .F. ) ;
#23816 = DIRECTION ( 'NONE',  ( -0.000000000000000000, 1.000000000000000000, -0.000000000000000000 ) ) ;
#23817 = PLANE ( 'NONE',  #18566 ) ;
#23818 = CARTESIAN_POINT ( 'NONE',  ( -59.62287095715004881, -24.64898659630367916, 1.056161002820822592 ) ) ;
#23819 = AXIS2_PLACEMENT_3D ( 'NONE', #26522, #57486, #65605 ) ;
#23820 = CARTESIAN_POINT ( 'NONE',  ( -98.52287095715007581, -23.47593901973090524, -1.443836447538996648 ) ) ;
#23821 = EDGE_CURVE ( 'NONE', #42999, #63531, #90240, .T. ) ;
#23822 = CARTESIAN_POINT ( 'NONE',  ( -128.5557741445947784, -24.15620529776629510, 10.23563542870659582 ) ) ;
#23823 = CARTESIAN_POINT ( 'NONE',  ( 0.02224039135773590858, 0.3828044741864812250, -0.3828044741864797817 ) ) ;
#23824 = EDGE_LOOP ( 'NONE', ( #26050, #31071, #89159, #89259 ) ) ;
#23825 = CARTESIAN_POINT ( 'NONE',  ( 12.54693703879240196, 16.07252283493236433, 11.49999999999998934 ) ) ;
#23826 = EDGE_LOOP ( 'NONE', ( #26120, #18752, #52037, #86109, #74201, #25641, #80256, #23746 ) ) ;
#23827 = CARTESIAN_POINT ( 'NONE',  ( 3.160899137004691717, 22.77513019406404382, 11.49999999999998934 ) ) ;
#23828 = CARTESIAN_POINT ( 'NONE',  ( -45.52287095715006870, -24.91544648472619983, 1.928969306349231028 ) ) ;
#23829 = ORIENTED_EDGE ( 'NONE', *, *, #75784, .F. ) ;
#23830 = CARTESIAN_POINT ( 'NONE',  ( -62.62287095715004881, -24.66019654487199020, 8.947790411086131712 ) ) ;
#23831 = VECTOR ( 'NONE', #62972, 1000.000000000000000 ) ;
#23832 = CARTESIAN_POINT ( 'NONE',  ( 2.904244945035652670, -6.376774720514415407, 20.04207437776001299 ) ) ;
#23833 = CARTESIAN_POINT ( 'NONE',  ( -89.52287095715006160, -24.65952944569304606, 1.056160979905700570 ) ) ;
#23835 = EDGE_LOOP ( 'NONE', ( #10989, #51765, #28092, #50101, #19447, #15509, #63594, #28517, #84114, #15206, #15122 ) ) ;
#23834 = CARTESIAN_POINT ( 'NONE',  ( -19.99249555334884221, 7.427959064407942513, 11.49999999999999645 ) ) ;
#23836 = ORIENTED_EDGE ( 'NONE', *, *, #78777, .F. ) ;
#23837 = CARTESIAN_POINT ( 'NONE',  ( 19.92104321119709098, 9.795001720801039369, 11.49999999999998934 ) ) ;
#23838 = B_SPLINE_CURVE_WITH_KNOTS ( 'NONE', 3,
 ( #66760, #49026, #87574, #69225 ),
 .UNSPECIFIED., .F., .F.,
 ( 4, 4 ),
 ( 0.9594697448489959424, 0.9604704918897616350 ),
 .UNSPECIFIED. ) ;
#23839 = CARTESIAN_POINT ( 'NONE',  ( -1.706377481887368486, -20.59057665607738130, -1.500000000000002220 ) ) ;
#23840 = VECTOR ( 'NONE', #56174, 1000.000000000000114 ) ;
#23841 = VERTEX_POINT ( 'NONE', #60308 ) ;
#23842 = VERTEX_POINT ( 'NONE', #36953 ) ;
#23843 = CARTESIAN_POINT ( 'NONE',  ( -109.6203743360497214, -25.31627411512031145, 5.518883902012535536 ) ) ;
#23844 = CARTESIAN_POINT ( 'NONE',  ( -95.50651195402215876, -24.63419186844610920, 9.035850630976922204 ) ) ;
#23845 = EDGE_LOOP ( 'NONE', ( #18076, #32316, #72755, #10244 ) ) ;
#23846 = CARTESIAN_POINT ( 'NONE',  ( -49.43404257242507782, -25.20234397918763847, 6.663189757676971858 ) ) ;
#23847 = VECTOR ( 'NONE', #75039, 1000.000000000000114 ) ;
#23848 = EDGE_LOOP ( 'NONE', ( #39851, #35387, #85907 ) ) ;
#23849 = CARTESIAN_POINT ( 'NONE',  ( 20.60020833695035236, 0.000000000000000000, 0.000000000000000000 ) ) ;
#23850 = CARTESIAN_POINT ( 'NONE',  ( -112.6228709571500417, -24.66019654487199730, 8.947790411086124607 ) ) ;
#23851 = CARTESIAN_POINT ( 'NONE',  ( -12.40256906124370673, -16.71776976679197801, -1.500000000000002220 ) ) ;
#23852 = CARTESIAN_POINT ( 'NONE',  ( -21.66901994843296819, -2.608494568651300138, 11.49999999999999645 ) ) ;
#23853 = CARTESIAN_POINT ( 'NONE',  ( -27.68651082257923335, -24.77993797811391019, 7.605672579471098871 ) ) ;
#23854 = CARTESIAN_POINT ( 'NONE',  ( -78.58187020279800095, -24.66019654487200441, 8.947790411086119278 ) ) ;
#23855 = CARTESIAN_POINT ( 'NONE',  ( 21.67916507323446496, -5.852930566066080864, -1.500000000000002220 ) ) ;
#23856 = CARTESIAN_POINT ( 'NONE',  ( -38.56093874523811849, -23.73766607897670511, -1.055555164236442689 ) ) ;
#23857 = CARTESIAN_POINT ( 'NONE',  ( -87.62287095715004170, -23.48783264082478794, -1.443836473390063269 ) ) ;
#23858 = PLANE ( 'NONE',  #44241 ) ;
#23859 = ORIENTED_EDGE ( 'NONE', *, *, #72243, .T. ) ;
#23860 = ORIENTED_EDGE ( 'NONE', *, *, #42646, .T. ) ;
#23861 = ORIENTED_EDGE ( 'NONE', *, *, #51614, .T. ) ;
#23862 = CARTESIAN_POINT ( 'NONE',  ( -19.64189229742525455, -8.423329616690555355, -1.500000000000002220 ) ) ;
#23863 = ORIENTED_EDGE ( 'NONE', *, *, #79905, .F. ) ;
#23864 = CARTESIAN_POINT ( 'NONE',  ( -20.88184962559319402, -2.832954952542597660, -1.500000000000002220 ) ) ;
#23865 = LINE ( 'NONE', #76152, #90346 ) ;
#23866 = EDGE_CURVE ( 'NONE', #35546, #67048, #47014, .T. ) ;
#23867 = CARTESIAN_POINT ( 'NONE',  ( -7.409219584043468920, -18.53548363135739052, -1.500000000000002220 ) ) ;
#23868 =( BOUNDED_CURVE ( )  B_SPLINE_CURVE ( 3, ( #45461, #68786, #83498, #30207, #99702, #37345, #36342, #28729, #44457, #28224, #59689, #52068, #99217, #13984, #60688, #61190, #90621, #82995, #91610, #43463 ),
 .UNSPECIFIED., .F., .F. ) 
 B_SPLINE_CURVE_WITH_KNOTS ( ( 4, 3, 1, 1, 3, 3, 1, 1, 3, 4 ),
 ( 0.000000000000000000, 0.1282082775799912033, 0.1695614466321895275, 0.2109146156843880737, 0.2522677847365863979, 0.7503515196349076488, 0.7917046886871055289, 0.8330578577393035200, 0.8744110267915015111, 1.000000000000000000 ),
 .UNSPECIFIED. ) 
 CURVE ( )  GEOMETRIC_REPRESENTATION_ITEM ( )  RATIONAL_B_SPLINE_CURVE ( ( 1.000039740655109810, 0.9986931415022445302, 0.9997852197113853423, 1.003315975282531802, 1.003315975282531802, 1.003315975282531802, 1.003315975282531802, 1.003315975282531802, 1.003315975282531802, 0.9773170091682806815, 0.9773170091682806815, 1.003315975282531802, 1.003315975282531802, 1.003315975282531802, 1.003315975282531802, 1.003315975282531802, 1.003315975282531802, 0.9998573533027315108, 0.9987387818499366965, 0.9999602609241470264 ) ) 
 REPRESENTATION_ITEM ( '' )  );
#23869 = DIRECTION ( 'NONE',  ( 0.000000000000000000, 0.3081562241202472352, 0.9513357669802769978 ) ) ;
#23870 = DIRECTION ( 'NONE',  ( 0.000000000000000000, -1.000000000000000000, 0.000000000000000000 ) ) ;
#23871 = CARTESIAN_POINT ( 'NONE',  ( 6.372119535971386917, -21.01724095701019479, -1.500000000000002220 ) ) ;
#23872 = CARTESIAN_POINT ( 'NONE',  ( 8.971512145086499856, -1.028487854913500810, 3.750000000000000000 ) ) ;
#23873 = ORIENTED_EDGE ( 'NONE', *, *, #60048, .F. ) ;
#23874 = CARTESIAN_POINT ( 'NONE',  ( 22.81105451610979173, 500000.0000000000582, -16.21691820600746681 ) ) ;
#23875 = EDGE_CURVE ( 'NONE', #60824, #41589, #88176, .T. ) ;
#23876 = CARTESIAN_POINT ( 'NONE',  ( -20.27875734969026311, -6.376774720514428729, 24.00402280011862288 ) ) ;
#23877 = CARTESIAN_POINT ( 'NONE',  ( -0.6367455441941621830, -20.85161220577290919, 11.49999999999999645 ) ) ;
#23878 = VECTOR ( 'NONE', #53346, 1000.000000000000114 ) ;
#23879 = EDGE_CURVE ( 'NONE', #21942, #33250, #92725, .T. ) ;
#23880 = CARTESIAN_POINT ( 'NONE',  ( 31.60706529141451426, -6.376774720514427841, 26.12024523944107557 ) ) ;
#23881 = EDGE_CURVE ( 'NONE', #95349, #85527, #6917, .T. ) ;
#23882 = CARTESIAN_POINT ( 'NONE',  ( -111.5562042904833930, -23.48786465467241769, 11.44779295918254292 ) ) ;
#23883 = CIRCLE ( 'NONE', #64422, 251.4258649670780699 ) ;
#23884 = DIRECTION ( 'NONE',  ( -3.773278334453079030E-23, 0.9999999999976377785, 2.173523156925979128E-06 ) ) ;
#23885 = CARTESIAN_POINT ( 'NONE',  ( 6.245503531335690361, -20.37428601906679759, 11.49999999999998934 ) ) ;
#23886 = CARTESIAN_POINT ( 'NONE',  ( -98.51627056919916470, -23.96169478059713498, 10.65365249895717881 ) ) ;
#23887 = ADVANCED_FACE ( 'NONE', ( #15607 ), #29338, .T. ) ;
#23888 = CARTESIAN_POINT ( 'NONE',  ( -51.24168201688318902, -25.24975565039529002, 3.737730239075333749 ) ) ;
#23889 = DIRECTION ( 'NONE',  ( 0.000000000000000000, 1.000000000000000000, 0.000000000000000000 ) ) ;
#23890 = FACE_OUTER_BOUND ( 'NONE', #70666, .T. ) ;
#23891 = CARTESIAN_POINT ( 'NONE',  ( -15.53634343318938704, 16.32316209468629253, -1.500000000000002220 ) ) ;
#23892 = B_SPLINE_CURVE_WITH_KNOTS ( 'NONE', 3,
 ( #9846, #11356, #41307, #1745, #34697, #40307, #63663, #10351, #88486, #26075, #72267, #71761, #10858, #72767, #3262, #48425 ),
 .UNSPECIFIED., .F., .F.,
 ( 4, 2, 2, 2, 2, 2, 2, 4 ),
 ( -2.611475609838436325E-05, 0.001181507984664241897, 0.001785319355045555511, 0.002389130725426869776, 0.002992942095808183173, 0.003596753466189497005, 0.004200564836570811270, 0.004804376206952124667 ),
 .UNSPECIFIED. ) ;
#23893 = B_SPLINE_SURFACE_WITH_KNOTS ( 'NONE', 3, 1, ( 
 ( #14692, #22291 ),
 ( #45164, #46661 ),
 ( #85205, #68985 ),
 ( #8087, #99426 ),
 ( #39035, #23293 ),
 ( #76088, #69984 ),
 ( #62382, #29920 ),
 ( #70493, #30920 ),
 ( #38534, #54280 ),
 ( #15696, #61391 ),
 ( #92317, #16192 ),
 ( #39540, #31930 ),
 ( #45656, #76581 ),
 ( #93311, #976 ),
 ( #62899, #471 ),
 ( #84202, #15194 ),
 ( #55278, #92813 ),
 ( #7085, #93821 ),
 ( #22788, #78080 ) ),
 .UNSPECIFIED., .F., .F., .F.,
 ( 4, 1, 1, 1, 1, 1, 1, 1, 1, 1, 1, 1, 1, 1, 1, 1, 4 ),
 ( 2, 2 ),
 ( 0.000000000000000000, 0.07952482958501205790, 0.1550999763495347628, 0.2272198200732689910, 0.2959105041914696366, 0.3620558809471779993, 0.4255201169126350269, 0.4858127192253077209, 0.5444947060018110463, 0.6014596357222257161, 0.6578405937966476102, 0.7139744721931383653, 0.7694679515974504058, 0.8261299671813285839, 0.8828853593090686402, 0.9407008816662013606, 1.000000000000000000 ),
 ( 0.000000000000000000, 1.000000000000000000 ),
 .UNSPECIFIED. ) ;
#23894 = CARTESIAN_POINT ( 'NONE',  ( -51.52287095715006870, -23.48786465467241058, 11.44779295918255002 ) ) ;
#23895 = ORIENTED_EDGE ( 'NONE', *, *, #15983, .T. ) ;
#23896 = DIRECTION ( 'NONE',  ( 0.6599726524652347326, 0.000000000000000000, -0.7512896232465895441 ) ) ;
#23897 = DIRECTION ( 'NONE',  ( -0.000000000000000000, 1.000000000000000000, -0.000000000000000000 ) ) ;
#23898 = CARTESIAN_POINT ( 'NONE',  ( -19.61143073682725202, -1.510137823221562092, 11.49999999999999645 ) ) ;
#23899 = CARTESIAN_POINT ( 'NONE',  ( -28.62287095715003815, -23.58338348806757168, -1.053490783401417552 ) ) ;
#23901 = B_SPLINE_CURVE_WITH_KNOTS ( 'NONE', 3,
 ( #52031, #52526, #75847, #29682 ),
 .UNSPECIFIED., .F., .F.,
 ( 4, 4 ),
 ( 0.000000000000000000, 9.999999999997510880E-05 ),
 .UNSPECIFIED. ) ;
#23900 = CARTESIAN_POINT ( 'NONE',  ( -39.58953762381673158, -24.64898659630366851, 1.056161002820378281 ) ) ;
#23902 = EDGE_CURVE ( 'NONE', #62329, #53678, #68902, .T. ) ;
#23903 = VERTEX_POINT ( 'NONE', #38451 ) ;
#23904 = CARTESIAN_POINT ( 'NONE',  ( -99.59615587936018244, -23.73766607897671577, -1.055555164236429144 ) ) ;
#23905 = DIRECTION ( 'NONE',  ( -1.000000000000000000, 0.000000000000000000, 0.000000000000000000 ) ) ;
#23906 = CARTESIAN_POINT ( 'NONE',  ( -90.93339583912592161, -25.25787539255926362, 3.590294762828090125 ) ) ;
#23907 = VECTOR ( 'NONE', #61864, 1000.000000000000000 ) ;
#23908 = CARTESIAN_POINT ( 'NONE',  ( -70.70074709382635092, -25.25639587447663459, 7.037036448897811880 ) ) ;
#23909 = CARTESIAN_POINT ( 'NONE',  ( 12.09797951242163805, 15.59582292391970704, -1.500000000000002220 ) ) ;
#23910 = ORIENTED_EDGE ( 'NONE', *, *, #35351, .T. ) ;
#23911 = CARTESIAN_POINT ( 'NONE',  ( 6.055070916906798217, 3.316774720512750019, -28.43998667593618990 ) ) ;
#23912 = VECTOR ( 'NONE', #85119, 1000.000000000000000 ) ;
#23913 = APPLICATION_PROTOCOL_DEFINITION ( 'international standard', 'config_control_design', 1994, #49246 ) ;
#23914 = ORIENTED_EDGE ( 'NONE', *, *, #61934, .T. ) ;
#23915 = CARTESIAN_POINT ( 'NONE',  ( 5.471383689419962337, -5.965225279485594001, -29.02273493113403902 ) ) ;
#23916 = CARTESIAN_POINT ( 'NONE',  ( -80.62287095715005592, -24.99132157543084531, 2.256160258750667502 ) ) ;
#23917 = CARTESIAN_POINT ( 'NONE',  ( -69.37717373815038968, -25.26785222005164400, 5.961561438218058839 ) ) ;
#23918 = CARTESIAN_POINT ( 'NONE',  ( -99.83839741074528717, -25.03145156749568656, 7.461409701454681631 ) ) ;
#23919 = DIRECTION ( 'NONE',  ( 0.000000000000000000, 0.08084198211964954695, -0.9967269304714136968 ) ) ;
#23920 = VECTOR ( 'NONE', #13766, 1000.000000000000000 ) ;
#23921 = CARTESIAN_POINT ( 'NONE',  ( -2.499999999999986677, 22.00000000000000000, 0.000000000000000000 ) ) ;
#23922 = CARTESIAN_POINT ( 'NONE',  ( -112.5228709571500616, -23.47596703998600631, 11.44779298504228038 ) ) ;
#23923 = CARTESIAN_POINT ( 'NONE',  ( -10.28607412905329532, -17.16720287211733975, -1.500000000000002220 ) ) ;
#23924 = B_SPLINE_CURVE_WITH_KNOTS ( 'NONE', 3,
 ( #43281, #67124, #35166, #42301, #26553, #81830 ),
 .UNSPECIFIED., .F., .F.,
 ( 4, 2, 4 ),
 ( 0.000000000000000000, 0.001380764517853249902, 0.002761529035706499803 ),
 .UNSPECIFIED. ) ;
#23925 = EDGE_CURVE ( 'NONE', #3797, #45450, #7499, .T. ) ;
#23926 = CARTESIAN_POINT ( 'NONE',  ( -99.13021050592293193, -25.27533083522742174, 3.853444758578534302 ) ) ;
#23927 = CARTESIAN_POINT ( 'NONE',  ( -116.6235094140349560, -24.66019654487199730, 8.947790411086115725 ) ) ;
#23928 = VERTEX_POINT ( 'NONE', #91236 ) ;
#23929 = EDGE_CURVE ( 'NONE', #51268, #23352, #55460, .T. ) ;
#23930 = CARTESIAN_POINT ( 'NONE',  ( -79.62973378576782579, -24.35071581493543036, 9.817618358456028815 ) ) ;
#23931 = CARTESIAN_POINT ( 'NONE',  ( -109.9559143002945234, -25.29012739791637188, 3.359997386848465606 ) ) ;
#23932 = FACE_OUTER_BOUND ( 'NONE', #36982, .T. ) ;
#23933 = DIRECTION ( 'NONE',  ( 1.251281512149627050E-16, 0.000000000000000000, -1.000000000000000000 ) ) ;
#23934 = DIRECTION ( 'NONE',  ( 0.000000000000000000, -0.9999999999976377785, -2.173523156925979975E-06 ) ) ;
#23935 = DIRECTION ( 'NONE',  ( 0.000000000000000000, 0.000000000000000000, 1.000000000000000000 ) ) ;
#23936 = DIRECTION ( 'NONE',  ( 0.000000000000000000, -2.173523156925979552E-06, 0.9999999999976378895 ) ) ;
#23937 = EDGE_CURVE ( 'NONE', #99569, #57091, #53694, .T. ) ;
#23938 = CARTESIAN_POINT ( 'NONE',  ( 5.359050311451609261, -5.876774720514419847, 21.05346524168807676 ) ) ;
#23939 = ORIENTED_EDGE ( 'NONE', *, *, #49844, .F. ) ;
#23940 = CARTESIAN_POINT ( 'NONE',  ( -8.348131891436525009, -18.51812344263101906, -1.500000000000002220 ) ) ;
#23941 = EDGE_CURVE ( 'NONE', #38564, #19712, #45746, .T. ) ;
#23942 = CARTESIAN_POINT ( 'NONE',  ( -28.58953762381673513, -24.50408623682959686, 1.056161642721338279 ) ) ;
#23943 = VECTOR ( 'NONE', #48617, 1000.000000000000000 ) ;
#23944 = CARTESIAN_POINT ( 'NONE',  ( -40.02662038540177747, -25.27394419400966541, 6.217212794464101577 ) ) ;
#23945 = ORIENTED_EDGE ( 'NONE', *, *, #28575, .T. ) ;
#23946 = LINE ( 'NONE', #615, #16145 ) ;
#23947 = CARTESIAN_POINT ( 'NONE',  ( -18.82377384687745447, 7.257840063761761051, -1.500000000000002220 ) ) ;
#23948 = CARTESIAN_POINT ( 'NONE',  ( 16.66693084842116335, 13.01107939256401913, 11.49999999999999645 ) ) ;
#23949 = CARTESIAN_POINT ( 'NONE',  ( -22.05048665130746954, -1.834114841651104832, -1.500000000000002220 ) ) ;
#23951 = CARTESIAN_POINT ( 'NONE',  ( 15.43701773751798001, -13.56989305476470875, -1.500000000000002220 ) ) ;
#23950 = CC_DESIGN_PERSON_AND_ORGANIZATION_ASSIGNMENT ( #45890, #91550, ( #34522 ) ) ;
#23952 = CARTESIAN_POINT ( 'NONE',  ( -60.58332302833671434, -24.73486907724917572, 1.287355809206962798 ) ) ;
#23953 = ORIENTED_EDGE ( 'NONE', *, *, #9579, .T. ) ;
#23954 = CARTESIAN_POINT ( 'NONE',  ( -32.62287095715004170, -24.50216790748204687, 0.6166512839542539481 ) ) ;
#23955 = ORIENTED_EDGE ( 'NONE', *, *, #37643, .T. ) ;
#23956 = CARTESIAN_POINT ( 'NONE',  ( -51.62287095715007013, -23.72747288104469732, -1.053458166803226792 ) ) ;
#23957 = CARTESIAN_POINT ( 'NONE',  ( -70.62287095715005592, -24.99132157543083821, 2.256160258750667502 ) ) ;
#23958 = EDGE_LOOP ( 'NONE', ( #77385, #4302, #77578, #90133 ) ) ;
#23959 = ORIENTED_EDGE ( 'NONE', *, *, #68767, .T. ) ;
#23960 = EDGE_LOOP ( 'NONE', ( #49449, #99307, #13976, #17202 ) ) ;
#23961 = CARTESIAN_POINT ( 'NONE',  ( -103.5895376238167245, -23.48786465467241769, 11.44779295918254114 ) ) ;
#23962 = CARTESIAN_POINT ( 'NONE',  ( 6.431189903846153300, -6.376774720514415407, 20.08974358974358765 ) ) ;
#23963 = CARTESIAN_POINT ( 'NONE',  ( -68.56536383884358088, -23.48786465467241058, 11.44779295918254824 ) ) ;
#23964 = CARTESIAN_POINT ( 'NONE',  ( 6.296002175621457475, 19.65409743616946514, -1.500000000000002220 ) ) ;
#23965 = CARTESIAN_POINT ( 'NONE',  ( 11.61936018155104833, -18.21891831228114356, 11.49999999999999645 ) ) ;
#23966 = ORIENTED_EDGE ( 'NONE', *, *, #64606, .F. ) ;
#23967 = DIRECTION ( 'NONE',  ( -3.773278334444166432E-23, 1.000000000000000000, 0.000000000000000000 ) ) ;
#23968 = LINE ( 'NONE', #69151, #69114 ) ;
#23969 = CARTESIAN_POINT ( 'NONE',  ( -4.763361739610138201, -21.85411462188651299, -1.500000000000002220 ) ) ;
#23970 = CIRCLE ( 'NONE', #20716, 91.74549126261076992 ) ;
#23971 = CARTESIAN_POINT ( 'NONE',  ( -79.35008398046767297, -25.12205589522605109, 6.078937818662843107 ) ) ;
#23972 = CARTESIAN_POINT ( 'NONE',  ( -120.6228709571499991, -24.62285846362215835, 9.038163152653522658 ) ) ;
#23973 = ORIENTED_EDGE ( 'NONE', *, *, #23422, .F. ) ;
#23974 = CARTESIAN_POINT ( 'NONE',  ( -99.72456502726817007, -25.30354620733853821, 4.451988771325939176 ) ) ;
#23975 = CARTESIAN_POINT ( 'NONE',  ( -60.52287095715006160, -23.47596703998600631, 11.44779298504228926 ) ) ;
#23976 = CARTESIAN_POINT ( 'NONE',  ( -11.35812032211249090, 17.58211214940072864, 11.49999999999998934 ) ) ;
#23977 = EDGE_LOOP ( 'NONE', ( #33580, #76263, #61371, #43453 ) ) ;
#23978 = CARTESIAN_POINT ( 'NONE',  ( -87.58953762381668184, -23.48786465467241769, 11.44779295918254114 ) ) ;
#23979 = VECTOR ( 'NONE', #58447, 1000.000000000000114 ) ;
#23980 = VERTEX_POINT ( 'NONE', #7003 ) ;
#23981 = CARTESIAN_POINT ( 'NONE',  ( -50.62287095715004881, -24.14406661707768365, 10.28769366152060449 ) ) ;
#23982 = CARTESIAN_POINT ( 'NONE',  ( 12.34367313097222763, -17.18290682204727915, -1.500000000000002220 ) ) ;
#23983 = ORIENTED_EDGE ( 'NONE', *, *, #21737, .F. ) ;
#23984 = FACE_OUTER_BOUND ( 'NONE', #32432, .T. ) ;
#23985 = CARTESIAN_POINT ( 'NONE',  ( -21.80608713477256089, -0.9339522974687717305, -1.500000000000002220 ) ) ;
#23986 = CARTESIAN_POINT ( 'NONE',  ( -7.138063944469604571, -6.376774720514408301, 19.21974929698718881 ) ) ;
#23987 = AXIS2_PLACEMENT_3D ( 'NONE', #43290, #15308, #31036 ) ;
#23988 = B_SPLINE_CURVE_WITH_KNOTS ( 'NONE', 3,
 ( #92606, #82997, #37347, #84503 ),
 .UNSPECIFIED., .F., .F.,
 ( 4, 4 ),
 ( 0.000000000000000000, 0.001530649038461562306 ),
 .UNSPECIFIED. ) ;
#23989 = CARTESIAN_POINT ( 'NONE',  ( -107.5228709571501184, -23.72747288104470442, -1.053458166803225460 ) ) ;
#23990 = B_SPLINE_CURVE_WITH_KNOTS ( 'NONE', 3,
 ( #95880, #57346, #88279, #18748 ),
 .UNSPECIFIED., .F., .F.,
 ( 4, 4 ),
 ( 0.5802002312608413037, 0.5892066625329569485 ),
 .UNSPECIFIED. ) ;
#23991 = CARTESIAN_POINT ( 'NONE',  ( -116.6228709571501412, -23.96127896941633750, -0.6493128931037774887 ) ) ;
#23992 = CARTESIAN_POINT ( 'NONE',  ( 4.771108217193557266, 21.26182814020628697, -1.500000000000002220 ) ) ;
#23993 = DIRECTION ( 'NONE',  ( -1.000000000000000000, 0.000000000000000000, 0.000000000000000000 ) ) ;
#23994 = ADVANCED_FACE ( 'NONE', ( #37950 ), #31338, .T. ) ;
#23995 = ORIENTED_EDGE ( 'NONE', *, *, #85544, .T. ) ;
#23996 = DIRECTION ( 'NONE',  ( 1.000000000000000000, 0.000000000000000000, 0.000000000000000000 ) ) ;
#23997 = CARTESIAN_POINT ( 'NONE',  ( -85.54292597230013939, -24.73531770709095312, 8.716586749053508498 ) ) ;
#23998 = ORIENTED_EDGE ( 'NONE', *, *, #38089, .F. ) ;
#23999 = ORIENTED_EDGE ( 'NONE', *, *, #71105, .T. ) ;
#24000 = TOROIDAL_SURFACE ( 'NONE', #9453, 3.060000000000000053, 2.040000000000000036 ) ;
#24001 = ORIENTED_EDGE ( 'NONE', *, *, #19406, .T. ) ;
#24002 = EDGE_CURVE ( 'NONE', #125, #84745, #100323, .T. ) ;
#24003 = FACE_OUTER_BOUND ( 'NONE', #84013, .T. ) ;
#24004 = CARTESIAN_POINT ( 'NONE',  ( -31.24388727629347784, -24.87479601683088148, 8.247789944647559324 ) ) ;
#24005 = CARTESIAN_POINT ( 'NONE',  ( 19.38521227897113874, -8.589346653930519437, 11.49999999999998934 ) ) ;
#24006 = LINE ( 'NONE', #1689, #82228 ) ;
#24007 = EDGE_CURVE ( 'NONE', #48956, #58117, #77498, .T. ) ;
#24008 = CARTESIAN_POINT ( 'NONE',  ( -79.98156793206884174, -25.03138283009880283, 7.487049201991271552 ) ) ;
#24009 = CARTESIAN_POINT ( 'NONE',  ( 0.4987820251299121543, -0.03487823687206273449, 9.000000000000000000 ) ) ;
#24010 = DIRECTION ( 'NONE',  ( -0.4009304992412300317, -6.845827386180410961E-16, -0.9161084732596779245 ) ) ;
#24011 = CARTESIAN_POINT ( 'NONE',  ( 19.38287969867323213, 0.6573286442255052986, -1.500000000000002220 ) ) ;
#24012 = CARTESIAN_POINT ( 'NONE',  ( -39.02904432526693768, -25.20650829394578096, 6.812666491500988464 ) ) ;
#24013 = ORIENTED_EDGE ( 'NONE', *, *, #81249, .T. ) ;
#24014 = CARTESIAN_POINT ( 'NONE',  ( 13.74000504945409418, 13.82049530813991467, 11.49999999999999645 ) ) ;
#24015 = DIRECTION ( 'NONE',  ( 0.000000000000000000, 0.000000000000000000, -1.000000000000000000 ) ) ;
#24016 = CARTESIAN_POINT ( 'NONE',  ( -108.6228709571500701, -23.48783264082478794, -1.443836473390060604 ) ) ;
#24017 = EDGE_CURVE ( 'NONE', #79371, #18949, #16624, .T. ) ;
#24018 = VERTEX_POINT ( 'NONE', #63315 ) ;
#24019 = CARTESIAN_POINT ( 'NONE',  ( -103.5228709571500758, -23.47596703998600631, 11.44779298504228215 ) ) ;
#24020 = DIRECTION ( 'NONE',  ( 0.000000000000000000, 0.000000000000000000, -1.000000000000000000 ) ) ;
#24021 = CARTESIAN_POINT ( 'NONE',  ( -103.5562042904834072, -23.47593901973091235, -1.443836447539001089 ) ) ;
#24022 = CARTESIAN_POINT ( 'NONE',  ( -93.63360700857630547, -23.96169478059713498, 10.65365249895717170 ) ) ;
#24023 = CARTESIAN_POINT ( 'NONE',  ( -6.620539020842763911, -18.51205181221761720, 11.49999999999998934 ) ) ;
#24024 = B_SPLINE_CURVE_WITH_KNOTS ( 'NONE', 3,
 ( #98426, #29926, #83208, #13694 ),
 .UNSPECIFIED., .F., .F.,
 ( 4, 4 ),
 ( 0.000000000000000000, 0.0001002978966067898494 ),
 .UNSPECIFIED. ) ;
#24025 = B_SPLINE_SURFACE_WITH_KNOTS ( 'NONE', 3, 1, ( 
 ( #97011, #74177 ),
 ( #36113, #3677 ),
 ( #26510, #4673 ),
 ( #65594, #97992 ),
 ( #28492, #88407 ),
 ( #59454, #65096 ),
 ( #90399, #28003 ),
 ( #35622, #66596 ),
 ( #58960, #20874 ),
 ( #51845, #81288 ),
 ( #82778, #11772 ),
 ( #73678, #13260 ),
 ( #34124, #18882 ),
 ( #27512, #57972 ),
 ( #19874, #50849 ),
 ( #81788, #68068 ),
 ( #30488, #76646 ),
 ( #84773, #52836 ),
 ( #99491, #59964 ) ),
 .UNSPECIFIED., .F., .F., .F.,
 ( 4, 1, 1, 1, 1, 1, 1, 1, 1, 1, 1, 1, 1, 1, 1, 1, 4 ),
 ( 2, 2 ),
 ( 0.000000000000000000, 0.06871184072392559627, 0.1348120656080472046, 0.1995375926079888951, 0.2633349351079785627, 0.3267474805653824976, 0.3903284830692779206, 0.4541258255692630641, 0.5192033216913150007, 0.5835101452921214182, 0.6454971827645034077, 0.7052898423114491999, 0.7634875795843552027, 0.8218564001280685982, 0.8800042732065155304, 0.9391077098979025983, 1.000000000000000000 ),
 ( 0.000000000000000000, 1.000000000000000000 ),
 .UNSPECIFIED. ) ;
#24026 = CARTESIAN_POINT ( 'NONE',  ( -41.44897309030830712, -25.31583615692164102, 4.366647674295371928 ) ) ;
#24027 = EDGE_LOOP ( 'NONE', ( #8634, #71669, #81226, #13117 ) ) ;
#24028 = CARTESIAN_POINT ( 'NONE',  ( -13.01863397230089170, 17.21462230531794901, -1.500000000000002220 ) ) ;
#24029 = CARTESIAN_POINT ( 'NONE',  ( -40.47472236188045258, -24.83618233451449342, 1.606449574219539711 ) ) ;
#24030 = DIRECTION ( 'NONE',  ( 0.000000000000000000, 0.000000000000000000, 1.000000000000000000 ) ) ;
#24031 = CARTESIAN_POINT ( 'NONE',  ( 3.535601659403828201, -22.84449096179584160, -1.500000000000002220 ) ) ;
#24032 = APPROVAL_STATUS ( 'not_yet_approved' ) ;
#24033 = DIRECTION ( 'NONE',  ( -1.000000000000000000, -3.773278334444167608E-23, -8.201307833595939069E-29 ) ) ;
#24034 = CARTESIAN_POINT ( 'NONE',  ( 4.573489327750471567, -6.376774720514420736, 20.79634280254998657 ) ) ;
#24035 = CARTESIAN_POINT ( 'NONE',  ( -42.62287095715004881, -23.47593901973091235, -1.443836447539011525 ) ) ;
#24036 = CARTESIAN_POINT ( 'NONE',  ( -120.5228709571500616, -23.48786465467241769, 11.44779295918253759 ) ) ;
#24037 = CARTESIAN_POINT ( 'NONE',  ( -109.7472523716161419, -25.20850093776611089, 3.466865132916900460 ) ) ;
#24038 = CARTESIAN_POINT ( 'NONE',  ( -129.5898459675138952, -23.96119346886881019, -0.6495511937831975890 ) ) ;
#24039 = CARTESIAN_POINT ( 'NONE',  ( -114.6235148883246637, -24.66019654487200441, 8.947790411086106843 ) ) ;
#24040 = CARTESIAN_POINT ( 'NONE',  ( -15.73602684802347440, -12.20685706852216867, 11.49999999999998934 ) ) ;
#24041 = FACE_OUTER_BOUND ( 'NONE', #58921, .T. ) ;
#24042 = CARTESIAN_POINT ( 'NONE',  ( -9.893332137849947472, -17.22304987741864579, -1.500000000000002220 ) ) ;
#24043 = AXIS2_PLACEMENT_3D ( 'NONE', #15298, #84313, #30023 ) ;
#24044 = CARTESIAN_POINT ( 'NONE',  ( -32.62287095715006302, -23.47596703998600276, 11.44779298504227505 ) ) ;
#24045 = EDGE_CURVE ( 'NONE', #85108, #2769, #98930, .T. ) ;
#24046 = CARTESIAN_POINT ( 'NONE',  ( -39.22373867983765194, -25.10925741625206342, 3.518977594474388848 ) ) ;
#24047 = CARTESIAN_POINT ( 'NONE',  ( -29.49875734969025842, -0.3587747205144262708, 15.62202280011862321 ) ) ;
#24048 = CARTESIAN_POINT ( 'NONE',  ( 10.28901978357889035, -18.02705789925236957, 11.49999999999999645 ) ) ;
#24049 = FACE_OUTER_BOUND ( 'NONE', #17260, .T. ) ;
#24050 = EDGE_CURVE ( 'NONE', #59175, #64167, #29923, .T. ) ;
#24051 = FACE_OUTER_BOUND ( 'NONE', #63050, .T. ) ;
#24053 = EDGE_CURVE ( 'NONE', #86736, #22711, #39457, .T. ) ;
#24052 = CARTESIAN_POINT ( 'NONE',  ( 0.9741843557120299923, -22.74547949729550922, 11.49999999999999645 ) ) ;
#24054 = ORIENTED_EDGE ( 'NONE', *, *, #92093, .T. ) ;
#24055 = CARTESIAN_POINT ( 'NONE',  ( -32.62287095715004881, -29.50247984919015209, -1.443849546365062242 ) ) ;
#24056 = CARTESIAN_POINT ( 'NONE',  ( -7.749999999999996447, 25.69999999999999574, 2.100000000000000089 ) ) ;
#24057 = ORIENTED_EDGE ( 'NONE', *, *, #10243, .F. ) ;
#24058 = VECTOR ( 'NONE', #92321, 1000.000000000000000 ) ;
#24059 = CARTESIAN_POINT ( 'NONE',  ( -20.17641613807547785, 1.360797614858565874, 11.49999999999998934 ) ) ;
#24060 = CARTESIAN_POINT ( 'NONE',  ( -56.62287095715005592, -29.50250786944525672, 11.44777988621623876 ) ) ;
#24061 = LINE ( 'NONE', #94076, #52844 ) ;
#24062 = B_SPLINE_CURVE_WITH_KNOTS ( 'NONE', 3,
 ( #51286, #35567, #96957, #97457 ),
 .UNSPECIFIED., .F., .F.,
 ( 4, 4 ),
 ( 0.000000000000000000, 9.999999999998897304E-05 ),
 .UNSPECIFIED. ) ;
#24063 = ORIENTED_EDGE ( 'NONE', *, *, #69313, .F. ) ;
#24064 = ORIENTED_EDGE ( 'NONE', *, *, #9242, .F. ) ;
#24065 = DIRECTION ( 'NONE',  ( -0.000000000000000000, -0.000000000000000000, -1.000000000000000000 ) ) ;
#24066 = CARTESIAN_POINT ( 'NONE',  ( -2.941484630304247450, -22.72858670154147376, -1.500000000000002220 ) ) ;
#24067 = CARTESIAN_POINT ( 'NONE',  ( -40.43756433397305017, -25.12049752546737835, 2.832404795212222659 ) ) ;
#24068 = CARTESIAN_POINT ( 'NONE',  ( -18.67883320684159543, -10.89015303950203517, -1.500000000000002220 ) ) ;
#24069 = AXIS2_PLACEMENT_3D ( 'NONE', #18812, #26443, #71616 ) ;
#24070 = FACE_OUTER_BOUND ( 'NONE', #15549, .T. ) ;
#24071 = CARTESIAN_POINT ( 'NONE',  ( -18.73635099073748833, 9.434554061794083069, 11.49999999999999645 ) ) ;
#24072 = ORIENTED_EDGE ( 'NONE', *, *, #38333, .T. ) ;
#24073 = CARTESIAN_POINT ( 'NONE',  ( 0.000000000000000000, -5.876774720514426953, 0.000000000000000000 ) ) ;
#24074 = CARTESIAN_POINT ( 'NONE',  ( -124.5891633685761803, -24.51314013834316086, 0.6176544820404203939 ) ) ;
#24075 = CARTESIAN_POINT ( 'NONE',  ( 9.413913215453616701, -19.89622248225912315, 11.49999999999998934 ) ) ;
#24076 = ADVANCED_FACE ( 'NONE', ( #55699 ), #8506, .T. ) ;
#24077 = DIRECTION ( 'NONE',  ( 0.000000000000000000, 0.000000000000000000, 1.000000000000000000 ) ) ;
#24078 = ORIENTED_EDGE ( 'NONE', *, *, #3223, .F. ) ;
#24079 = CARTESIAN_POINT ( 'NONE',  ( -49.73776537321236901, -25.18440148854909921, 3.509878368039943464 ) ) ;
#24080 = CARTESIAN_POINT ( 'NONE',  ( 26.73860345374794178, 5.356774720496559894, 19.84760796525321780 ) ) ;
#24081 = VERTEX_POINT ( 'NONE', #32846 ) ;
#24082 = CARTESIAN_POINT ( 'NONE',  ( 3.714584954927674154, -6.376774720514402972, 18.16171433633635246 ) ) ;
#24083 = ORIENTED_EDGE ( 'NONE', *, *, #24245, .T. ) ;
#24084 = EDGE_LOOP ( 'NONE', ( #27608, #48413, #46908, #95725 ) ) ;
#24085 = DIRECTION ( 'NONE',  ( 0.000000000000000000, 0.000000000000000000, -1.000000000000000000 ) ) ;
#24086 = DIRECTION ( 'NONE',  ( -0.4009304992412300317, 6.845827386180410961E-16, -0.9161084732596779245 ) ) ;
#24087 = DIRECTION ( 'NONE',  ( 0.000000000000000000, 0.000000000000000000, 1.000000000000000000 ) ) ;
#24088 = CARTESIAN_POINT ( 'NONE',  ( 13.31029742451639386, -15.53102932315203510, -1.500000000000002220 ) ) ;
#24089 = ORIENTED_EDGE ( 'NONE', *, *, #88838, .T. ) ;
#24090 = CARTESIAN_POINT ( 'NONE',  ( -100.6814946224345846, -25.30401792888237367, 5.197789011716578145 ) ) ;
#24091 = EDGE_CURVE ( 'NONE', #73894, #59704, #70407, .T. ) ;
#24092 = CARTESIAN_POINT ( 'NONE',  ( -33.62287095715005592, -24.66019654487199020, 8.947790411086138818 ) ) ;
#24093 = CARTESIAN_POINT ( 'NONE',  ( 4.143214286797170409, 4.821574250326516875, -2.677392948487098267E-15 ) ) ;
#24094 = CARTESIAN_POINT ( 'NONE',  ( -20.55991158545366204, 8.586518200734140294, 11.49999999999998934 ) ) ;
#24095 = EDGE_CURVE ( 'NONE', #80512, #43640, #85643, .T. ) ;
#24096 = CARTESIAN_POINT ( 'NONE',  ( -71.30292240304103757, -25.24939213713761887, 6.271475255338955002 ) ) ;
#24097 = CARTESIAN_POINT ( 'NONE',  ( -26.01933804882074597, -24.74254525576054320, 7.260434932203454039 ) ) ;
#24098 = EDGE_LOOP ( 'NONE', ( #17501, #16347, #67797, #505, #47329, #48228, #21222, #93094, #11228, #4886, #4110, #65430, #75382, #899, #64412, #23715, #74323, #38940, #21174, #40933 ) ) ;
#24099 = CARTESIAN_POINT ( 'NONE',  ( -2.499999999999986677, 22.00000000000000000, 0.000000000000000000 ) ) ;
#24100 = CARTESIAN_POINT ( 'NONE',  ( -9.749999999999984013, 18.74999999999999645, 2.100000000000000089 ) ) ;
#24101 = EDGE_CURVE ( 'NONE', #8769, #20357, #4610, .T. ) ;
#24102 = CARTESIAN_POINT ( 'NONE',  ( -20.74012505511919713, -1.853331690952414013, 11.49999999999998934 ) ) ;
#24103 = VERTEX_POINT ( 'NONE', #18119 ) ;
#24105 = ORIENTED_EDGE ( 'NONE', *, *, #34229, .T. ) ;
#24104 = CARTESIAN_POINT ( 'NONE',  ( 1.140932434931746582E-13, -5.876774720514426953, 21.78128695274321203 ) ) ;
#24106 = EDGE_LOOP ( 'NONE', ( #38093, #52276, #32211, #27998, #39686, #30836, #14359, #86830, #92115, #394, #47572, #3180 ) ) ;
#24107 = CARTESIAN_POINT ( 'NONE',  ( -51.49483116284216067, -25.25854422715338288, 6.426654113949027192 ) ) ;
#24108 = CARTESIAN_POINT ( 'NONE',  ( 3.785439364192078937, -20.66625369722972749, -1.500000000000002220 ) ) ;
#24109 = ORIENTED_EDGE ( 'NONE', *, *, #74914, .T. ) ;
#24110 = DIRECTION ( 'NONE',  ( -3.773278334453079618E-23, 0.9999999999976377785, 2.173523156925979975E-06 ) ) ;
#24111 = AXIS2_PLACEMENT_3D ( 'NONE', #77099, #84720, #16208 ) ;
#24112 = CARTESIAN_POINT ( 'NONE',  ( -32.52287095715006160, -29.50248528299804818, 1.056150453629029817 ) ) ;
#24113 = CARTESIAN_POINT ( 'NONE',  ( 5.865642684142210683, -5.356774720514426491, -25.36740469599890702 ) ) ;
#24114 = AXIS2_PLACEMENT_3D ( 'NONE', #82544, #66355, #97280 ) ;
#24115 = CARTESIAN_POINT ( 'NONE',  ( -40.62287095715004881, -24.52323809116983355, 9.355190652339421931 ) ) ;
#24116 = CARTESIAN_POINT ( 'NONE',  ( -49.58953762381673869, -24.64898659630528499, 1.056161002820820372 ) ) ;
#24117 = CARTESIAN_POINT ( 'NONE',  ( -64.52287095715006160, -24.64965694238407323, 8.947790433994201820 ) ) ;
#24118 = ADVANCED_FACE ( 'NONE', ( #33333 ), #25729, .F. ) ;
#24120 = ORIENTED_EDGE ( 'NONE', *, *, #94579, .F. ) ;
#24119 = CARTESIAN_POINT ( 'NONE',  ( -20.56242917251232782, -8.299981740788712870, 11.49999999999999645 ) ) ;
#24121 = LINE ( 'NONE', #8400, #22654 ) ;
#24122 = CARTESIAN_POINT ( 'NONE',  ( 6.650000000000004796, 0.000000000000000000, 18.35000000000000142 ) ) ;
#24123 = ORIENTED_EDGE ( 'NONE', *, *, #83611, .T. ) ;
#24124 = CARTESIAN_POINT ( 'NONE',  ( -7.311831771877058905, -21.45741656709679646, -1.500000000000002220 ) ) ;
#24125 = AXIS2_PLACEMENT_3D ( 'NONE', #54025, #47401, #70737 ) ;
#24127 = ORIENTED_EDGE ( 'NONE', *, *, #24224, .F. ) ;
#24126 = CARTESIAN_POINT ( 'NONE',  ( -5.891303133519534718, -6.376774720514420736, 20.71116975788854475 ) ) ;
#24128 = ORIENTED_EDGE ( 'NONE', *, *, #73256, .T. ) ;
#24129 = CARTESIAN_POINT ( 'NONE',  ( 8.160000000000000142, -10.15233964170348457, 0.003711184059992174607 ) ) ;
#24130 = EDGE_CURVE ( 'NONE', #98627, #63848, #71920, .T. ) ;
#24131 = CARTESIAN_POINT ( 'NONE',  ( 18.82035724208558491, -7.196742317222773799, 11.49999999999998934 ) ) ;
#24132 = EDGE_CURVE ( 'NONE', #19712, #7766, #34789, .T. ) ;
#24133 = DIRECTION ( 'NONE',  ( 0.000000000000000000, -0.9999999999976377785, -2.173523156925979975E-06 ) ) ;
#24134 = ORIENTED_EDGE ( 'NONE', *, *, #70162, .T. ) ;
#24135 = CIRCLE ( 'NONE', #58208, 6.594667762285751245 ) ;
#24136 = DIRECTION ( 'NONE',  ( 1.000000000000000000, 3.773278334444167608E-23, 8.201307833595939069E-29 ) ) ;
#24137 = CARTESIAN_POINT ( 'NONE',  ( 6.497064355747536268, 21.42967291005575348, -1.500000000000002220 ) ) ;
#24138 = ADVANCED_FACE ( 'NONE', ( #94735 ), #95742, .F. ) ;
#24139 = ORIENTED_EDGE ( 'NONE', *, *, #51871, .F. ) ;
#24140 = VERTEX_POINT ( 'NONE', #56200 ) ;
#24141 = DIRECTION ( 'NONE',  ( 0.000000000000000000, 0.000000000000000000, -1.000000000000000000 ) ) ;
#24142 = CARTESIAN_POINT ( 'NONE',  ( -4.141025641025642301, -6.376774720514411854, 19.63681891025641235 ) ) ;
#24143 = CARTESIAN_POINT ( 'NONE',  ( -39.64491860520665512, -25.31344806528496250, 4.759838987950200995 ) ) ;
#24144 = PLANE ( 'NONE',  #98414 ) ;
#24145 = EDGE_CURVE ( 'NONE', #62281, #47994, #94073, .T. ) ;
#24146 = DIRECTION ( 'NONE',  ( 1.000000000000000000, -0.000000000000000000, -0.000000000000000000 ) ) ;
#24147 = CARTESIAN_POINT ( 'NONE',  ( -18.05301863641116000, -7.546005365994440162, -1.500000000000002220 ) ) ;
#24148 = DIRECTION ( 'NONE',  ( 0.6599726524652352877, -0.000000000000000000, -0.7512896232465891000 ) ) ;
#24149 = ORIENTED_EDGE ( 'NONE', *, *, #84369, .T. ) ;
#24150 = CARTESIAN_POINT ( 'NONE',  ( 5.543860000110784725, 20.76261553274053284, 11.49999999999998934 ) ) ;
#24151 = DIRECTION ( 'NONE',  ( 0.000000000000000000, -0.9999999999976377785, -2.173523156925979128E-06 ) ) ;
#24152 = CARTESIAN_POINT ( 'NONE',  ( -38.52287095715006870, -23.47593901973090169, -1.443836447538997092 ) ) ;
#24153 = CARTESIAN_POINT ( 'NONE',  ( -29.49875734969025842, 0.3587747205144262708, 15.62202280011862321 ) ) ;
#24154 = FACE_OUTER_BOUND ( 'NONE', #63975, .T. ) ;
#24155 = CARTESIAN_POINT ( 'NONE',  ( -22.87863416751641310, 0.2071024363326711970, -1.500000000000002220 ) ) ;
#24156 = VECTOR ( 'NONE', #85059, 1000.000000000000227 ) ;
#24157 = SHAPE_DEFINITION_REPRESENTATION ( #80619, #32845 ) ;
#24158 = FACE_OUTER_BOUND ( 'NONE', #36305, .T. ) ;
#24159 = CARTESIAN_POINT ( 'NONE',  ( -2.656471864501908975, -5.876774720514412742, 19.66116880005639800 ) ) ;
#24160 = CARTESIAN_POINT ( 'NONE',  ( -10.14125802585430947, 17.27231531754821603, 11.49999999999999645 ) ) ;
#24161 = CARTESIAN_POINT ( 'NONE',  ( -79.44434589896187049, -25.31594384477702775, 4.820847139809496085 ) ) ;
#24162 = CYLINDRICAL_SURFACE ( 'NONE', #71176, 1.700000000000000178 ) ;
#24163 = CARTESIAN_POINT ( 'NONE',  ( -0.02075734969026423599, -5.965225279485572685, -0.08597719988137648983 ) ) ;
#24164 = CARTESIAN_POINT ( 'NONE',  ( -103.5228709571500758, -24.64898659630367916, 1.056161002820829697 ) ) ;
#24165 = ORIENTED_EDGE ( 'NONE', *, *, #31083, .F. ) ;
#24166 = CARTESIAN_POINT ( 'NONE',  ( 30.93860345374796594, -6.376774720514426953, 28.83647319851474933 ) ) ;
#24167 = CARTESIAN_POINT ( 'NONE',  ( 5.219777686717518961, -21.12652377152128480, -1.500000000000002220 ) ) ;
#24168 = CARTESIAN_POINT ( 'NONE',  ( 15.99960863614631101, 3.577630190450212577, -27.91116951066581819 ) ) ;
#24169 = CARTESIAN_POINT ( 'NONE',  ( -19.44079195400435012, 3.002763184081948200, -1.500000000000002220 ) ) ;
#24170 = CARTESIAN_POINT ( 'NONE',  ( -122.6228709571500559, -23.73907113216991860, -1.053371485793221485 ) ) ;
#24171 = ADVANCED_FACE ( 'NONE', ( #49085 ), #80015, .F. ) ;
#24172 = CARTESIAN_POINT ( 'NONE',  ( -104.5228709571500758, -23.48786465467241769, 11.44779295918254114 ) ) ;
#24173 = APPROVAL_ROLE ( '' ) ;
#24174 = CARTESIAN_POINT ( 'NONE',  ( -56.62287095715007013, -24.33927499327855060, 9.819080762295818943 ) ) ;
#24175 = PLANE ( 'NONE',  #19955 ) ;
#24176 = CARTESIAN_POINT ( 'NONE',  ( 16.23509277041898358, 12.58620111108425377, 11.49999999999999645 ) ) ;
#24177 = CARTESIAN_POINT ( 'NONE',  ( 3.825768195983636044, -5.876774720514423400, 21.47884071039599618 ) ) ;
#24178 = CARTESIAN_POINT ( 'NONE',  ( -75.62287095715004170, -29.50248789122583659, 2.256150453626215580 ) ) ;
#24180 = EDGE_CURVE ( 'NONE', #96748, #73682, #73904, .T. ) ;
#24179 = CARTESIAN_POINT ( 'NONE',  ( -21.83012794225054165, -5.757306806698124113, 11.49999999999999645 ) ) ;
#24181 = EDGE_LOOP ( 'NONE', ( #19575, #53482, #97470, #2407 ) ) ;
#24182 = CARTESIAN_POINT ( 'NONE',  ( -70.12829555472771403, -25.12219141572935044, 7.087033598080036079 ) ) ;
#24183 = CARTESIAN_POINT ( 'NONE',  ( -27.60893876761982213, -24.80447294267062830, 7.602474626589142304 ) ) ;
#24184 = CARTESIAN_POINT ( 'NONE',  ( -125.6240011470757025, -24.73531770709095312, 8.716586749053508498 ) ) ;
#24185 = CARTESIAN_POINT ( 'NONE',  ( -69.58953762381671027, -24.64965694238407323, 8.947790433994656567 ) ) ;
#24186 = B_SPLINE_CURVE_WITH_KNOTS ( 'NONE', 3,
 ( #81425, #19514, #88540, #43372 ),
 .UNSPECIFIED., .F., .F.,
 ( 4, 4 ),
 ( 0.2299501262341301644, 0.2389565575062454206 ),
 .UNSPECIFIED. ) ;
#24187 = LINE ( 'NONE', #7458, #11107 ) ;
#24188 = CARTESIAN_POINT ( 'NONE',  ( -125.5562042904834215, -23.47596703998600631, 11.44779298504227683 ) ) ;
#24189 = AXIS2_PLACEMENT_3D ( 'NONE', #29592, #75760, #74281 ) ;
#24190 = ORIENTED_EDGE ( 'NONE', *, *, #26294, .F. ) ;
#24191 = CARTESIAN_POINT ( 'NONE',  ( -79.80213995901898727, -25.26749909610970235, 5.120505659559028366 ) ) ;
#24192 = CARTESIAN_POINT ( 'NONE',  ( 22.73759373355791169, -1.750760473330008171, -1.500000000000002220 ) ) ;
#24193 = CARTESIAN_POINT ( 'NONE',  ( 4.653515142448186204, -5.876774720514414518, 19.86181745814487343 ) ) ;
#24194 = AXIS2_PLACEMENT_3D ( 'NONE', #81510, #50555, #13477 ) ;
#24195 = CARTESIAN_POINT ( 'NONE',  ( -115.5228709571501042, -24.51254535375846899, 9.355368624242137443 ) ) ;
#24196 = CARTESIAN_POINT ( 'NONE',  ( -59.66801233241169911, -25.31912262272984293, 4.489962371710368494 ) ) ;
#24197 = CARTESIAN_POINT ( 'NONE',  ( -3.217810451210200817, -22.18463865543611391, 11.49999999999999645 ) ) ;
#24198 = ORIENTED_EDGE ( 'NONE', *, *, #40617, .T. ) ;
#24199 = CIRCLE ( 'NONE', #50151, 6.594667762285751245 ) ;
#24200 = CARTESIAN_POINT ( 'NONE',  ( -3.108974358974355923, -5.876774720514426953, 21.75000000000001066 ) ) ;
#24201 = CARTESIAN_POINT ( 'NONE',  ( -12.46176837856299002, 18.05058065364367792, -1.500000000000002220 ) ) ;
#24202 = FACE_OUTER_BOUND ( 'NONE', #10914, .T. ) ;
#24203 = EDGE_CURVE ( 'NONE', #5126, #38206, #4353, .T. ) ;
#24205 = CARTESIAN_POINT ( 'NONE',  ( -110.5895376238167245, -25.00158670708909625, 2.256160236439165523 ) ) ;
#24204 = AXIS2_PLACEMENT_3D ( 'NONE', #33005, #32499, #62964 ) ;
#24206 = CARTESIAN_POINT ( 'NONE',  ( -74.55620429048340725, -23.48786465467241058, 11.44779295918255002 ) ) ;
#24207 = ORIENTED_EDGE ( 'NONE', *, *, #41645, .T. ) ;
#24208 = CARTESIAN_POINT ( 'NONE',  ( 5.271800844963591359, 6.376774720514426953, -28.56638892015329745 ) ) ;
#24209 = CARTESIAN_POINT ( 'NONE',  ( -42.62287095715004881, -29.50247984919015209, -1.443849546365060466 ) ) ;
#24210 = EDGE_LOOP ( 'NONE', ( #8945, #39371 ) ) ;
#24211 = CARTESIAN_POINT ( 'NONE',  ( -16.48689143942861079, 12.14541645011370541, -1.500000000000002220 ) ) ;
#24212 = ORIENTED_EDGE ( 'NONE', *, *, #9373, .T. ) ;
#24213 = ORIENTED_EDGE ( 'NONE', *, *, #99155, .F. ) ;
#24214 = ORIENTED_EDGE ( 'NONE', *, *, #56843, .F. ) ;
#24215 = ORIENTED_EDGE ( 'NONE', *, *, #2950, .T. ) ;
#24216 = CARTESIAN_POINT ( 'NONE',  ( 16.10802587768190008, -16.50329280669357246, 11.49999999999998934 ) ) ;
#24217 = CARTESIAN_POINT ( 'NONE',  ( -49.10797093729408402, -25.26756514004985377, 3.919560524017612124 ) ) ;
#24218 = CARTESIAN_POINT ( 'NONE',  ( -2.359408512905806443, -20.17289352931189583, -1.500000000000002220 ) ) ;
#24219 = ORIENTED_EDGE ( 'NONE', *, *, #84409, .T. ) ;
#24220 = ADVANCED_FACE ( 'NONE', ( #59186 ), #79017, .T. ) ;
#24221 = DIRECTION ( 'NONE',  ( 0.9980236263794188822, 0.000000000000000000, -0.06283980576413537855 ) ) ;
#24222 = EDGE_CURVE ( 'NONE', #9746, #15899, #67299, .T. ) ;
#24223 = CARTESIAN_POINT ( 'NONE',  ( -92.55185405631918627, -24.15543982623908192, -0.2315651400026453588 ) ) ;
#24224 = EDGE_CURVE ( 'NONE', #11368, #87961, #11771, .T. ) ;
#24225 = CARTESIAN_POINT ( 'NONE',  ( -93.62287095715007013, -23.47596703998600631, 11.44779298504227860 ) ) ;
#24226 = CARTESIAN_POINT ( 'NONE',  ( -70.53413262234137449, -24.92564183028979130, 1.928384488918253536 ) ) ;
#24228 = ORIENTED_EDGE ( 'NONE', *, *, #61709, .T. ) ;
#24227 = CARTESIAN_POINT ( 'NONE',  ( 0.6623178260406717976, 21.47796536025111536, 11.49999999999999645 ) ) ;
#24229 = DIRECTION ( 'NONE',  ( 0.000000000000000000, 0.000000000000000000, 1.000000000000000000 ) ) ;
#24230 = CARTESIAN_POINT ( 'NONE',  ( -61.52208231706953967, -23.48786465467240703, 11.44779295918255002 ) ) ;
#24231 = EDGE_CURVE ( 'NONE', #63074, #13848, #44494, .T. ) ;
#24232 = ORIENTED_EDGE ( 'NONE', *, *, #52915, .T. ) ;
#24233 = CARTESIAN_POINT ( 'NONE',  ( 20.09396958936853395, 5.161349618257207617, -1.500000000000002220 ) ) ;
#24234 = ORIENTED_EDGE ( 'NONE', *, *, #99711, .F. ) ;
#24236 = VERTEX_POINT ( 'NONE', #82015 ) ;
#24235 = CARTESIAN_POINT ( 'NONE',  ( -125.5198031208248324, -24.73486907724918638, 1.287355809206972346 ) ) ;
#24237 = CARTESIAN_POINT ( 'NONE',  ( -75.62287095715007013, -24.14406661707769075, 10.28769366152060982 ) ) ;
#24238 = CARTESIAN_POINT ( 'NONE',  ( -6.775140224358976226, -6.376774720514408301, 19.14743589743590846 ) ) ;
#24239 = ORIENTED_EDGE ( 'NONE', *, *, #9502, .F. ) ;
#24240 = ORIENTED_EDGE ( 'NONE', *, *, #36745, .T. ) ;
#24241 = CARTESIAN_POINT ( 'NONE',  ( -101.6228709571500559, -29.50250243563736774, 8.947779886222138046 ) ) ;
#24242 = CARTESIAN_POINT ( 'NONE',  ( -42.58141094947423966, -24.51419770103158413, 9.386484678747191168 ) ) ;
#24244 = ADVANCED_FACE ( 'NONE', ( #66814 ), #30718, .T. ) ;
#24243 = CARTESIAN_POINT ( 'NONE',  ( -28.07518484056776131, -24.65329974738956409, 1.661544776103349941 ) ) ;
#24245 = EDGE_CURVE ( 'NONE', #79008, #74917, #23988, .T. ) ;
#24246 = CARTESIAN_POINT ( 'NONE',  ( 21.84380375219137349, -3.031640915038902762, 11.49999999999999645 ) ) ;
#24247 = CARTESIAN_POINT ( 'NONE',  ( -89.50836770226504768, -24.35071581493543391, 9.817618358456025263 ) ) ;
#24248 = CARTESIAN_POINT ( 'NONE',  ( -3.174168706971715270, 22.36591850054903929, 11.49999999999998934 ) ) ;
#24249 = CARTESIAN_POINT ( 'NONE',  ( 19.54352652498339182, 7.673529024697476331, -1.500000000000002220 ) ) ;
#24250 = CARTESIAN_POINT ( 'NONE',  ( -105.6228709571500559, -23.47593901973091235, -1.443836447538999312 ) ) ;
#24252 = VERTEX_POINT ( 'NONE', #38825 ) ;
#24251 = PLANE ( 'NONE',  #2069 ) ;
#24253 = ORIENTED_EDGE ( 'NONE', *, *, #10527, .F. ) ;
#24254 = CARTESIAN_POINT ( 'NONE',  ( 6.184520403203631389, -5.356774720514425603, -25.32021290018218451 ) ) ;
#24255 = AXIS2_PLACEMENT_3D ( 'NONE', #17161, #1453, #15659 ) ;
#24256 = ADVANCED_FACE ( 'NONE', ( #22582 ), #6881, .F. ) ;
#24257 = CYLINDRICAL_SURFACE ( 'NONE', #76508, 2.499999999999998668 ) ;
#24258 = VERTEX_POINT ( 'NONE', #99219 ) ;
#24259 = CARTESIAN_POINT ( 'NONE',  ( 20.71511372717374755, 4.256074106246791722, 11.49999999999998934 ) ) ;
#24260 = CARTESIAN_POINT ( 'NONE',  ( -82.62287095715007013, -23.73907113216990794, -1.053371485793227924 ) ) ;
#24261 = CARTESIAN_POINT ( 'NONE',  ( -61.66375751369396596, -25.20144863547804803, 6.835696751361012957 ) ) ;
#24263 = DIRECTION ( 'NONE',  ( 3.773278334444167608E-23, -1.000000000000000000, 0.000000000000000000 ) ) ;
#24262 = VECTOR ( 'NONE', #74391, 1000.000000000000114 ) ;
#24264 = CARTESIAN_POINT ( 'NONE',  ( -89.81226385320383088, -29.50249591506787894, 5.947779886229223045 ) ) ;
#24265 = DIRECTION ( 'NONE',  ( -0.6392559695863496705, 0.000000000000000000, -0.7689940216596069522 ) ) ;
#24266 = CARTESIAN_POINT ( 'NONE',  ( -18.13406196532287140, 12.77545654309102474, -1.500000000000002220 ) ) ;
#24267 = CARTESIAN_POINT ( 'NONE',  ( -81.63689878905805131, -23.96169478059713498, 10.65365249895718591 ) ) ;
#24268 = EDGE_CURVE ( 'NONE', #17017, #14365, #31211, .T. ) ;
#24269 = ORIENTED_EDGE ( 'NONE', *, *, #32284, .F. ) ;
#24270 = CARTESIAN_POINT ( 'NONE',  ( 5.271800844830267785, 3.316774720514427344, -28.56638892017480913 ) ) ;
#24271 = CARTESIAN_POINT ( 'NONE',  ( -48.62287095715004881, -24.64898659630528144, 1.056161002820821038 ) ) ;
#24272 = CARTESIAN_POINT ( 'NONE',  ( -40.17542836734610745, -25.30419542993397641, 5.528894015552427099 ) ) ;
#24274 = AXIS2_PLACEMENT_3D ( 'NONE', #71313, #55595, #86524 ) ;
#24273 = B_SPLINE_CURVE_WITH_KNOTS ( 'NONE', 3,
 ( #97696, #83461, #51536, #21061 ),
 .UNSPECIFIED., .F., .F.,
 ( 4, 4 ),
 ( 0.000000000000000000, 1.000000000000000000 ),
 .UNSPECIFIED. ) ;
#24275 = EDGE_CURVE ( 'NONE', #78876, #29283, #90622, .T. ) ;
#24276 = CARTESIAN_POINT ( 'NONE',  ( -100.5461034797779547, -24.83618233451451118, 1.606449574219533050 ) ) ;
#24277 = PLANE ( 'NONE',  #98774 ) ;
#24278 = ADVANCED_FACE ( 'NONE', ( #13489 ), #21100, .T. ) ;
#24279 = AXIS2_PLACEMENT_3D ( 'NONE', #47092, #94749, #93245 ) ;
#24280 = CARTESIAN_POINT ( 'NONE',  ( 19.32586673001642197, -2.567307930040524599, -1.500000000000002220 ) ) ;
#24281 = VECTOR ( 'NONE', #23409, 1000.000000000000114 ) ;
#24282 = CARTESIAN_POINT ( 'NONE',  ( -8.434714792116727367, -19.68496499552307455, -1.500000000000002220 ) ) ;
#24283 = CARTESIAN_POINT ( 'NONE',  ( -62.53525840560303095, -24.65952944569303895, 1.056160979905693686 ) ) ;
#24284 = CARTESIAN_POINT ( 'NONE',  ( -5.366453405989236813, 0.000000000000000000, 0.000000000000000000 ) ) ;
#24285 = CARTESIAN_POINT ( 'NONE',  ( -51.61379554000202319, -23.48783264082476308, -1.443836473390094133 ) ) ;
#24286 = CARTESIAN_POINT ( 'NONE',  ( -101.1478676400630405, -25.18440077821660239, 3.600571543962751253 ) ) ;
#24287 = CARTESIAN_POINT ( 'NONE',  ( -21.16080155796574047, 8.166215375980355518, -1.500000000000002220 ) ) ;
#24288 = CIRCLE ( 'NONE', #22667, 1.835999999999983423 ) ;
#24289 = CARTESIAN_POINT ( 'NONE',  ( 18.22465585706453339, -0.5000000000000000000, -2.153101996372891236 ) ) ;
#24290 = CARTESIAN_POINT ( 'NONE',  ( -0.02075734969026423599, 6.475225279485573360, -0.08597719988137648983 ) ) ;
#24291 = CARTESIAN_POINT ( 'NONE',  ( 19.41305359857673096, 4.112862643401165919, 11.49999999999999645 ) ) ;
#24292 = CARTESIAN_POINT ( 'NONE',  ( 5.495499487697820484, -6.376774720514418959, 20.18701882043406926 ) ) ;
#24293 = DIRECTION ( 'NONE',  ( -1.000000000000000000, 0.000000000000000000, 1.526034937513432889E-15 ) ) ;
#24294 = LINE ( 'NONE', #80080, #60270 ) ;
#24295 = ORIENTED_EDGE ( 'NONE', *, *, #35385, .F. ) ;
#24296 = CARTESIAN_POINT ( 'NONE',  ( -11.64875734969026233, -5.965225279485572685, 31.02402280011862246 ) ) ;
#24297 = PLANE ( 'NONE',  #66948 ) ;
#24298 = CARTESIAN_POINT ( 'NONE',  ( -37.62287095715006302, -24.65952944569304250, 1.056160979905693020 ) ) ;
#24299 = CARTESIAN_POINT ( 'NONE',  ( -15.83346750871019992, -14.79491179806518630, 11.49999999999998934 ) ) ;
#24300 = CARTESIAN_POINT ( 'NONE',  ( -56.58743753624276707, -24.35071581493543391, 9.817618358456030592 ) ) ;
#24301 = CARTESIAN_POINT ( 'NONE',  ( -14.69715086760845857, -12.76062437926726290, -1.500000000000002220 ) ) ;
#24302 = CARTESIAN_POINT ( 'NONE',  ( -61.62287095715004881, -23.48786465467240347, 11.44779295918254824 ) ) ;
#24303 = ORIENTED_EDGE ( 'NONE', *, *, #59414, .F. ) ;
#24304 = CARTESIAN_POINT ( 'NONE',  ( 17.64890103348723116, 10.21726211432410203, 11.49999999999999645 ) ) ;
#24305 = DIRECTION ( 'NONE',  ( -3.469446951953614189E-15, 1.000000000000000000, -1.734723475976807094E-15 ) ) ;
#24306 = FACE_OUTER_BOUND ( 'NONE', #42015, .T. ) ;
#24307 = VERTEX_POINT ( 'NONE', #84998 ) ;
#24308 = CARTESIAN_POINT ( 'NONE',  ( 15.00000000000000533, 0.000000000000000000, 0.000000000000000000 ) ) ;
#24309 = DIRECTION ( 'NONE',  ( -3.773278334444167608E-23, 1.000000000000000000, 0.000000000000000000 ) ) ;
#24310 = CARTESIAN_POINT ( 'NONE',  ( -84.52287095715007581, -24.66019654487199730, 8.947790411086122830 ) ) ;
#24311 = LINE ( 'NONE', #46158, #1960 ) ;
#24312 = PLANE ( 'NONE',  #17086 ) ;
#24313 = CARTESIAN_POINT ( 'NONE',  ( 11.77038589110637901, 16.27938679534767275, 11.49999999999998934 ) ) ;
#24314 = CARTESIAN_POINT ( 'NONE',  ( -109.5571235402458967, -23.73766607897670156, -1.055555164236452903 ) ) ;
#24315 = ORIENTED_EDGE ( 'NONE', *, *, #79919, .F. ) ;
#24316 = CARTESIAN_POINT ( 'NONE',  ( -66.53646650503104354, -24.66019654487199375, 8.947790411086119278 ) ) ;
#24317 = CARTESIAN_POINT ( 'NONE',  ( 21.13568926591755925, -8.834425160694816981, 11.49999999999999645 ) ) ;
#24318 = CARTESIAN_POINT ( 'NONE',  ( 20.46598465274837864, -9.837531852206524263, 11.49999999999998934 ) ) ;
#24319 = ORIENTED_EDGE ( 'NONE', *, *, #62975, .T. ) ;
#24320 = CARTESIAN_POINT ( 'NONE',  ( -30.47287095715007865, -24.66779572958783717, 8.870747851402812856 ) ) ;
#24321 = LINE ( 'NONE', #87730, #41543 ) ;
#24322 = CARTESIAN_POINT ( 'NONE',  ( -40.20933087355918900, -25.19828085996519818, 3.317003188998405960 ) ) ;
#24323 = CARTESIAN_POINT ( 'NONE',  ( -100.6228709571500559, -29.50250786944525672, 11.44777988621623166 ) ) ;
#24324 = AXIS2_PLACEMENT_3D ( 'NONE', #59055, #29083, #89991 ) ;
#24325 = CARTESIAN_POINT ( 'NONE',  ( -128.5903321797774765, -23.48786465467241769, 11.44779295918253403 ) ) ;
#24326 = EDGE_CURVE ( 'NONE', #20122, #91108, #61687, .T. ) ;
#24327 = DIRECTION ( 'NONE',  ( -0.7071067811865474617, 0.000000000000000000, -0.7071067811865476838 ) ) ;
#24328 = CARTESIAN_POINT ( 'NONE',  ( -98.95846461277810135, -25.25460634227597012, 5.689168979074962884 ) ) ;
#24329 = ORIENTED_EDGE ( 'NONE', *, *, #72565, .F. ) ;
#24330 = EDGE_CURVE ( 'NONE', #86922, #17186, #72357, .T. ) ;
#24331 = AXIS2_PLACEMENT_3D ( 'NONE', #38688, #22450, #76244 ) ;
#24332 = CARTESIAN_POINT ( 'NONE',  ( -9.549598871097368047, 18.00506641634745009, -1.500000000000002220 ) ) ;
#24334 = EDGE_CURVE ( 'NONE', #29240, #13848, #5883, .T. ) ;
#24333 = VERTEX_POINT ( 'NONE', #52070 ) ;
#24335 = CARTESIAN_POINT ( 'NONE',  ( -0.3492834940180428727, 22.98956000712751546, -1.500000000000002220 ) ) ;
#24336 = CARTESIAN_POINT ( 'NONE',  ( -63.62287095715004881, -24.64898659630528499, 1.056161002820822592 ) ) ;
#24337 = ADVANCED_FACE ( 'NONE', ( #69787 ), #264, .T. ) ;
#24338 = EDGE_LOOP ( 'NONE', ( #50105, #26544, #36084, #95457 ) ) ;
#24339 = CARTESIAN_POINT ( 'NONE',  ( -114.5228709571501327, -23.96177878511310055, 10.65340807706329507 ) ) ;
#24340 = EDGE_CURVE ( 'NONE', #30931, #65310, #59052, .T. ) ;
#24341 = EDGE_CURVE ( 'NONE', #95739, #66931, #91611, .T. ) ;
#24342 = VECTOR ( 'NONE', #77040, 1000.000000000000000 ) ;
#24343 = CARTESIAN_POINT ( 'NONE',  ( -116.5120864331906319, -25.30063104534080054, 5.394122295771973441 ) ) ;
#24345 = ORIENTED_EDGE ( 'NONE', *, *, #57367, .T. ) ;
#24344 = CARTESIAN_POINT ( 'NONE',  ( 18.63368790978032763, -10.32677859091227113, 11.49999999999999645 ) ) ;
#24346 = AXIS2_PLACEMENT_3D ( 'NONE', #99191, #37316, #60662 ) ;
#24347 = ORIENTED_EDGE ( 'NONE', *, *, #83499, .F. ) ;
#24348 = CARTESIAN_POINT ( 'NONE',  ( -13.35739915041183323, 17.77566839534079435, 11.49999999999998934 ) ) ;
#24349 = CARTESIAN_POINT ( 'NONE',  ( -10.67548511050313209, -17.69376651829569269, -1.500000000000002220 ) ) ;
#24350 = AXIS2_PLACEMENT_3D ( 'NONE', #64499, #64997, #71588 ) ;
#24351 = VERTEX_POINT ( 'NONE', #93107 ) ;
#24352 = PLANE ( 'NONE',  #26846 ) ;
#24353 = CARTESIAN_POINT ( 'NONE',  ( -95.50513609013532346, -24.73531770709095312, 8.716586749053508498 ) ) ;
#24354 = EDGE_LOOP ( 'NONE', ( #65632, #6672, #91876, #44693, #38808, #82771 ) ) ;
#24355 = FACE_OUTER_BOUND ( 'NONE', #28949, .T. ) ;
#24356 = VERTEX_POINT ( 'NONE', #55570 ) ;
#24357 = DIRECTION ( 'NONE',  ( 1.000000000000000000, 3.491481338843133355E-15, 2.352173255807796056E-16 ) ) ;
#24358 = CARTESIAN_POINT ( 'NONE',  ( -70.80215084669140424, -25.14053967007993506, 6.999363323083984234 ) ) ;
#24359 = CARTESIAN_POINT ( 'NONE',  ( -9.832896139050584239, -18.40278743011522877, -1.500000000000002220 ) ) ;
#24360 = EDGE_CURVE ( 'NONE', #54291, #21668, #47953, .T. ) ;
#24361 = CARTESIAN_POINT ( 'NONE',  ( -21.80608713477256089, -0.9339522974687717305, 11.49999999999999645 ) ) ;
#24362 = CARTESIAN_POINT ( 'NONE',  ( -102.6228709571501128, -23.96177878511309345, 10.65340807706329507 ) ) ;
#24363 = CARTESIAN_POINT ( 'NONE',  ( -78.51252607565909614, -23.96169478059713498, 10.65365249895717881 ) ) ;
#24364 = CARTESIAN_POINT ( 'NONE',  ( -14.31525571501011207, 17.33968770572689166, 11.49999999999998934 ) ) ;
#24365 = DIRECTION ( 'NONE',  ( 1.000000000000000000, 0.000000000000000000, 5.238131417152343399E-15 ) ) ;
#24366 = CARTESIAN_POINT ( 'NONE',  ( -57.62287095715004881, -23.72747288104441665, -1.053458166803662666 ) ) ;
#24367 = CARTESIAN_POINT ( 'NONE',  ( -29.49875734969025842, 0.3587747205144265483, 25.61802280011862720 ) ) ;
#24369 = ORIENTED_EDGE ( 'NONE', *, *, #45458, .T. ) ;
#24368 = EDGE_CURVE ( 'NONE', #79014, #90831, #32449, .T. ) ;
#24370 = ORIENTED_EDGE ( 'NONE', *, *, #42916, .F. ) ;
#24371 = EDGE_LOOP ( 'NONE', ( #69630, #84045, #32662, #23108 ) ) ;
#24372 = ORIENTED_EDGE ( 'NONE', *, *, #4649, .F. ) ;
#24373 = CARTESIAN_POINT ( 'NONE',  ( -6.079122355442096115, 20.50309271558274915, -1.500000000000002220 ) ) ;
#24374 = CARTESIAN_POINT ( 'NONE',  ( 18.00092565640838416, -13.26076702590692769, 11.49999999999999645 ) ) ;
#24375 = VERTEX_POINT ( 'NONE', #70785 ) ;
#24376 = CARTESIAN_POINT ( 'NONE',  ( 18.71565868802652588, -9.641079743366450572, -1.500000000000002220 ) ) ;
#24377 = DIRECTION ( 'NONE',  ( -3.773278334453079030E-23, 0.9999999999976377785, 2.173523156925979128E-06 ) ) ;
#24378 = CARTESIAN_POINT ( 'NONE',  ( -15.85412420263326538, -12.13584807887712458, -1.500000000000002220 ) ) ;
#24379 = CARTESIAN_POINT ( 'NONE',  ( -15.87499999999997868, 2.877919977996279334E-16, -2.349999999999999645 ) ) ;
#24380 = LINE ( 'NONE', #28549, #82263 ) ;
#24381 = CARTESIAN_POINT ( 'NONE',  ( 16.16784302627978320, -14.93143893958281154, -1.500000000000002220 ) ) ;
#24382 = CARTESIAN_POINT ( 'NONE',  ( -83.52287095715009002, -24.50216790748204687, 0.6166512839542566127 ) ) ;
#24383 = VERTEX_POINT ( 'NONE', #33215 ) ;
#24384 = CARTESIAN_POINT ( 'NONE',  ( -38.62287095715005592, -23.47593901973091235, -1.443836447539011525 ) ) ;
#24385 = LINE ( 'NONE', #8670, #66033 ) ;
#24386 = CARTESIAN_POINT ( 'NONE',  ( -8.730572200882948053, 18.91488879456464289, 11.49999999999999645 ) ) ;
#24387 = EDGE_CURVE ( 'NONE', #49834, #95734, #62685, .T. ) ;
#24388 = CARTESIAN_POINT ( 'NONE',  ( 31.69157588030328299, -3.540801019308528197, 29.47507166493026176 ) ) ;
#24389 = DIRECTION ( 'NONE',  ( -0.9888510809027408754, -0.000000000000000000, -0.1489078231574183231 ) ) ;
#24390 = CARTESIAN_POINT ( 'NONE',  ( -48.55620429048340014, -23.47593901973091235, -1.443836447539009749 ) ) ;
#24391 = CARTESIAN_POINT ( 'NONE',  ( -8.160016139516647726, -19.69179572373923648, -1.500000000000002220 ) ) ;
#24392 = PLANE ( 'NONE',  #77437 ) ;
#24393 = CARTESIAN_POINT ( 'NONE',  ( -51.29572423414915505, -25.26926909690447332, 3.940521613042322624 ) ) ;
#24395 = EDGE_CURVE ( 'NONE', #39871, #29452, #32252, .T. ) ;
#24394 = AXIS2_PLACEMENT_3D ( 'NONE', #13995, #73916, #29232 ) ;
#24396 = LINE ( 'NONE', #18292, #38980 ) ;
#24397 = CARTESIAN_POINT ( 'NONE',  ( -5.238752036864926964, -5.876774720514410966, 19.51517878119694061 ) ) ;
#24398 = CARTESIAN_POINT ( 'NONE',  ( 8.566404662457630437, 20.85315857434707709, -1.500000000000002220 ) ) ;
#24399 = CARTESIAN_POINT ( 'NONE',  ( -83.58953762381673869, -24.66019654487199730, 8.947790411086112172 ) ) ;
#24400 = ORIENTED_EDGE ( 'NONE', *, *, #85655, .T. ) ;
#24401 = CARTESIAN_POINT ( 'NONE',  ( -79.20788237378963004, -25.30563682090317812, 5.076185341878163726 ) ) ;
#24402 = CARTESIAN_POINT ( 'NONE',  ( -4.686006777320708139, 5.965225279485572685, 29.60911411231905888 ) ) ;
#24403 = CARTESIAN_POINT ( 'NONE',  ( -6.620539020842763911, -18.51205181221761720, 11.49999999999999645 ) ) ;
#24404 = CARTESIAN_POINT ( 'NONE',  ( 32.16024265030974050, -5.965225279485572685, 14.03360796525321774 ) ) ;
#24405 = B_SPLINE_CURVE_WITH_KNOTS ( 'NONE', 3,
 ( #85725, #92827, #76097, #7597 ),
 .UNSPECIFIED., .F., .F.,
 ( 4, 4 ),
 ( 0.000000000000000000, 1.000000000000000000 ),
 .UNSPECIFIED. ) ;
#24406 = CARTESIAN_POINT ( 'NONE',  ( -119.5228709571500616, -24.50321055353805377, 9.387540953477511607 ) ) ;
#24407 = ORIENTED_EDGE ( 'NONE', *, *, #73876, .T. ) ;
#24408 = CARTESIAN_POINT ( 'NONE',  ( -99.58504710487255807, -24.65952944569304961, 1.056160979905703901 ) ) ;
#24409 = CARTESIAN_POINT ( 'NONE',  ( -55.62287095715004170, -24.62226745350437440, 0.9660975649728266168 ) ) ;
#24410 = DIRECTION ( 'NONE',  ( -4.522247983293619802E-39, -2.173523156893721996E-06, 0.9999999999976377785 ) ) ;
#24411 = LINE ( 'NONE', #72606, #7549 ) ;
#24412 = CARTESIAN_POINT ( 'NONE',  ( 19.48663422773152121, -3.193742178437300794, 11.49999999999998934 ) ) ;
#24413 = AXIS2_PLACEMENT_3D ( 'NONE', #21883, #46751, #31013 ) ;
#24414 = EDGE_LOOP ( 'NONE', ( #12998, #32548, #22441, #32194 ) ) ;
#24415 = CIRCLE ( 'NONE', #16300, 2.040000000000000036 ) ;
#24416 = CARTESIAN_POINT ( 'NONE',  ( 2.165584020960389822, 20.11889322763239107, 11.49999999999999645 ) ) ;
#24417 = CARTESIAN_POINT ( 'NONE',  ( 10.16119454606143435, 6.376774720514261752, -28.04611093484508899 ) ) ;
#24418 = AXIS2_PLACEMENT_3D ( 'NONE', #54908, #94462, #71133 ) ;
#24419 = SECURITY_CLASSIFICATION_LEVEL ( 'unclassified' ) ;
#24420 = EDGE_LOOP ( 'NONE', ( #52975, #46433, #74036, #17156 ) ) ;
#24421 = DIRECTION ( 'NONE',  ( 0.000000000000000000, -1.000000000000000000, 0.000000000000000000 ) ) ;
#24422 = DIRECTION ( 'NONE',  ( -1.000000000000000000, -0.000000000000000000, 0.000000000000000000 ) ) ;
#24423 = CARTESIAN_POINT ( 'NONE',  ( -24.90875734969025501, -5.965225279485572685, 26.43402280011862615 ) ) ;
#24424 = CARTESIAN_POINT ( 'NONE',  ( 5.742690948595683409, -6.376774720514427841, 21.62260900090680593 ) ) ;
#24425 = CARTESIAN_POINT ( 'NONE',  ( 22.65031661608460922, -2.682774720514426559, -20.71116937900381672 ) ) ;
#24426 = CARTESIAN_POINT ( 'NONE',  ( -61.52287095715004028, -23.73907113216989018, -1.053371485793255014 ) ) ;
#24427 = CARTESIAN_POINT ( 'NONE',  ( -19.32702923155483177, -5.217993511516596961, 11.49999999999998934 ) ) ;
#24428 = CARTESIAN_POINT ( 'NONE',  ( -34.62287095715005592, -24.64898659630367206, 1.056161002820817485 ) ) ;
#24429 = CARTESIAN_POINT ( 'NONE',  ( 31.37501302269236092, -4.132774720514428068, -3.717120176012354449 ) ) ;
#24430 = EDGE_LOOP ( 'NONE', ( #13280, #61689, #37333, #23983 ) ) ;
#24431 = CARTESIAN_POINT ( 'NONE',  ( 24.50000000000000000, 0.000000000000000000, -2.000000000000000000 ) ) ;
#24432 = CARTESIAN_POINT ( 'NONE',  ( -110.1380102904055178, -25.29012728827590450, 3.309553723195009400 ) ) ;
#24433 = CARTESIAN_POINT ( 'NONE',  ( -58.52287095715006160, -23.48786465467241058, 11.44779295918254824 ) ) ;
#24434 = CARTESIAN_POINT ( 'NONE',  ( -106.5228709571500758, -23.48786465467242479, 11.44779295918253936 ) ) ;
#24435 = CARTESIAN_POINT ( 'NONE',  ( -117.2170317540820861, -25.33540041250693875, 3.690481496468084988 ) ) ;
#24436 = CARTESIAN_POINT ( 'NONE',  ( -83.55442932252776700, -23.96119346886880663, -0.6495511937832110227 ) ) ;
#24437 = LINE ( 'NONE', #86347, #39831 ) ;
#24438 = EDGE_CURVE ( 'NONE', #37312, #30827, #46816, .T. ) ;
#24439 = CARTESIAN_POINT ( 'NONE',  ( -99.90616583242666593, -25.25978491487772004, 3.590542621692357717 ) ) ;
#24440 = ORIENTED_EDGE ( 'NONE', *, *, #23048, .T. ) ;
#24441 = EDGE_CURVE ( 'NONE', #93762, #20861, #1280, .T. ) ;
#24442 = CARTESIAN_POINT ( 'NONE',  ( 19.34776771173714849, 6.126202725962671458, -1.500000000000002220 ) ) ;
#24443 = B_SPLINE_CURVE_WITH_KNOTS ( 'NONE', 3,
 ( #41864, #19501, #66711, #73790 ),
 .UNSPECIFIED., .F., .F.,
 ( 4, 4 ),
 ( 0.6502502522661839368, 0.6592566835382995816 ),
 .UNSPECIFIED. ) ;
#24444 = CARTESIAN_POINT ( 'NONE',  ( 31.63587494018430135, 3.477878053198200536, 27.33969830395653844 ) ) ;
#24445 = EDGE_CURVE ( 'NONE', #59566, #88484, #10377, .T. ) ;
#24446 = B_SPLINE_CURVE_WITH_KNOTS ( 'NONE', 3,
 ( #68238, #92061, #37286, #93547 ),
 .UNSPECIFIED., .F., .F.,
 ( 4, 4 ),
 ( 0.3800573141027208113, 0.3890637453748362340 ),
 .UNSPECIFIED. ) ;
#24447 = CARTESIAN_POINT ( 'NONE',  ( -59.52207684527606801, -23.48786465467241058, 11.44779295918255357 ) ) ;
#24448 = EDGE_CURVE ( 'NONE', #96886, #99590, #37105, .T. ) ;
#24449 = ORIENTED_EDGE ( 'NONE', *, *, #26241, .T. ) ;
#24450 = CARTESIAN_POINT ( 'NONE',  ( -94.58953762381672448, -23.47596703998600631, 11.44779298504227683 ) ) ;
#24451 = CARTESIAN_POINT ( 'NONE',  ( -15.75104486599040321, 12.61009050114280861, -1.500000000000002220 ) ) ;
#24452 = EDGE_CURVE ( 'NONE', #92846, #6893, #79531, .T. ) ;
#24453 = CARTESIAN_POINT ( 'NONE',  ( -4.502559807402421121, -20.62786074129878955, 11.49999999999999645 ) ) ;
#24454 = CARTESIAN_POINT ( 'NONE',  ( -19.88706384024380824, 9.709922325909349894, 11.49999999999998934 ) ) ;
#24455 = EDGE_CURVE ( 'NONE', #34094, #5846, #19067, .T. ) ;
#24456 = VECTOR ( 'NONE', #69714, 1000.000000000000114 ) ;
#24457 = CARTESIAN_POINT ( 'NONE',  ( -19.39287000742378453, 6.875061630626206011, 11.49999999999998934 ) ) ;
#24458 = CARTESIAN_POINT ( 'NONE',  ( -55.52287095715008292, -24.82558206586143612, 1.605769216559449486 ) ) ;
#24459 = VERTEX_POINT ( 'NONE', #43830 ) ;
#24460 = DIRECTION ( 'NONE',  ( -1.000000000000000000, 9.637352644315600173E-17, 0.000000000000000000 ) ) ;
#24461 = VERTEX_POINT ( 'NONE', #74764 ) ;
#24462 = PLANE ( 'NONE',  #65694 ) ;
#24463 = CARTESIAN_POINT ( 'NONE',  ( -29.49875734969026198, -0.3587747205144265483, 10.11402280011862587 ) ) ;
#24464 = ORIENTED_EDGE ( 'NONE', *, *, #94814, .T. ) ;
#24465 = ORIENTED_EDGE ( 'NONE', *, *, #44517, .T. ) ;
#24466 = ORIENTED_EDGE ( 'NONE', *, *, #36971, .T. ) ;
#24467 = CARTESIAN_POINT ( 'NONE',  ( -100.5228709571500616, -24.99132157543084531, 2.256160258750667502 ) ) ;
#24468 = CARTESIAN_POINT ( 'NONE',  ( 6.853365600657045142, -5.876774720514415407, 20.20310688689519196 ) ) ;
#24469 = CARTESIAN_POINT ( 'NONE',  ( 0.3791100739519297491, -6.376774720514418959, 20.35309744218306349 ) ) ;
#24470 = CARTESIAN_POINT ( 'NONE',  ( -20.69558417703438025, 1.077208295497980250, -1.500000000000002220 ) ) ;
#24471 = CARTESIAN_POINT ( 'NONE',  ( 21.21565077533257337, 4.556159429511043690, 11.49999999999999645 ) ) ;
#24472 = ORIENTED_EDGE ( 'NONE', *, *, #8182, .F. ) ;
#24473 = CARTESIAN_POINT ( 'NONE',  ( -106.6228709571500559, -29.50248528299804818, 1.056150453629043584 ) ) ;
#24474 = LINE ( 'NONE', #32085, #20437 ) ;
#24475 = CARTESIAN_POINT ( 'NONE',  ( 5.437191932089902480, -21.69250089042843754, 11.49999999999998934 ) ) ;
#24476 = CARTESIAN_POINT ( 'NONE',  ( -47.52204401451512439, -23.48786465467240347, 11.44779295918255002 ) ) ;
#24477 = PLANE ( 'NONE',  #54574 ) ;
#24478 = ORIENTED_EDGE ( 'NONE', *, *, #27290, .F. ) ;
#24479 = CARTESIAN_POINT ( 'NONE',  ( 33.41145047975764726, -4.538943570064878585, -12.61568413423376889 ) ) ;
#24480 = CIRCLE ( 'NONE', #60146, 1.149999999999998135 ) ;
#24481 = CARTESIAN_POINT ( 'NONE',  ( -35.47580382915101183, -24.73531770709095312, 8.716586749053508498 ) ) ;
#24482 = AXIS2_PLACEMENT_3D ( 'NONE', #42530, #73464, #10558 ) ;
#24483 = ORIENTED_EDGE ( 'NONE', *, *, #39914, .F. ) ;
#24484 = DIRECTION ( 'NONE',  ( -0.1254312216594016538, -0.000000000000000000, -0.9921023176230513441 ) ) ;
#24485 = VERTEX_POINT ( 'NONE', #59067 ) ;
#24486 = CARTESIAN_POINT ( 'NONE',  ( 32.16024265030974050, -0.3587747205144265483, 16.27760796525321751 ) ) ;
#24487 = CARTESIAN_POINT ( 'NONE',  ( -4.955175619359221351, 20.59750927568439138, -1.500000000000002220 ) ) ;
#24488 = VERTEX_POINT ( 'NONE', #33722 ) ;
#24489 = CARTESIAN_POINT ( 'NONE',  ( -50.57648070875571733, -24.92564183028979130, 1.928384488918255535 ) ) ;
#24490 = CARTESIAN_POINT ( 'NONE',  ( 1.801620404824296084, -21.73869551012647605, -1.500000000000002220 ) ) ;
#24491 = DIRECTION ( 'NONE',  ( 0.000000000000000000, -0.9999999999976377785, -2.173523156925979975E-06 ) ) ;
#24492 = DIRECTION ( 'NONE',  ( -3.773278334453079618E-23, 0.9999999999976377785, 2.173523156925979975E-06 ) ) ;
#24493 = PLANE ( 'NONE',  #66010 ) ;
#24494 = CARTESIAN_POINT ( 'NONE',  ( -21.44618410820073606, 4.064364382921047181, -1.500000000000002220 ) ) ;
#24495 = CARTESIAN_POINT ( 'NONE',  ( -30.57287095715006586, -24.48248896992290469, 0.5825846392791583783 ) ) ;
#24496 = VERTEX_POINT ( 'NONE', #19483 ) ;
#24497 = DIRECTION ( 'NONE',  ( -0.000000000000000000, -0.000000000000000000, -1.000000000000000000 ) ) ;
#24498 = DIRECTION ( 'NONE',  ( 0.000000000000000000, -0.000000000000000000, -1.000000000000000000 ) ) ;
#24499 = EDGE_LOOP ( 'NONE', ( #54364, #16271, #3231, #90270 ) ) ;
#24500 = B_SPLINE_CURVE_WITH_KNOTS ( 'NONE', 3,
 ( #67609, #97046, #6190, #83812, #27547, #90431 ),
 .UNSPECIFIED., .F., .F.,
 ( 4, 2, 4 ),
 ( -8.872634692045293004E-06, 0.0009000329399760627434, 0.001808938514644170764 ),
 .UNSPECIFIED. ) ;
#24501 = CARTESIAN_POINT ( 'NONE',  ( -129.5219154021366137, -24.35071581493544102, 9.817618358456021710 ) ) ;
#24502 = ORIENTED_EDGE ( 'NONE', *, *, #74563, .T. ) ;
#24503 = VERTEX_POINT ( 'NONE', #42358 ) ;
#24504 = CARTESIAN_POINT ( 'NONE',  ( -29.24636659180999843, -25.20264517434234364, 4.940287045316306802 ) ) ;
#24505 = CARTESIAN_POINT ( 'NONE',  ( -82.58825244796760501, -24.34968618360933945, 0.1864209137778926328 ) ) ;
#24506 = CARTESIAN_POINT ( 'NONE',  ( 17.84191302092929021, 11.53353326677314961, 11.49999999999998934 ) ) ;
#24507 = CARTESIAN_POINT ( 'NONE',  ( -94.60069243175672682, -23.48783264082477373, -1.443836473390087249 ) ) ;
#24508 = CARTESIAN_POINT ( 'NONE',  ( -41.52287095715006870, -24.65952944569304606, 1.056160979905691910 ) ) ;
#24509 = ADVANCED_FACE ( 'NONE', ( #26611 ), #66195, .F. ) ;
#24510 = CARTESIAN_POINT ( 'NONE',  ( -61.62287095715004881, -29.50248528299804818, 1.056150453629034924 ) ) ;
#24511 = CARTESIAN_POINT ( 'NONE',  ( -127.5228709571500332, -24.66019654487200441, 8.947790411086105067 ) ) ;
#24512 = CARTESIAN_POINT ( 'NONE',  ( 8.665315094346039970, 17.34094453737590769, -1.500000000000002220 ) ) ;
#24513 = EDGE_CURVE ( 'NONE', #99093, #92445, #15344, .T. ) ;
#24514 = CARTESIAN_POINT ( 'NONE',  ( -117.6250629353716590, -24.35071581493544457, 9.817618358456019934 ) ) ;
#24515 = ORIENTED_EDGE ( 'NONE', *, *, #36053, .F. ) ;
#24516 = CARTESIAN_POINT ( 'NONE',  ( -9.627943313441900131, 16.98966435471970726, 11.49999999999999645 ) ) ;
#24517 = DIRECTION ( 'NONE',  ( 0.000000000000000000, -0.000000000000000000, -1.000000000000000000 ) ) ;
#24518 = CARTESIAN_POINT ( 'NONE',  ( -79.45589157972931105, -25.21686183209924792, 6.470215754339476710 ) ) ;
#24519 = VERTEX_POINT ( 'NONE', #51447 ) ;
#24520 = CARTESIAN_POINT ( 'NONE',  ( 4.910384361841649614, -6.376774720514420736, 20.73924463800384643 ) ) ;
#24521 = CARTESIAN_POINT ( 'NONE',  ( -89.59156628431851743, -24.15543982623907482, -0.2315651400026483009 ) ) ;
#24522 = CARTESIAN_POINT ( 'NONE',  ( -30.47287095715007510, -23.47593906522708451, -1.422904450652597852 ) ) ;
#24523 = CARTESIAN_POINT ( 'NONE',  ( -55.62287095715006302, -24.63287334234180292, 0.9662140553045335256 ) ) ;
#24524 = CARTESIAN_POINT ( 'NONE',  ( -11.90832679833862073, -15.64659449181510986, -1.500000000000002220 ) ) ;
#24525 = ORIENTED_EDGE ( 'NONE', *, *, #64631, .T. ) ;
#24526 = CARTESIAN_POINT ( 'NONE',  ( 21.32721141102669193, -3.434809268862642817, 11.49999999999998934 ) ) ;
#24527 = B_SPLINE_CURVE_WITH_KNOTS ( 'NONE', 3,
 ( #68155, #69654, #29580, #7235, #60557, #100064 ),
 .UNSPECIFIED., .F., .F.,
 ( 4, 2, 4 ),
 ( 0.000000000000000000, 0.001380764517853254455, 0.002761529035706508910 ),
 .UNSPECIFIED. ) ;
#24528 = CARTESIAN_POINT ( 'NONE',  ( -85.55620429048337883, -25.00182538069145721, 7.747789668545100206 ) ) ;
#24529 = AXIS2_PLACEMENT_3D ( 'NONE', #82451, #74833, #60636 ) ;
#24530 = CARTESIAN_POINT ( 'NONE',  ( -50.62287095715005592, -29.50248528299804818, 1.056150453629033370 ) ) ;
#24531 = CARTESIAN_POINT ( 'NONE',  ( 6.977686149863070675, -22.03694335537135984, -1.500000000000002220 ) ) ;
#24533 = EDGE_CURVE ( 'NONE', #65803, #54238, #58076, .T. ) ;
#24532 = CC_DESIGN_PERSON_AND_ORGANIZATION_ASSIGNMENT ( #27304, #33920, ( #19830 ) ) ;
#24534 = APPROVAL_STATUS ( 'not_yet_approved' ) ;
#24535 = CARTESIAN_POINT ( 'NONE',  ( 3.249631081431332280, -5.876774720514423400, 21.24682042713427776 ) ) ;
#24536 = CARTESIAN_POINT ( 'NONE',  ( -121.5228709571500616, -29.50248528299804818, 1.056150453629045360 ) ) ;
#24537 = CARTESIAN_POINT ( 'NONE',  ( 9.299999999999993605, 12.00000000000002309, 2.100000000000000089 ) ) ;
#24538 = CARTESIAN_POINT ( 'NONE',  ( -101.9131232614075770, -25.23352619098501393, 6.415922869675740436 ) ) ;
#24539 = CARTESIAN_POINT ( 'NONE',  ( -110.7466941838547143, -25.29823823612047917, 2.889690974355013875 ) ) ;
#24540 = CARTESIAN_POINT ( 'NONE',  ( -110.6228709571500701, -23.48786465467241769, 11.44779295918254114 ) ) ;
#24541 = CARTESIAN_POINT ( 'NONE',  ( -99.41873814713473223, -25.31566058944073916, 4.744921480468723196 ) ) ;
#24542 = CARTESIAN_POINT ( 'NONE',  ( 5.901097582950029619, 19.04237314665466485, 11.49999999999998934 ) ) ;
#24543 = CARTESIAN_POINT ( 'NONE',  ( -75.50775092909401565, -24.15602025860895807, 10.28564288303536678 ) ) ;
#24544 = CARTESIAN_POINT ( 'NONE',  ( 8.478510716907816658, 17.93336729499101523, -1.500000000000002220 ) ) ;
#24545 = VERTEX_POINT ( 'NONE', #95618 ) ;
#24546 = CARTESIAN_POINT ( 'NONE',  ( -0.3225169060639742624, -5.876774720514411854, 19.46611907402017749 ) ) ;
#24547 = VECTOR ( 'NONE', #61383, 1000.000000000000114 ) ;
#24548 = LOCAL_TIME ( 0, 54, 15.00000000000000000, #78436 ) ;
#24549 = CARTESIAN_POINT ( 'NONE',  ( -39.44256650533377950, -25.29116604522729972, 3.228027748310828837 ) ) ;
#24550 = DIRECTION ( 'NONE',  ( 1.000000000000000000, 0.000000000000000000, -1.252131230780251939E-15 ) ) ;
#24551 = CARTESIAN_POINT ( 'NONE',  ( 3.485566553294195291, 20.44204155273375889, 11.49999999999999645 ) ) ;
#24552 = DIRECTION ( 'NONE',  ( -3.773278334453079618E-23, 0.9999999999976377785, 2.173523156925979975E-06 ) ) ;
#24553 = CARTESIAN_POINT ( 'NONE',  ( -106.5889902452000939, -24.34968618360933945, 0.1864209137778878034 ) ) ;
#24554 = CARTESIAN_POINT ( 'NONE',  ( 15.23092229589061830, -16.91372389758942418, 11.49999999999999645 ) ) ;
#24555 = ORIENTED_EDGE ( 'NONE', *, *, #4107, .T. ) ;
#24556 = CARTESIAN_POINT ( 'NONE',  ( -69.60831051794583857, -23.48783264082476308, -1.443836473390097908 ) ) ;
#24557 = CARTESIAN_POINT ( 'NONE',  ( -90.62287095715004170, -23.47596703998600631, 11.44779298504227860 ) ) ;
#24558 = ORIENTED_EDGE ( 'NONE', *, *, #43157, .T. ) ;
#24559 = CARTESIAN_POINT ( 'NONE',  ( 2.532258636284850706, -20.04889675553949147, -1.500000000000002220 ) ) ;
#24560 = CARTESIAN_POINT ( 'NONE',  ( -43.62287095715004170, -23.48786465467241058, 11.44779295918255180 ) ) ;
#24561 = DIRECTION ( 'NONE',  ( -0.1311553622875919756, -6.845827386180409975E-16, -0.9913618264504692190 ) ) ;
#24562 = ORIENTED_EDGE ( 'NONE', *, *, #42113, .T. ) ;
#24563 = CARTESIAN_POINT ( 'NONE',  ( -70.62287095715001328, -24.51254535404256529, 9.355368623467642308 ) ) ;
#24564 = CARTESIAN_POINT ( 'NONE',  ( -14.98413761715186077, 17.36544542080599740, 11.49999999999998934 ) ) ;
#24565 = CARTESIAN_POINT ( 'NONE',  ( -29.49875734969025842, 5.965225279485572685, 23.37402280011862743 ) ) ;
#24566 = CARTESIAN_POINT ( 'NONE',  ( -17.62595516807937557, -9.487554784798948759, -1.500000000000002220 ) ) ;
#24567 = FACE_OUTER_BOUND ( 'NONE', #16509, .T. ) ;
#24568 = EDGE_CURVE ( 'NONE', #39794, #43715, #83102, .T. ) ;
#24569 = CARTESIAN_POINT ( 'NONE',  ( -3.838044578953509145, 20.63102806057878880, 11.49999999999999645 ) ) ;
#24570 = CARTESIAN_POINT ( 'NONE',  ( -48.52287095715004739, -23.48783264083430211, -1.443836473375264440 ) ) ;
#24571 = CARTESIAN_POINT ( 'NONE',  ( -69.08877929746488178, -25.31612571981231596, 5.548814315813750397 ) ) ;
#24572 = CARTESIAN_POINT ( 'NONE',  ( -14.94409825380703616, 16.19114737329946507, -1.500000000000002220 ) ) ;
#24573 = EDGE_CURVE ( 'NONE', #62281, #90808, #4275, .T. ) ;
#24574 = PERSON ( 'NAUO-PER4', 'UNSPECIFIED', 'UNSPECIFIED', ('UNSPECIFIED'), ('UNSPECIFIED'), ('UNSPECIFIED') ) ;
#24575 = ORIENTED_EDGE ( 'NONE', *, *, #16893, .F. ) ;
#24576 = VECTOR ( 'NONE', #55597, 1000.000000000000114 ) ;
#24577 = CARTESIAN_POINT ( 'NONE',  ( -118.5228709571501184, -24.66019654487200441, 8.947790411086110396 ) ) ;
#24578 = CARTESIAN_POINT ( 'NONE',  ( -53.01255352321339842, -4.132774720514426292, 35.59556822165056644 ) ) ;
#24579 = ORIENTED_EDGE ( 'NONE', *, *, #28242, .F. ) ;
#24580 = CARTESIAN_POINT ( 'NONE',  ( 8.971512145086521173, -7.528487854913501920, 6.500000000000000888 ) ) ;
#24581 = ORIENTED_EDGE ( 'NONE', *, *, #92283, .F. ) ;
#24582 = B_SPLINE_CURVE_WITH_KNOTS ( 'NONE', 3,
 ( #59383, #43661, #57902, #27439, #36038, #58397, #90325, #20798, #82708, #44157 ),
 .UNSPECIFIED., .F., .F.,
 ( 4, 2, 2, 2, 4 ),
 ( 0.000000000000000000, 0.0004823517777971119314, 0.0009647035555942238627, 0.001447055333391335848, 0.001929407111188447725 ),
 .UNSPECIFIED. ) ;
#24583 = ORIENTED_EDGE ( 'NONE', *, *, #7905, .F. ) ;
#24584 = CARTESIAN_POINT ( 'NONE',  ( 4.653846153846159517, -6.376774720514415407, 19.99999999999999289 ) ) ;
#24585 = FACE_OUTER_BOUND ( 'NONE', #30022, .T. ) ;
#24587 = EDGE_CURVE ( 'NONE', #44056, #88744, #99917, .T. ) ;
#24586 = CARTESIAN_POINT ( 'NONE',  ( -4.141166922167975883, -5.876774720514419847, 20.63520656483649063 ) ) ;
#24588 = CARTESIAN_POINT ( 'NONE',  ( 10.78675619948152864, -17.38023510967517637, -1.500000000000002220 ) ) ;
#24589 = ORIENTED_EDGE ( 'NONE', *, *, #58901, .F. ) ;
#24590 = CARTESIAN_POINT ( 'NONE',  ( -106.5228709571500758, -24.66019654487200441, 8.947790411086112172 ) ) ;
#24591 = CARTESIAN_POINT ( 'NONE',  ( -44.53465503250131263, -24.51314013834316086, 0.6176544820404110681 ) ) ;
#24592 = CARTESIAN_POINT ( 'NONE',  ( -77.55620429048339304, -24.64898659630529210, 1.056161002820828809 ) ) ;
#24593 = CARTESIAN_POINT ( 'NONE',  ( -21.75032768068154354, -4.810781854073628239, -1.500000000000002220 ) ) ;
#24594 = CARTESIAN_POINT ( 'NONE',  ( -70.44736088819470865, -25.13396146398487119, 7.096960098442634646 ) ) ;
#24595 = CARTESIAN_POINT ( 'NONE',  ( -90.55620429048337883, -24.99156044556202971, 7.747789690856174083 ) ) ;
#24596 = ORIENTED_EDGE ( 'NONE', *, *, #5546, .F. ) ;
#24597 = CARTESIAN_POINT ( 'NONE',  ( -96.62287095715004170, -24.65952944569304606, 1.056160979905703456 ) ) ;
#24598 = CARTESIAN_POINT ( 'NONE',  ( -118.5228709571500758, -23.47593901973090524, -1.443836447538996204 ) ) ;
#24599 = CARTESIAN_POINT ( 'NONE',  ( -12.40256906124370673, -16.71776976679197801, 11.49999999999998934 ) ) ;
#24600 = ORIENTED_EDGE ( 'NONE', *, *, #83561, .F. ) ;
#24602 = ORIENTED_EDGE ( 'NONE', *, *, #53688, .T. ) ;
#24601 = CARTESIAN_POINT ( 'NONE',  ( 32.66876533700882845, 5.965225279485572685, -12.58926540598385557 ) ) ;
#24603 = VERTEX_POINT ( 'NONE', #96609 ) ;
#24604 = CARTESIAN_POINT ( 'NONE',  ( -50.40445135320379677, -25.25854569424054219, 7.101635264402184511 ) ) ;
#24605 = CARTESIAN_POINT ( 'NONE',  ( -17.93810645791062441, 10.97360191750010827, -1.500000000000002220 ) ) ;
#24606 = VERTEX_POINT ( 'NONE', #4769 ) ;
#24607 = DIRECTION ( 'NONE',  ( -8.659560562354873694E-17, -0.7071067811865525687, -0.7071067811865425767 ) ) ;
#24608 = CARTESIAN_POINT ( 'NONE',  ( -10.24059822343757808, -5.876774720514426953, 0.000000000000000000 ) ) ;
#24609 = CARTESIAN_POINT ( 'NONE',  ( 9.131215498121711960, -5.356774720514425603, -25.00673578072587588 ) ) ;
#24610 = CARTESIAN_POINT ( 'NONE',  ( -101.6175123368144142, -25.25419440104175095, 7.038108131071323825 ) ) ;
#24611 = CARTESIAN_POINT ( 'NONE',  ( -110.2244512850201659, -25.12087729867975483, 2.834499938438063360 ) ) ;
#24612 = CARTESIAN_POINT ( 'NONE',  ( -63.62287095715004881, -24.64898659630528499, 1.056161002820822592 ) ) ;
#24614 = ORIENTED_EDGE ( 'NONE', *, *, #82579, .F. ) ;
#24613 = CARTESIAN_POINT ( 'NONE',  ( 5.796264663052079769, -21.44337444023769379, 11.49999999999999645 ) ) ;
#24615 = LINE ( 'NONE', #40359, #37243 ) ;
#24616 = CARTESIAN_POINT ( 'NONE',  ( -71.18699820573013426, -25.28351461562841607, 5.743153344412908368 ) ) ;
#24617 = EDGE_LOOP ( 'NONE', ( #77514, #22809, #56941, #37368 ) ) ;
#24618 = CARTESIAN_POINT ( 'NONE',  ( -18.33335541821337245, -13.34141728429830742, 11.49999999999998934 ) ) ;
#24620 = EDGE_LOOP ( 'NONE', ( #83882, #43566, #93216, #37564 ) ) ;
#24619 = CARTESIAN_POINT ( 'NONE',  ( -6.033988668995577065, -6.376774720514413630, 19.86422795159478483 ) ) ;
#24621 = EDGE_CURVE ( 'NONE', #45070, #31086, #85368, .T. ) ;
#24622 = VECTOR ( 'NONE', #21142, 1000.000000000000114 ) ;
#24623 = ORIENTED_EDGE ( 'NONE', *, *, #14607, .F. ) ;
#24624 = CC_DESIGN_APPROVAL ( #88468, ( #29568 ) ) ;
#24625 = CYLINDRICAL_SURFACE ( 'NONE', #2758, 130.7884398600581335 ) ;
#24626 = EDGE_CURVE ( 'NONE', #1265, #60838, #18951, .T. ) ;
#24627 = CARTESIAN_POINT ( 'NONE',  ( -3.510519812331947875, -19.85243952969433323, 11.49999999999998934 ) ) ;
#24628 = CARTESIAN_POINT ( 'NONE',  ( 8.971512145086499856, -1.028487854913500810, 3.750000000000000000 ) ) ;
#24629 = EDGE_LOOP ( 'NONE', ( #71403, #4007, #23238 ) ) ;
#24630 = DIRECTION ( 'NONE',  ( -3.773278334453079618E-23, 0.9999999999976377785, 2.173523156925979975E-06 ) ) ;
#24631 = CARTESIAN_POINT ( 'NONE',  ( -22.40390758644239710, -1.035154934579901820, -1.500000000000002220 ) ) ;
#24632 = B_SPLINE_CURVE_WITH_KNOTS ( 'NONE', 3,
 ( #11335, #42311, #26056, #50404, #57028, #73729 ),
 .UNSPECIFIED., .F., .F.,
 ( 4, 2, 4 ),
 ( 6.396480873082856813E-06, 0.001387752211907360709, 0.002769107942941638652 ),
 .UNSPECIFIED. ) ;
#24633 = ORIENTED_EDGE ( 'NONE', *, *, #24050, .F. ) ;
#24634 = VERTEX_POINT ( 'NONE', #20477 ) ;
#24635 = CARTESIAN_POINT ( 'NONE',  ( 32.16024265030974050, 5.965225279485572685, 16.27760796525321751 ) ) ;
#24636 = CARTESIAN_POINT ( 'NONE',  ( -4.312370003044874167, -6.376774720514408301, 19.42522865122897358 ) ) ;
#24637 = PLANE ( 'NONE',  #55491 ) ;
#24638 = FACE_OUTER_BOUND ( 'NONE', #81648, .T. ) ;
#24639 = CYLINDRICAL_SURFACE ( 'NONE', #11506, 1.699999999999999289 ) ;
#24640 = CARTESIAN_POINT ( 'NONE',  ( -13.18904525526904692, 14.46673508071025971, 11.49999999999998934 ) ) ;
#24641 = CARTESIAN_POINT ( 'NONE',  ( -5.799455386767018439, -5.876774720514413630, 19.66076420632890276 ) ) ;
#24642 = ORIENTED_EDGE ( 'NONE', *, *, #63607, .T. ) ;
#24643 = CARTESIAN_POINT ( 'NONE',  ( 7.367719877546908158, -20.20905560389912026, -1.500000000000002220 ) ) ;
#24644 = LINE ( 'NONE', #39881, #98164 ) ;
#24645 = CARTESIAN_POINT ( 'NONE',  ( -53.01255352321339842, -1.477225279485574028, 35.59556822165056644 ) ) ;
#24646 = CARTESIAN_POINT ( 'NONE',  ( -10.34999999999999254, 4.999999999999999112, 0.000000000000000000 ) ) ;
#24647 = CARTESIAN_POINT ( 'NONE',  ( 32.19706240494739546, -5.152774720514445406, -11.87117847608345933 ) ) ;
#24648 = CARTESIAN_POINT ( 'NONE',  ( 19.50756536182865020, -12.10693203178887423, -1.500000000000002220 ) ) ;
#24649 = CC_DESIGN_PERSON_AND_ORGANIZATION_ASSIGNMENT ( #25155, #9938, ( #57026 ) ) ;
#24650 = VECTOR ( 'NONE', #100235, 1000.000000000000114 ) ;
#24651 = CALENDAR_DATE ( 2026, 9, 10 ) ;
#24652 = CARTESIAN_POINT ( 'NONE',  ( -93.62287095715007013, -23.96127896941632685, -0.6493128931037834839 ) ) ;
#24653 = CARTESIAN_POINT ( 'NONE',  ( -53.52206055214148250, -23.48783264082476663, -1.443836473390096353 ) ) ;
#24654 = CARTESIAN_POINT ( 'NONE',  ( 16.02535498940104830, 12.03463022438520191, 11.49999999999999645 ) ) ;
#24655 = LINE ( 'NONE', #77435, #91567 ) ;
#24656 = DIRECTION ( 'NONE',  ( -3.773278334453079618E-23, 0.9999999999976377785, 2.173523156925979975E-06 ) ) ;
#24657 = PLANE ( 'NONE',  #58726 ) ;
#24658 = CARTESIAN_POINT ( 'NONE',  ( -39.55620429048340014, -23.47596703998600276, 11.44779298504227505 ) ) ;
#24659 = CARTESIAN_POINT ( 'NONE',  ( -65.52287095715006160, -23.47593901973090169, -1.443836447538996870 ) ) ;
#24660 = CARTESIAN_POINT ( 'NONE',  ( 21.64095104908334122, -2.195182070091274529, 11.49999999999998934 ) ) ;
#24661 = EDGE_CURVE ( 'NONE', #21356, #47882, #28668, .T. ) ;
#24662 = CARTESIAN_POINT ( 'NONE',  ( -90.62287095715004170, -23.48786465467241058, 11.44779295918254469 ) ) ;
#24663 = CARTESIAN_POINT ( 'NONE',  ( 14.10018531369908423, 13.67006465538575277, -1.500000000000002220 ) ) ;
#24664 = CARTESIAN_POINT ( 'NONE',  ( -122.6228709571500701, -24.34917612406838572, 0.1852690917426738082 ) ) ;
#24665 = CARTESIAN_POINT ( 'NONE',  ( -40.94614453995487935, -25.19886899424074400, 3.394663469267442224 ) ) ;
#24666 = PERSON_AND_ORGANIZATION_ROLE ( 'classification_officer' ) ;
#24667 = AXIS2_PLACEMENT_3D ( 'NONE', #23147, #23655, #47015 ) ;
#24668 = DIRECTION ( 'NONE',  ( 0.000000000000000000, 0.000000000000000000, 1.000000000000000000 ) ) ;
#24669 = DIRECTION ( 'NONE',  ( -0.000000000000000000, -1.000000000000000000, -0.000000000000000000 ) ) ;
#24670 = CARTESIAN_POINT ( 'NONE',  ( -11.90445915685808131, 16.78794160864392992, 11.49999999999999645 ) ) ;
#24671 = CARTESIAN_POINT ( 'NONE',  ( -118.5228709571500758, -29.50248528299804818, 1.056150453629045360 ) ) ;
#24672 = AXIS2_PLACEMENT_3D ( 'NONE', #3490, #34429, #96325 ) ;
#24673 = CARTESIAN_POINT ( 'NONE',  ( -120.5173596569751311, -24.73486907724918638, 1.287355809206965684 ) ) ;
#24674 = CARTESIAN_POINT ( 'NONE',  ( 11.79716412695777272, 19.27136520130675024, 11.49999999999999645 ) ) ;
#24675 = ORIENTED_EDGE ( 'NONE', *, *, #76772, .T. ) ;
#24676 = CARTESIAN_POINT ( 'NONE',  ( -99.52927036222322954, -25.26387300713328443, 4.031758623024652266 ) ) ;
#24677 = CARTESIAN_POINT ( 'NONE',  ( -37.52287095715008292, -23.72747288104470087, -1.053458166803228124 ) ) ;
#24678 = CARTESIAN_POINT ( 'NONE',  ( -125.5192790873664279, -25.00182538069147498, 7.747789668545045139 ) ) ;
#24679 = DIRECTION ( 'NONE',  ( 0.000000000000000000, -1.000000000000000000, 0.000000000000000000 ) ) ;
#24680 = EDGE_CURVE ( 'NONE', #44828, #83541, #2093, .T. ) ;
#24681 = CARTESIAN_POINT ( 'NONE',  ( -26.14934357328621317, -24.93063460670250109, 7.450064799070047705 ) ) ;
#24682 = CARTESIAN_POINT ( 'NONE',  ( -28.52287095715005805, -24.49960542107631056, 8.947790409070465856 ) ) ;
#24683 = VERTEX_POINT ( 'NONE', #51944 ) ;
#24684 = AXIS2_PLACEMENT_3D ( 'NONE', #54118, #85038, #78424 ) ;
#24685 = CARTESIAN_POINT ( 'NONE',  ( -79.34687923781920915, -25.31596438058133813, 5.960409178060182889 ) ) ;
#24686 = CARTESIAN_POINT ( 'NONE',  ( -21.14637036216210575, 8.611126525438130841, 11.49999999999998934 ) ) ;
#24687 = CARTESIAN_POINT ( 'NONE',  ( 4.372949846226492632, -5.876774720514405637, 18.80635842184136308 ) ) ;
#24688 = CARTESIAN_POINT ( 'NONE',  ( -72.52287095715010423, -24.66019654487199375, 8.947790411086128159 ) ) ;
#24689 = CARTESIAN_POINT ( 'NONE',  ( -63.60363133230624300, -23.73791477778912196, 11.05961554403170766 ) ) ;
#24690 = CC_DESIGN_APPROVAL ( #82835, ( #21497 ) ) ;
#24691 = EDGE_CURVE ( 'NONE', #923, #39432, #99582, .T. ) ;
#24692 = CARTESIAN_POINT ( 'NONE',  ( -11.43049785330379997, -19.34545768653811493, 11.49999999999999645 ) ) ;
#24693 = ORIENTED_EDGE ( 'NONE', *, *, #25982, .T. ) ;
#24694 = CARTESIAN_POINT ( 'NONE',  ( -70.62287095715004170, -23.48786465467241058, 11.44779295918254469 ) ) ;
#24695 = CARTESIAN_POINT ( 'NONE',  ( -12.46176837856299002, 18.05058065364367792, 11.49999999999998934 ) ) ;
#24696 = EDGE_CURVE ( 'NONE', #84956, #87003, #83220, .T. ) ;
#24697 = LINE ( 'NONE', #64300, #78592 ) ;
#24698 = CARTESIAN_POINT ( 'NONE',  ( -110.5228709571500616, -25.00158670708909625, 2.256160236439166411 ) ) ;
#24699 = DIRECTION ( 'NONE',  ( 1.000000000000000000, 0.000000000000000000, -0.000000000000000000 ) ) ;
#24700 = AXIS2_PLACEMENT_3D ( 'NONE', #70338, #54616, #78433 ) ;
#24701 = ORIENTED_EDGE ( 'NONE', *, *, #78652, .F. ) ;
#24702 = CARTESIAN_POINT ( 'NONE',  ( -48.62369553988378357, -24.66019654487199730, 8.947790411086119278 ) ) ;
#24703 = PLANE ( 'NONE',  #68924 ) ;
#24704 = EDGE_LOOP ( 'NONE', ( #57802, #47931, #58589, #54968 ) ) ;
#24705 = CARTESIAN_POINT ( 'NONE',  ( -18.14515864413662172, 9.488524743509296755, 11.49999999999998934 ) ) ;
#24706 = ORIENTED_EDGE ( 'NONE', *, *, #6192, .F. ) ;
#24707 = ORIENTED_EDGE ( 'NONE', *, *, #100027, .T. ) ;
#24709 = EDGE_LOOP ( 'NONE', ( #57431, #30984, #49446, #64475 ) ) ;
#24708 = AXIS2_PLACEMENT_3D ( 'NONE', #96616, #43842, #26620 ) ;
#24710 = EDGE_LOOP ( 'NONE', ( #33322, #31959, #21969, #93915 ) ) ;
#24711 = CARTESIAN_POINT ( 'NONE',  ( 6.910522817300494225, 22.03692736239173300, -1.500000000000002220 ) ) ;
#24713 = ADVANCED_FACE ( 'NONE', ( #45823 ), #59564, .F. ) ;
#24712 = DIRECTION ( 'NONE',  ( -1.000000000000000000, -3.773278334444166432E-23, -8.201307841325785021E-29 ) ) ;
#24714 = CARTESIAN_POINT ( 'NONE',  ( -20.21730713243277933, 1.494317884549376974, -1.500000000000002220 ) ) ;
#24715 = VERTEX_POINT ( 'NONE', #68664 ) ;
#24716 = CARTESIAN_POINT ( 'NONE',  ( 29.70566059910618861, 3.975162330554212531, 28.10075438475601928 ) ) ;
#24717 = DIRECTION ( 'NONE',  ( -3.773278334453079030E-23, 0.9999999999976377785, 2.173523156925979128E-06 ) ) ;
#24718 = CARTESIAN_POINT ( 'NONE',  ( -8.160000000000000142, -10.65233964170348635, -1.621096496867198589 ) ) ;
#24719 = CARTESIAN_POINT ( 'NONE',  ( 4.653846153846159517, -6.376774720514415407, 19.99999999999999289 ) ) ;
#24721 = EDGE_LOOP ( 'NONE', ( #57330, #55034, #242, #66702 ) ) ;
#24720 = CARTESIAN_POINT ( 'NONE',  ( -11.48222599368078889, -18.13851731312990267, 11.49999999999999645 ) ) ;
#24722 = CARTESIAN_POINT ( 'NONE',  ( -75.59707762896087502, -24.15503026093913874, -0.2815557561904522554 ) ) ;
#24723 = CARTESIAN_POINT ( 'NONE',  ( -48.58953762381672448, -24.64898659630528144, 1.056161002820820372 ) ) ;
#24724 = EDGE_LOOP ( 'NONE', ( #23051, #10239, #17012, #71019 ) ) ;
#24725 = CARTESIAN_POINT ( 'NONE',  ( -7.464567774302189207, 19.34240081622845153, 11.49999999999998934 ) ) ;
#24726 = VERTEX_POINT ( 'NONE', #13863 ) ;
#24728 = VERTEX_POINT ( 'NONE', #90497 ) ;
#24727 = CARTESIAN_POINT ( 'NONE',  ( -125.5916854314852458, -23.48783264082478794, -1.443836473390061936 ) ) ;
#24729 = VECTOR ( 'NONE', #63100, 1000.000000000000000 ) ;
#24730 = B_SPLINE_SURFACE_WITH_KNOTS ( 'NONE', 3, 3, ( 
 ( #48390, #96062, #2723, #88949 ),
 ( #25546, #47891, #87443, #41792 ),
 ( #56012, #86939, #10320, #57015 ),
 ( #17430, #40273, #78809, #63630 ),
 ( #3235, #95559, #41275, #72229 ),
 ( #64643, #26041, #73231, #1716 ),
 ( #79325, #65636, #3723, #9819 ) ),
 .UNSPECIFIED., .F., .F., .F.,
 ( 4, 3, 4 ),
 ( 4, 4 ),
 ( 0.7945040050992240310, 0.8970133687736500105, 0.9995227324480759901 ),
 ( 0.3295777475180419747, 0.3307426270317702643 ),
 .UNSPECIFIED. ) ;
#24731 = DIRECTION ( 'NONE',  ( 0.000000000000000000, 0.000000000000000000, 1.000000000000000000 ) ) ;
#24733 = CARTESIAN_POINT ( 'NONE',  ( -117.5228709571500758, -24.65952944569305316, 1.056160979905705899 ) ) ;
#24732 = B_SPLINE_CURVE_WITH_KNOTS ( 'NONE', 3,
 ( #91385, #53842, #69564, #21862, #60957, #54344, #23360, #13755, #42, #61457, #15261, #21367, #69053, #38100 ),
 .UNSPECIFIED., .F., .F.,
 ( 4, 2, 2, 2, 2, 2, 4 ),
 ( 0.000000000000000000, 0.0004063758915776106203, 0.0008127517831552199395, 0.001015939728944024491, 0.001219127674732828608, 0.001422315620521632726, 0.001625503566310437060 ),
 .UNSPECIFIED. ) ;
#24734 = ORIENTED_EDGE ( 'NONE', *, *, #31008, .T. ) ;
#24735 = ORIENTED_EDGE ( 'NONE', *, *, #71968, .F. ) ;
#24736 = CARTESIAN_POINT ( 'NONE',  ( -6.128026245051341192, -5.876774720514410966, 19.39236848396478763 ) ) ;
#24737 = CARTESIAN_POINT ( 'NONE',  ( 22.02124265030973760, -6.376774720514428729, 19.20402280011862217 ) ) ;
#24738 = CARTESIAN_POINT ( 'NONE',  ( -66.52287095715003318, -24.66019654487199375, 8.947790411086119278 ) ) ;
#24739 = CARTESIAN_POINT ( 'NONE',  ( -21.82725030464235516, 2.967780500094957308, 11.49999999999999645 ) ) ;
#24740 = CARTESIAN_POINT ( 'NONE',  ( -43.52287095715006160, -29.50247984919015209, -1.443849546365060466 ) ) ;
#24741 = CARTESIAN_POINT ( 'NONE',  ( -4.885077187424587741, 22.05487924249641551, 11.49999999999998934 ) ) ;
#24742 = CARTESIAN_POINT ( 'NONE',  ( 19.96068868648078620, -6.529529906025321573, -1.500000000000002220 ) ) ;
#24744 = ORIENTED_EDGE ( 'NONE', *, *, #48984, .F. ) ;
#24743 = CARTESIAN_POINT ( 'NONE',  ( -62.52287095715007581, -23.72747288104470087, -1.053458166803227458 ) ) ;
#24745 = VECTOR ( 'NONE', #29278, 1000.000000000000000 ) ;
#24746 = ORIENTED_EDGE ( 'NONE', *, *, #71363, .F. ) ;
#24747 = CARTESIAN_POINT ( 'NONE',  ( -80.62287095715008434, -24.82558206586145033, 1.605769216559443491 ) ) ;
#24748 = EDGE_CURVE ( 'NONE', #6143, #94577, #68558, .T. ) ;
#24749 = DIRECTION ( 'NONE',  ( 0.000000000000000000, 0.000000000000000000, -1.000000000000000000 ) ) ;
#24750 = ORIENTED_EDGE ( 'NONE', *, *, #88393, .T. ) ;
#24751 = CARTESIAN_POINT ( 'NONE',  ( 1.363997202867437863, 21.09336101032836908, -1.500000000000002220 ) ) ;
#24752 = DIRECTION ( 'NONE',  ( -0.000000000000000000, 1.000000000000000000, -0.000000000000000000 ) ) ;
#24753 = CARTESIAN_POINT ( 'NONE',  ( -51.93023907722363219, -25.26040824531888518, 6.217084455637032825 ) ) ;
#24754 = CARTESIAN_POINT ( 'NONE',  ( -121.5573556918825204, -23.48783264082477373, -1.443836473390087916 ) ) ;
#24755 = CARTESIAN_POINT ( 'NONE',  ( -118.5895376238167245, -23.47593901973091235, -1.443836447538997536 ) ) ;
#24756 = DIRECTION ( 'NONE',  ( 1.000000000000000000, 0.000000000000000000, 0.000000000000000000 ) ) ;
#24757 = CARTESIAN_POINT ( 'NONE',  ( 10.53326394202159300, -19.55463526559320542, -1.500000000000002220 ) ) ;
#24758 = CARTESIAN_POINT ( 'NONE',  ( 27.53860345374808105, 3.356774720514427379, 1.647607965253217621 ) ) ;
#24759 = ORIENTED_EDGE ( 'NONE', *, *, #99948, .F. ) ;
#24760 = DIRECTION ( 'NONE',  ( -0.000000000000000000, -0.000000000000000000, -1.000000000000000000 ) ) ;
#24761 = CARTESIAN_POINT ( 'NONE',  ( -37.49782949886290595, -24.15543982623907127, -0.2315651400026566831 ) ) ;
#24762 = CARTESIAN_POINT ( 'NONE',  ( -126.5549976813165642, -24.51314013834316086, 0.6176544820404181735 ) ) ;
#24763 = CARTESIAN_POINT ( 'NONE',  ( -41.86995616089613748, -25.27977532709532227, 4.210709737483026238 ) ) ;
#24764 = DIRECTION ( 'NONE',  ( 0.000000000000000000, -1.000000000000000000, 0.000000000000000000 ) ) ;
#24765 = AXIS2_PLACEMENT_3D ( 'NONE', #90687, #29286, #52133 ) ;
#24766 = CARTESIAN_POINT ( 'NONE',  ( 19.32586673001642197, -2.567307930040524599, 11.49999999999998934 ) ) ;
#24767 = EDGE_LOOP ( 'NONE', ( #17863, #99022, #85165, #71693 ) ) ;
#24768 = CARTESIAN_POINT ( 'NONE',  ( -9.924231251898440576, -18.97836718215353713, -1.500000000000002220 ) ) ;
#24769 = DIRECTION ( 'NONE',  ( -3.773278334444166432E-23, 1.000000000000000000, 0.000000000000000000 ) ) ;
#24770 = CARTESIAN_POINT ( 'NONE',  ( -60.64669611341108890, -24.15602025861359792, 10.28564288302606045 ) ) ;
#24771 = CARTESIAN_POINT ( 'NONE',  ( -51.63318508066054591, -24.34968618360933590, 0.1864209137778788938 ) ) ;
#24772 = CARTESIAN_POINT ( 'NONE',  ( -38.52287095715006870, -24.65952944569303895, 1.056160979905691910 ) ) ;
#24773 = CARTESIAN_POINT ( 'NONE',  ( -22.70586268970451371, -1.818501321912391999, -1.500000000000002220 ) ) ;
#24774 = EDGE_CURVE ( 'NONE', #27638, #35495, #57809, .T. ) ;
#24775 = VECTOR ( 'NONE', #61260, 1000.000000000000114 ) ;
#24776 = LINE ( 'NONE', #24289, #61305 ) ;
#24777 = LINE ( 'NONE', #953, #46011 ) ;
#24778 = CARTESIAN_POINT ( 'NONE',  ( 6.283368587668265448, -18.83516890145298106, 11.49999999999999645 ) ) ;
#24779 = CARTESIAN_POINT ( 'NONE',  ( -123.5918566822411009, -23.48786465467241769, 11.44779295918253759 ) ) ;
#24780 = EDGE_CURVE ( 'NONE', #82889, #18993, #28598, .T. ) ;
#24781 = AXIS2_PLACEMENT_3D ( 'NONE', #29876, #98884, #45120 ) ;
#24782 = CARTESIAN_POINT ( 'NONE',  ( -89.81226385320384509, -25.12770589570459379, 7.104042815775061470 ) ) ;
#24783 = LINE ( 'NONE', #25793, #44024 ) ;
#24784 = ORIENTED_EDGE ( 'NONE', *, *, #1923, .T. ) ;
#24785 = CARTESIAN_POINT ( 'NONE',  ( 0.9317375178030620209, -7.299023693294228288, -9.000000000000000000 ) ) ;
#24786 = CARTESIAN_POINT ( 'NONE',  ( -6.487934372591614540, -6.376774720514411854, 19.49432735726520605 ) ) ;
#24787 = CARTESIAN_POINT ( 'NONE',  ( -51.43440959051734751, -25.10935856805285482, 3.290885709867275910 ) ) ;
#24788 = CARTESIAN_POINT ( 'NONE',  ( -14.64807036877012258, -15.96857234361563904, -1.500000000000002220 ) ) ;
#24789 = ADVANCED_FACE ( 'NONE', ( #45333 ), #51583, .T. ) ;
#24790 = CARTESIAN_POINT ( 'NONE',  ( -29.62287095715005947, -24.26261939641257825, 9.819270444555529664 ) ) ;
#24791 = CARTESIAN_POINT ( 'NONE',  ( -1.849579639615634097, -19.42000222497389927, -1.500000000000002220 ) ) ;
#24792 = ADVANCED_FACE ( 'NONE', ( #55948 ), #2165, .T. ) ;
#24793 = CARTESIAN_POINT ( 'NONE',  ( -55.52645046534955497, -25.00182538069146787, 7.747789668545041586 ) ) ;
#24794 = ORIENTED_EDGE ( 'NONE', *, *, #59283, .T. ) ;
#24795 = ADVANCED_FACE ( 'NONE', ( #40211 ), #66157, .T. ) ;
#24796 = CARTESIAN_POINT ( 'NONE',  ( 13.37706023731332827, -15.40713922116925616, 11.49999999999999645 ) ) ;
#24797 = CARTESIAN_POINT ( 'NONE',  ( -29.49875734969025842, 0.3587747205144265483, 25.61802280011862720 ) ) ;
#24798 = PLANE ( 'NONE',  #14010 ) ;
#24799 = ORIENTED_EDGE ( 'NONE', *, *, #69853, .F. ) ;
#24800 = CARTESIAN_POINT ( 'NONE',  ( -30.63208233338744080, -23.87624887660337691, 11.01174216662000127 ) ) ;
#24801 = CARTESIAN_POINT ( 'NONE',  ( 33.41263754283357912, 3.496799131921995762, -12.47286811689047070 ) ) ;
#24802 = CARTESIAN_POINT ( 'NONE',  ( -39.04454818115137016, -25.31628458813839444, 4.262458856014446518 ) ) ;
#24803 = LINE ( 'NONE', #17196, #86249 ) ;
#24804 = DIRECTION ( 'NONE',  ( -1.000000000000000000, -3.491481338843133355E-15, -2.352173255807796056E-16 ) ) ;
#24805 = CARTESIAN_POINT ( 'NONE',  ( 4.282148337517553749, -19.64591042314588165, -1.500000000000002220 ) ) ;
#24806 = EDGE_CURVE ( 'NONE', #46271, #22334, #60136, .T. ) ;
#24807 = CARTESIAN_POINT ( 'NONE',  ( -57.58953762381672448, -23.47593901973091235, -1.443836447539007972 ) ) ;
#24808 = VECTOR ( 'NONE', #15359, 1000.000000000000000 ) ;
#24809 = ORIENTED_EDGE ( 'NONE', *, *, #54540, .F. ) ;
#24810 = CARTESIAN_POINT ( 'NONE',  ( 32.53135143123563466, -0.3587747205144265483, 6.926385399448451885 ) ) ;
#24811 = CARTESIAN_POINT ( 'NONE',  ( 15.56936346670522120, 16.85858822313069894, 11.49999999999999645 ) ) ;
#24812 = CARTESIAN_POINT ( 'NONE',  ( 7.533951754900199305, 21.46025436219600024, -1.500000000000002220 ) ) ;
#24813 = ORIENTED_EDGE ( 'NONE', *, *, #6075, .F. ) ;
#24814 = CARTESIAN_POINT ( 'NONE',  ( -31.55620429048339304, -23.47596703998600276, 11.44779298504227505 ) ) ;
#24815 = VECTOR ( 'NONE', #23535, 1000.000000000000000 ) ;
#24816 = DIRECTION ( 'NONE',  ( -1.000000000000000000, -0.000000000000000000, -0.000000000000000000 ) ) ;
#24817 = CARTESIAN_POINT ( 'NONE',  ( -90.59125879922106606, -24.40034930558990922, 0.3402023900116054045 ) ) ;
#24818 = PLANE ( 'NONE',  #7625 ) ;
#24819 = EDGE_CURVE ( 'NONE', #58107, #9739, #85371, .T. ) ;
#24820 = B_SPLINE_CURVE_WITH_KNOTS ( 'NONE', 3,
 ( #40920, #95706, #18080, #72380, #25691, #49048 ),
 .UNSPECIFIED., .F., .F.,
 ( 4, 2, 4 ),
 ( 0.000000000000000000, 0.001380764517853247516, 0.002761529035706495033 ),
 .UNSPECIFIED. ) ;
#24821 = DIRECTION ( 'NONE',  ( -0.2488812114211667037, -0.000000000000000000, -0.9685340172660599212 ) ) ;
#24822 = EDGE_CURVE ( 'NONE', #80762, #15342, #27417, .T. ) ;
#24823 = CARTESIAN_POINT ( 'NONE',  ( -115.6228709571500417, -24.63287334234178516, 0.9662140553045511782 ) ) ;
#24824 = CARTESIAN_POINT ( 'NONE',  ( -54.52287095715009002, -24.33832256527048088, 0.1851278514138564868 ) ) ;
#24825 = CARTESIAN_POINT ( 'NONE',  ( -81.52287095715010423, -23.47593901973090524, -1.443836447538996648 ) ) ;
#24826 = ORIENTED_EDGE ( 'NONE', *, *, #12424, .F. ) ;
#24827 = CARTESIAN_POINT ( 'NONE',  ( 13.37706023731332827, -15.40713922116925616, -1.500000000000002220 ) ) ;
#24828 = VERTEX_POINT ( 'NONE', #47827 ) ;
#24829 = B_SPLINE_CURVE_WITH_KNOTS ( 'NONE', 3,
 ( #32696, #31703, #30702, #46931 ),
 .UNSPECIFIED., .F., .F.,
 ( 4, 4 ),
 ( 0.000000000000000000, 9.999999999998897304E-05 ),
 .UNSPECIFIED. ) ;
#24830 = CARTESIAN_POINT ( 'NONE',  ( -22.77861398648627400, -3.026084143414268013, 11.49999999999998934 ) ) ;
#24832 = EDGE_CURVE ( 'NONE', #18101, #87003, #37224, .T. ) ;
#24831 = CARTESIAN_POINT ( 'NONE',  ( -7.064692883725313344, -5.876774720514411854, 19.55266968305501862 ) ) ;
#24833 = ORIENTED_EDGE ( 'NONE', *, *, #69873, .F. ) ;
#24834 = CARTESIAN_POINT ( 'NONE',  ( -12.84880425037202656, -0.3587747205143964613, -26.59900746623529244 ) ) ;
#24835 = DIRECTION ( 'NONE',  ( 1.000000000000000000, 0.000000000000000000, 0.000000000000000000 ) ) ;
#24836 = EDGE_CURVE ( 'NONE', #48449, #67264, #9756, .T. ) ;
#24837 = CIRCLE ( 'NONE', #68593, 18.50000000000000000 ) ;
#24838 = ADVANCED_FACE ( 'NONE', ( #12240 ), #58451, .T. ) ;
#24839 = CARTESIAN_POINT ( 'NONE',  ( -29.62287095715004881, -24.58390616985635546, 1.056161279468100123 ) ) ;
#24841 = VERTEX_POINT ( 'NONE', #97491 ) ;
#24840 = CARTESIAN_POINT ( 'NONE',  ( -20.61954105445765251, -5.431428859615135885, 11.49999999999999645 ) ) ;
#24842 = ORIENTED_EDGE ( 'NONE', *, *, #71929, .F. ) ;
#24843 = CARTESIAN_POINT ( 'NONE',  ( -4.073883676365832152, 21.86232641878667593, 11.49999999999998934 ) ) ;
#24844 = CARTESIAN_POINT ( 'NONE',  ( 10.61356161029474521, 17.70173163822984819, -1.500000000000002220 ) ) ;
#24846 = ORIENTED_EDGE ( 'NONE', *, *, #30956, .F. ) ;
#24845 = VECTOR ( 'NONE', #18064, 1000.000000000000000 ) ;
#24847 = CARTESIAN_POINT ( 'NONE',  ( 0.2196812790064107401, -6.376774720514408301, 19.42522865122897002 ) ) ;
#24848 = CARTESIAN_POINT ( 'NONE',  ( -95.54582827825265667, -24.73531770709095312, 8.716586749053508498 ) ) ;
#24849 = VERTEX_POINT ( 'NONE', #41729 ) ;
#24850 = DIRECTION ( 'NONE',  ( 0.000000000000000000, 2.173523156925980399E-06, -0.9999999999976378895 ) ) ;
#24851 = VERTEX_POINT ( 'NONE', #74160 ) ;
#24852 = VECTOR ( 'NONE', #95913, 1000.000000000000114 ) ;
#24853 = CARTESIAN_POINT ( 'NONE',  ( -129.5895376238167387, -24.65952944569305316, 1.056160979905705011 ) ) ;
#24854 = DIRECTION ( 'NONE',  ( 1.000000000000000000, 0.000000000000000000, 0.000000000000000000 ) ) ;
#24855 = CARTESIAN_POINT ( 'NONE',  ( 13.94627346685978075, -15.57361473980792255, -1.500000000000002220 ) ) ;
#24856 = CARTESIAN_POINT ( 'NONE',  ( -18.37375256118794553, 11.78967355450649457, 11.49999999999999645 ) ) ;
#24857 = CARTESIAN_POINT ( 'NONE',  ( -27.07602811445854130, -24.77993765707372376, 7.457967602658744255 ) ) ;
#24858 = CARTESIAN_POINT ( 'NONE',  ( -91.62287095715004170, -29.50248528299804818, 1.056150453629040253 ) ) ;
#24859 = CARTESIAN_POINT ( 'NONE',  ( 22.08653571170524543, -4.319401766784854324, 11.49999999999998934 ) ) ;
#24860 = CARTESIAN_POINT ( 'NONE',  ( -50.38822539166533687, -25.31296765081191680, 4.736250530724597674 ) ) ;
#24861 = CARTESIAN_POINT ( 'NONE',  ( 10.34999999999998010, 22.00000000000000000, 2.100000000000000089 ) ) ;
#24862 = DIRECTION ( 'NONE',  ( -0.7512896232465891000, 0.000000000000000000, -0.6599726524652352877 ) ) ;
#24863 = VERTEX_POINT ( 'NONE', #79763 ) ;
#24864 = ORIENTED_EDGE ( 'NONE', *, *, #58968, .T. ) ;
#24865 = VERTEX_POINT ( 'NONE', #80779 ) ;
#24866 = CARTESIAN_POINT ( 'NONE',  ( -29.49875734969026198, 0.3587747205144265483, 2.362022800118626531 ) ) ;
#24867 = ORIENTED_EDGE ( 'NONE', *, *, #87362, .F. ) ;
#24868 = CARTESIAN_POINT ( 'NONE',  ( -5.333777546869826303, -20.73983961313815172, -1.500000000000002220 ) ) ;
#24869 = CARTESIAN_POINT ( 'NONE',  ( 13.15158565771796084, -18.08388448789661851, 11.49999999999999645 ) ) ;
#24870 = VERTEX_POINT ( 'NONE', #34606 ) ;
#24871 = CARTESIAN_POINT ( 'NONE',  ( 32.76524810979199742, -3.299944812882172229, -3.892744026461423701 ) ) ;
#24872 = CARTESIAN_POINT ( 'NONE',  ( -16.48755246578841849, -13.11705038010048163, 11.49999999999998934 ) ) ;
#24873 = CARTESIAN_POINT ( 'NONE',  ( -30.50821306534034250, -24.04899441997164189, 10.47557002954947336 ) ) ;
#24874 = CARTESIAN_POINT ( 'NONE',  ( -17.57349146297605103, 9.389787994052484876, -1.500000000000002220 ) ) ;
#24875 = FACE_OUTER_BOUND ( 'NONE', #24957, .T. ) ;
#24876 = CARTESIAN_POINT ( 'NONE',  ( 3.036358173076929123, -6.376774720514420736, 20.87990785256409865 ) ) ;
#24877 = CARTESIAN_POINT ( 'NONE',  ( -18.24146354680218707, 12.35505607031776165, -1.500000000000002220 ) ) ;
#24878 = CARTESIAN_POINT ( 'NONE',  ( -83.52287095715009002, -23.94994826722565406, -0.6494450866342720285 ) ) ;
#24879 = ORIENTED_EDGE ( 'NONE', *, *, #76220, .F. ) ;
#24880 = CARTESIAN_POINT ( 'NONE',  ( -65.58377276114705978, -24.73531770709095312, 8.716586749053508498 ) ) ;
#24881 = CIRCLE ( 'NONE', #78323, 129.7684398600581517 ) ;
#24882 = PLANE ( 'NONE',  #43267 ) ;
#24883 = CARTESIAN_POINT ( 'NONE',  ( -1.025521031027718299, 20.81036885881322362, 11.49999999999999645 ) ) ;
#24884 = CARTESIAN_POINT ( 'NONE',  ( -74.62287095715005592, -24.65952944569304606, 1.056160979905696351 ) ) ;
#24885 = VECTOR ( 'NONE', #68884, 1000.000000000000000 ) ;
#24886 = CARTESIAN_POINT ( 'NONE',  ( -129.5228709571500758, -23.47596703998600631, 11.44779298504227683 ) ) ;
#24887 = LINE ( 'NONE', #25394, #88592 ) ;
#24888 = CARTESIAN_POINT ( 'NONE',  ( -11.06822068739258391, -18.21809710261049275, 11.49999999999998934 ) ) ;
#24889 = CARTESIAN_POINT ( 'NONE',  ( 0.5999240985075944277, 1.411520799013914917, -8.999999999999998224 ) ) ;
#24890 = CARTESIAN_POINT ( 'NONE',  ( -41.26959558397305727, -29.50249893827660941, 7.338705366995167623 ) ) ;
#24891 = CARTESIAN_POINT ( 'NONE',  ( -92.52287095715006160, -23.47593901973090169, -1.443836447538996426 ) ) ;
#24892 = LINE ( 'NONE', #94909, #55663 ) ;
#24893 = CARTESIAN_POINT ( 'NONE',  ( 22.48569338394020534, -0.9006126209707296937, -1.500000000000002220 ) ) ;
#24894 = EDGE_CURVE ( 'NONE', #15218, #98626, #57955, .T. ) ;
#24895 = CARTESIAN_POINT ( 'NONE',  ( -83.55620429048340725, -24.66019654487199730, 8.947790411086126383 ) ) ;
#24896 = ORIENTED_EDGE ( 'NONE', *, *, #65886, .F. ) ;
#24897 = EDGE_CURVE ( 'NONE', #80644, #33824, #81270, .T. ) ;
#24898 = CARTESIAN_POINT ( 'NONE',  ( -119.5228709571500616, -24.66019654487200441, 8.947790411086108620 ) ) ;
#24899 = CARTESIAN_POINT ( 'NONE',  ( -31.47681414363396613, -24.66019654487199020, 8.947790411086133489 ) ) ;
#24900 = CARTESIAN_POINT ( 'NONE',  ( 11.88433821776028942, -15.71472908967258242, 11.49999999999999645 ) ) ;
#24901 = DIRECTION ( 'NONE',  ( -4.089440751051245812E-15, -1.000000000000000000, 1.042451643221144600E-15 ) ) ;
#24902 = PLANE ( 'NONE',  #65841 ) ;
#24903 = ORIENTED_EDGE ( 'NONE', *, *, #94745, .F. ) ;
#24904 = CARTESIAN_POINT ( 'NONE',  ( -99.63465086565865647, -23.73766607897671577, -1.055555164236429144 ) ) ;
#24905 = DIRECTION ( 'NONE',  ( 0.000000000000000000, 0.000000000000000000, 1.000000000000000000 ) ) ;
#24906 = CARTESIAN_POINT ( 'NONE',  ( -124.5904482984883970, -23.96169478059714564, 10.65365249895717170 ) ) ;
#24907 = EDGE_CURVE ( 'NONE', #87025, #55690, #19856, .T. ) ;
#24908 = FACE_OUTER_BOUND ( 'NONE', #81436, .T. ) ;
#24909 = EDGE_CURVE ( 'NONE', #1499, #87928, #25415, .T. ) ;
#24910 = FACE_OUTER_BOUND ( 'NONE', #59213, .T. ) ;
#24911 = CARTESIAN_POINT ( 'NONE',  ( -9.637476322613308000, -17.25261889746210997, -1.500000000000002220 ) ) ;
#24912 = ORIENTED_EDGE ( 'NONE', *, *, #67671, .T. ) ;
#24913 = EDGE_CURVE ( 'NONE', #30912, #2401, #33598, .T. ) ;
#24914 = CARTESIAN_POINT ( 'NONE',  ( -14.69473627950705108, 13.90061564059656440, 11.49999999999999645 ) ) ;
#24915 = CARTESIAN_POINT ( 'NONE',  ( 6.431189903846153300, -5.876774720514424288, 20.08974358974358765 ) ) ;
#24916 = VECTOR ( 'NONE', #39627, 1000.000000000000000 ) ;
#24917 = ORIENTED_EDGE ( 'NONE', *, *, #39092, .T. ) ;
#24918 = CARTESIAN_POINT ( 'NONE',  ( -48.62287095715004881, -23.47596703998600276, 11.44779298504227505 ) ) ;
#24919 = CARTESIAN_POINT ( 'NONE',  ( 26.73860345374794178, -1.477225279485574028, 19.84760796525321780 ) ) ;
#24920 = CARTESIAN_POINT ( 'NONE',  ( -51.52764846858840997, -25.24768739062223943, 6.187572788000800017 ) ) ;
#24921 = CARTESIAN_POINT ( 'NONE',  ( 10.86264264036872440, -0.3587747205144257157, -28.05717073575603138 ) ) ;
#24922 = LINE ( 'NONE', #23921, #44102 ) ;
#24923 = AXIS2_PLACEMENT_3D ( 'NONE', #3955, #2964, #33896 ) ;
#24924 = CARTESIAN_POINT ( 'NONE',  ( 19.72776355195876263, 5.965225279485572685, 28.39950002376592764 ) ) ;
#24925 = CARTESIAN_POINT ( 'NONE',  ( -1.591348192139008466, -19.94584644712825039, 11.49999999999998934 ) ) ;
#24926 = EDGE_CURVE ( 'NONE', #153, #96640, #50525, .T. ) ;
#24927 = CARTESIAN_POINT ( 'NONE',  ( -99.92788026055190187, -25.27532880725036790, 2.920407968822682054 ) ) ;
#24928 = CARTESIAN_POINT ( 'NONE',  ( -116.5185765065318861, -24.15620529776628800, 10.23563542870659759 ) ) ;
#24929 = ORIENTED_EDGE ( 'NONE', *, *, #60458, .F. ) ;
#24930 = EDGE_CURVE ( 'NONE', #10530, #23209, #77244, .T. ) ;
#24931 = CARTESIAN_POINT ( 'NONE',  ( -79.62361068839391010, -24.66019654487199375, 8.947790411086119278 ) ) ;
#24932 = CARTESIAN_POINT ( 'NONE',  ( -109.9559143002945234, -25.18430168171479266, 3.359997616863110270 ) ) ;
#24933 = CARTESIAN_POINT ( 'NONE',  ( -35.58884038832008656, -24.52300882791529446, 0.6510814631126419227 ) ) ;
#24934 = CARTESIAN_POINT ( 'NONE',  ( -100.5895376238167245, -23.48786465467241769, 11.44779295918254114 ) ) ;
#24935 = CARTESIAN_POINT ( 'NONE',  ( -116.7735373858569119, -25.37153787860454202, 4.078969152973338730 ) ) ;
#24936 = CARTESIAN_POINT ( 'NONE',  ( 0.7051282051282027341, -6.376774720514408301, 19.19230769230768985 ) ) ;
#24937 = EDGE_CURVE ( 'NONE', #47723, #5782, #54607, .T. ) ;
#24938 = CARTESIAN_POINT ( 'NONE',  ( -27.15721599100127648, 0.3587747205144061757, -10.22292133548836723 ) ) ;
#24939 = CARTESIAN_POINT ( 'NONE',  ( -49.62090859027108536, -25.22926554657857423, 3.641651233274940669 ) ) ;
#24940 = ORIENTED_EDGE ( 'NONE', *, *, #32289, .F. ) ;
#24941 = CARTESIAN_POINT ( 'NONE',  ( 16.59675031405745571, -11.69241480613374407, 11.49999999999998934 ) ) ;
#24942 = DIRECTION ( 'NONE',  ( -1.000000000000000000, 0.000000000000000000, 0.000000000000000000 ) ) ;
#24943 = AXIS2_PLACEMENT_3D ( 'NONE', #74134, #3632, #57929 ) ;
#24944 = CARTESIAN_POINT ( 'NONE',  ( -34.62918016310124614, -24.51314013834315375, 0.6176544820404091807 ) ) ;
#24945 = CARTESIAN_POINT ( 'NONE',  ( -105.6228709571500559, -23.48783264082479150, -1.443836473390060160 ) ) ;
#24947 = ORIENTED_EDGE ( 'NONE', *, *, #72984, .T. ) ;
#24946 = EDGE_CURVE ( 'NONE', #67290, #18359, #27985, .T. ) ;
#24948 = FACE_OUTER_BOUND ( 'NONE', #82882, .T. ) ;
#24949 = CARTESIAN_POINT ( 'NONE',  ( -9.895454706725905325, 17.58729670687104729, -1.500000000000002220 ) ) ;
#24950 = B_SPLINE_CURVE_WITH_KNOTS ( 'NONE', 3,
 ( #26480, #87873, #80258, #49831, #42222, #83744, #15235, #60436, #36571, #67541, #21834, #75621, #98461, #29961, #44202, #82744, #91359, #14225, #6626, #53814, #69535, #60930, #76128, #13228, #68531, #84747, #46192 ),
 .UNSPECIFIED., .F., .F.,
 ( 4, 1, 1, 1, 1, 1, 1, 1, 1, 1, 1, 1, 1, 1, 1, 1, 1, 1, 1, 1, 1, 1, 1, 1, 4 ),
 ( 0.000000000000000000, 0.06506328961727787796, 0.1267731664665228408, 0.1855157632260783507, 0.2407646791677146292, 0.2929797960235977494, 0.3422503727797667206, 0.3889192861856601846, 0.4327756640583091396, 0.4746284326311175361, 0.5147746906379525589, 0.5536058934984424695, 0.5914264064311723912, 0.6280281199460664432, 0.6638036341103201732, 0.6989843361316636638, 0.7335914893067054798, 0.7676284691511399139, 0.8012083477865917791, 0.8342638397266231021, 0.8669806947287760357, 0.8997197415181603652, 0.9327019124985379550, 0.9661758834327495160, 1.000000000000000000 ),
 .UNSPECIFIED. ) ;
#24951 = VECTOR ( 'NONE', #32071, 1000.000000000000114 ) ;
#24952 = CARTESIAN_POINT ( 'NONE',  ( -3.044128750896296420, -20.94304649679510888, 11.49999999999999645 ) ) ;
#24953 = CARTESIAN_POINT ( 'NONE',  ( 17.03105324785762420, 14.15717209551829647, -1.500000000000002220 ) ) ;
#24954 = ADVANCED_FACE ( 'NONE', ( #18868 ), #49341, .F. ) ;
#24955 = CARTESIAN_POINT ( 'NONE',  ( -20.44794078217315558, 2.270689272194197805, 11.49999999999998934 ) ) ;
#24956 = LINE ( 'NONE', #55930, #41973 ) ;
#24957 = EDGE_LOOP ( 'NONE', ( #80030, #2189, #95079, #10732 ) ) ;
#24958 = CARTESIAN_POINT ( 'NONE',  ( -88.55620429048339304, -23.47596703998600631, 11.44779298504227683 ) ) ;
#24959 = VERTEX_POINT ( 'NONE', #58942 ) ;
#24960 = CARTESIAN_POINT ( 'NONE',  ( -54.51466552200992055, -23.73766607897669800, -1.055555164236461785 ) ) ;
#24961 = DIRECTION ( 'NONE',  ( -3.773278334453079030E-23, 0.9999999999976377785, 2.173523156925979128E-06 ) ) ;
#24962 = ORIENTED_EDGE ( 'NONE', *, *, #3422, .F. ) ;
#24963 = ORIENTED_EDGE ( 'NONE', *, *, #57246, .T. ) ;
#24964 = VERTEX_POINT ( 'NONE', #3660 ) ;
#24965 = CARTESIAN_POINT ( 'NONE',  ( -112.6228709571500417, -24.65952944569304961, 1.056160979905702346 ) ) ;
#24966 = CARTESIAN_POINT ( 'NONE',  ( -105.6228709571500275, -25.00158670708909625, 2.256160236439166411 ) ) ;
#24967 = CARTESIAN_POINT ( 'NONE',  ( -12.84880425037203011, 5.965225279485592225, -26.59900746623528534 ) ) ;
#24968 = CARTESIAN_POINT ( 'NONE',  ( -19.40401905104624802, 7.283777608679691262, -1.500000000000002220 ) ) ;
#24969 = CARTESIAN_POINT ( 'NONE',  ( 17.85095790706337127, 12.24325521369631176, 11.49999999999999645 ) ) ;
#24970 = ORIENTED_EDGE ( 'NONE', *, *, #83089, .F. ) ;
#24971 = FACE_OUTER_BOUND ( 'NONE', #42860, .T. ) ;
#24972 = LINE ( 'NONE', #48835, #61022 ) ;
#24973 = CARTESIAN_POINT ( 'NONE',  ( 6.968497804723354783, -21.30229754059623559, 11.49999999999998934 ) ) ;
#24974 = CARTESIAN_POINT ( 'NONE',  ( -47.61502911968744201, -23.48786465467240347, 11.44779295918255002 ) ) ;
#24975 = CARTESIAN_POINT ( 'NONE',  ( -53.52287095715006870, -24.64898659630367916, 1.056161002820821038 ) ) ;
#24976 = ORIENTED_EDGE ( 'NONE', *, *, #32284, .T. ) ;
#24977 = FACE_OUTER_BOUND ( 'NONE', #50314, .T. ) ;
#24978 = CARTESIAN_POINT ( 'NONE',  ( -120.6228709571500843, -24.15516710230294706, 10.28746687063725851 ) ) ;
#24979 = ORIENTED_EDGE ( 'NONE', *, *, #100274, .T. ) ;
#24980 = ORIENTED_EDGE ( 'NONE', *, *, #78848, .T. ) ;
#24981 = FACE_OUTER_BOUND ( 'NONE', #68414, .T. ) ;
#24982 = VERTEX_POINT ( 'NONE', #73660 ) ;
#24983 = B_SPLINE_CURVE_WITH_KNOTS ( 'NONE', 3,
 ( #40846, #24116, #48974, #2805 ),
 .UNSPECIFIED., .F., .F.,
 ( 4, 4 ),
 ( 1.387778780781445676E-17, 9.999999999999593903E-05 ),
 .UNSPECIFIED. ) ;
#24984 = CARTESIAN_POINT ( 'NONE',  ( -129.6228709571500417, -24.64965695001463430, 8.947790411086117501 ) ) ;
#24985 = CARTESIAN_POINT ( 'NONE',  ( 10.81949470224598997, -18.29866561848832518, -1.500000000000002220 ) ) ;
#24986 = EDGE_LOOP ( 'NONE', ( #73411, #37208, #40948, #18589 ) ) ;
#24987 = CARTESIAN_POINT ( 'NONE',  ( -50.63517956937771203, -24.63355581998386157, 0.9682620441943928791 ) ) ;
#24988 = CARTESIAN_POINT ( 'NONE',  ( 12.66963027563507005, -17.75133666976559255, -1.500000000000002220 ) ) ;
#24989 = CARTESIAN_POINT ( 'NONE',  ( -52.62809792546378418, -24.51419770103158413, 9.386484678747189392 ) ) ;
#24990 = CARTESIAN_POINT ( 'NONE',  ( 7.176111537430461595, -6.376774720514424288, 21.53668079471899333 ) ) ;
#24991 = CARTESIAN_POINT ( 'NONE',  ( 6.156881756163101294, -5.876774720514414518, 19.74809127057764968 ) ) ;
#24992 = CARTESIAN_POINT ( 'NONE',  ( -6.542779104410481494, 20.88585256366161502, -1.500000000000002220 ) ) ;
#24993 = CARTESIAN_POINT ( 'NONE',  ( -30.57287095715006231, -24.66858702400017123, 1.114042296326039017 ) ) ;
#24994 = ORIENTED_EDGE ( 'NONE', *, *, #14736, .T. ) ;
#24995 = CARTESIAN_POINT ( 'NONE',  ( -30.49303573129054357, -23.47596703998576118, 11.44779287168131710 ) ) ;
#24996 = B_SPLINE_CURVE_WITH_KNOTS ( 'NONE', 3,
 ( #26315, #27807, #19187, #33928 ),
 .UNSPECIFIED., .F., .F.,
 ( 4, 4 ),
 ( 0.000000000000000000, 9.999999999999592548E-05 ),
 .UNSPECIFIED. ) ;
#24997 = LINE ( 'NONE', #79285, #65412 ) ;
#24998 = VERTEX_POINT ( 'NONE', #3168 ) ;
#24999 = ORIENTED_EDGE ( 'NONE', *, *, #10549, .F. ) ;
#25000 = ORIENTED_EDGE ( 'NONE', *, *, #76619, .F. ) ;
#25001 = PLANE ( 'NONE',  #63771 ) ;
#25002 = CARTESIAN_POINT ( 'NONE',  ( -82.58247902686774466, -24.65952944569304606, 1.056160979905702790 ) ) ;
#25003 = B_SPLINE_CURVE_WITH_KNOTS ( 'NONE', 3,
 ( #74458, #42534, #49152, #49643, #73468, #65383 ),
 .UNSPECIFIED., .F., .F.,
 ( 4, 2, 4 ),
 ( 1.570887131794176733E-05, 0.001396322306279756519, 0.002776935741241571502 ),
 .UNSPECIFIED. ) ;
#25004 = CARTESIAN_POINT ( 'NONE',  ( -3.247986963444697395, 20.98610878802851332, -1.500000000000002220 ) ) ;
#25005 = CARTESIAN_POINT ( 'NONE',  ( 10.46399479596398052, 3.316774720514422903, -27.03001098546561209 ) ) ;
#25006 = LINE ( 'NONE', #90911, #83756 ) ;
#25007 = AXIS2_PLACEMENT_3D ( 'NONE', #21792, #46156, #30419 ) ;
#25008 = FACE_OUTER_BOUND ( 'NONE', #28917, .T. ) ;
#25009 = B_SPLINE_CURVE_WITH_KNOTS ( 'NONE', 3,
 ( #68407, #59808, #99340, #45079, #99825, #90242, #92231, #22703, #52184, #20717, #90742, #6000, #28844, #29837, #67920, #21708 ),
 .UNSPECIFIED., .F., .F.,
 ( 4, 2, 2, 2, 2, 2, 2, 4 ),
 ( 0.000000000000000000, 0.0002659278985097128707, 0.0005318557970194257413, 0.0007977836955291387746, 0.001063711594038851483, 0.001595567391058279067, 0.001861495289568003376, 0.002127423188077727251 ),
 .UNSPECIFIED. ) ;
#25010 = PLANE ( 'NONE',  #26535 ) ;
#25011 = CARTESIAN_POINT ( 'NONE',  ( -5.977879402576776968, -18.46583800616800630, -1.500000000000002220 ) ) ;
#25012 = FACE_OUTER_BOUND ( 'NONE', #75375, .T. ) ;
#25013 = ORIENTED_EDGE ( 'NONE', *, *, #87049, .T. ) ;
#25014 = EDGE_CURVE ( 'NONE', #59202, #1020, #27494, .T. ) ;
#25015 = CARTESIAN_POINT ( 'NONE',  ( 16.53150372360616771, 10.32350692489952593, 11.49999999999999645 ) ) ;
#25016 = CARTESIAN_POINT ( 'NONE',  ( -5.554587162835583847, -6.376774720514417183, 19.99258394656885329 ) ) ;
#25017 = EDGE_CURVE ( 'NONE', #39724, #91631, #42098, .T. ) ;
#25018 = CARTESIAN_POINT ( 'NONE',  ( 1.949999999999999956, 0.1925000000000007538, -0.1924999999999994493 ) ) ;
#25019 = ORIENTED_EDGE ( 'NONE', *, *, #66974, .T. ) ;
#25020 = VECTOR ( 'NONE', #53297, 1000.000000000000000 ) ;
#25021 = EDGE_CURVE ( 'NONE', #51300, #82863, #89882, .T. ) ;
#25022 = CARTESIAN_POINT ( 'NONE',  ( -98.58953762381673869, -24.66019654487199375, 8.947790411086119278 ) ) ;
#25023 = CARTESIAN_POINT ( 'NONE',  ( -32.52287095715006160, -23.48786465467240347, 11.44779295918255357 ) ) ;
#25024 = EDGE_CURVE ( 'NONE', #45617, #71712, #96530, .T. ) ;
#25025 = DIRECTION ( 'NONE',  ( 0.000000000000000000, 1.000000000000000000, 0.000000000000000000 ) ) ;
#25026 = B_SPLINE_CURVE_WITH_KNOTS ( 'NONE', 3,
 ( #77195, #31033, #7701, #69610 ),
 .UNSPECIFIED., .F., .F.,
 ( 4, 4 ),
 ( 0.000000000000000000, 9.999999999998897304E-05 ),
 .UNSPECIFIED. ) ;
#25027 = B_SPLINE_CURVE_WITH_KNOTS ( 'NONE', 3,
 ( #98765, #52111, #83036, #13526, #46991, #69826 ),
 .UNSPECIFIED., .F., .F.,
 ( 4, 2, 4 ),
 ( 0.000000000000000000, 0.001380901958385386376, 0.002761803916770772752 ),
 .UNSPECIFIED. ) ;
#25028 = CARTESIAN_POINT ( 'NONE',  ( -81.86427935766467101, -25.03155814569520743, 6.429953324065727394 ) ) ;
#25029 = CARTESIAN_POINT ( 'NONE',  ( 18.74904333037421011, -5.873301551693434597, -1.500000000000002220 ) ) ;
#25030 = ORIENTED_EDGE ( 'NONE', *, *, #78777, .T. ) ;
#25031 = CARTESIAN_POINT ( 'NONE',  ( 30.54125281784916268, 0.6647747205144264315, 23.11160796525322070 ) ) ;
#25032 = CARTESIAN_POINT ( 'NONE',  ( -114.6228709571500701, -23.47596703998600631, 11.44779298504227860 ) ) ;
#25034 = EDGE_CURVE ( 'NONE', #100167, #83385, #35107, .T. ) ;
#25033 = PERSON_AND_ORGANIZATION ( #70597, #27821 ) ;
#25035 = DIRECTION ( 'NONE',  ( 0.000000000000000000, -0.9999999999976377785, -2.173523156925979975E-06 ) ) ;
#25036 = LINE ( 'NONE', #86937, #8534 ) ;
#25037 = LINE ( 'NONE', #2224, #26619 ) ;
#25038 = CARTESIAN_POINT ( 'NONE',  ( -101.5951766307233441, -25.13932753814477294, 7.067349521424753256 ) ) ;
#25039 = CARTESIAN_POINT ( 'NONE',  ( 5.671135738765417322, -5.876774720514421624, 20.99074880795119924 ) ) ;
#25040 = CARTESIAN_POINT ( 'NONE',  ( -129.6239064868591981, -23.48783264082478084, -1.443836473390078590 ) ) ;
#25041 = DIRECTION ( 'NONE',  ( -4.218136541796977197E-15, -1.000000000000000000, -1.324960360541890271E-16 ) ) ;
#25042 = CARTESIAN_POINT ( 'NONE',  ( 11.38277053702107899, 16.36964821499295653, -1.500000000000002220 ) ) ;
#25043 = CARTESIAN_POINT ( 'NONE',  ( -100.4326965455114902, -25.19502912051678578, 3.293943094755625633 ) ) ;
#25044 = CARTESIAN_POINT ( 'NONE',  ( -18.24533751216517885, 7.751685665592884078, -1.500000000000002220 ) ) ;
#25045 = ORIENTED_EDGE ( 'NONE', *, *, #46594, .F. ) ;
#25046 = FACE_OUTER_BOUND ( 'NONE', #69527, .T. ) ;
#25047 = B_SPLINE_CURVE_WITH_KNOTS ( 'NONE', 3,
 ( #94318, #51034, #71503, #63909, #56288, #40551 ),
 .UNSPECIFIED., .F., .F.,
 ( 4, 2, 4 ),
 ( 6.384118696095308626E-06, 0.001386860460837117774, 0.002767336802978140158 ),
 .UNSPECIFIED. ) ;
#25048 = CARTESIAN_POINT ( 'NONE',  ( -50.73873594106601104, -25.13877094469005513, 7.069300430009204383 ) ) ;
#25049 = AXIS2_PLACEMENT_3D ( 'NONE', #19668, #19171, #51131 ) ;
#25050 = CARTESIAN_POINT ( 'NONE',  ( 4.784292611721462585, -6.376774720514426953, -25.54547254883130947 ) ) ;
#25051 = CARTESIAN_POINT ( 'NONE',  ( -19.40401905104624802, 7.283777608679691262, 11.49999999999999645 ) ) ;
#25052 = CARTESIAN_POINT ( 'NONE',  ( -7.640838998533831194, -6.376774720514417183, 20.32624910079993086 ) ) ;
#25053 = CARTESIAN_POINT ( 'NONE',  ( -106.5159538269883512, -24.15543982623907482, -0.2315651400026576268 ) ) ;
#25054 = CARTESIAN_POINT ( 'NONE',  ( 18.64237364862239943, 13.12531859369229359, 11.49999999999999645 ) ) ;
#25055 = ORIENTED_EDGE ( 'NONE', *, *, #87587, .F. ) ;
#25056 = CARTESIAN_POINT ( 'NONE',  ( -57.62287095715004881, -23.48783264082478794, -1.443836473390068820 ) ) ;
#25057 = DIRECTION ( 'NONE',  ( -1.000000000000000000, -3.773278334444167020E-23, -8.201307838832447938E-29 ) ) ;
#25058 = ORIENTED_EDGE ( 'NONE', *, *, #62975, .F. ) ;
#25059 = B_SPLINE_CURVE_WITH_KNOTS ( 'NONE', 3,
 ( #12597, #74496, #10855, #57046 ),
 .UNSPECIFIED., .F., .F.,
 ( 4, 4 ),
 ( 0.000000000000000000, 9.999999999998897304E-05 ),
 .UNSPECIFIED. ) ;
#25060 = CARTESIAN_POINT ( 'NONE',  ( 14.71488472389458124, -13.84269218943631508, 11.49999999999998934 ) ) ;
#25061 = CARTESIAN_POINT ( 'NONE',  ( 6.467769777575680834, -6.376774720514427841, 21.83821538399986650 ) ) ;
#25062 = CARTESIAN_POINT ( 'NONE',  ( -40.48088817674474882, -25.30533602047519892, 5.080586759489595039 ) ) ;
#25063 = EDGE_CURVE ( 'NONE', #47722, #67682, #84256, .T. ) ;
#25064 = ORIENTED_EDGE ( 'NONE', *, *, #35351, .F. ) ;
#25065 = CARTESIAN_POINT ( 'NONE',  ( -127.5228709571500616, -23.73907113216990794, -1.053371485793243467 ) ) ;
#25066 = CARTESIAN_POINT ( 'NONE',  ( -51.62287095715007013, -23.96127896941632685, -0.6493128931037859264 ) ) ;
#25067 = CARTESIAN_POINT ( 'NONE',  ( -12.72357806474857966, 15.40231687525621318, -1.500000000000002220 ) ) ;
#25068 = CARTESIAN_POINT ( 'NONE',  ( -40.94687764114259920, -25.04307374350000259, 7.563175304812659761 ) ) ;
#25069 = CARTESIAN_POINT ( 'NONE',  ( -4.092705237139750984, -20.55955383578756113, 11.49999999999999645 ) ) ;
#25070 = DIRECTION ( 'NONE',  ( -0.000000000000000000, 1.000000000000000000, -0.000000000000000000 ) ) ;
#25071 = CARTESIAN_POINT ( 'NONE',  ( -93.52287095715006160, -24.66019654487200086, 8.947790411086110396 ) ) ;
#25072 = CARTESIAN_POINT ( 'NONE',  ( 20.91424602935089894, 6.983905699820807556, -1.500000000000002220 ) ) ;
#25073 = EDGE_CURVE ( 'NONE', #70350, #88394, #5144, .T. ) ;
#25074 = AXIS2_PLACEMENT_3D ( 'NONE', #14065, #91198, #92688 ) ;
#25075 = CARTESIAN_POINT ( 'NONE',  ( -101.6228709571500559, -23.47593901973091235, -1.443836447539001089 ) ) ;
#25076 = ORIENTED_EDGE ( 'NONE', *, *, #32737, .T. ) ;
#25077 = CARTESIAN_POINT ( 'NONE',  ( -60.52287095715005449, -24.14321612903115621, -0.2833117244521560774 ) ) ;
#25078 = CARTESIAN_POINT ( 'NONE',  ( -49.51045894826389571, -25.18440238133807796, 3.920634963436217202 ) ) ;
#25079 = PLANE ( 'NONE',  #41336 ) ;
#25080 = VERTEX_POINT ( 'NONE', #7134 ) ;
#25081 = CARTESIAN_POINT ( 'NONE',  ( -68.52287095715006160, -29.50250243563736774, 8.947779886222143375 ) ) ;
#25082 = ORIENTED_EDGE ( 'NONE', *, *, #28380, .F. ) ;
#25083 = ORIENTED_EDGE ( 'NONE', *, *, #75083, .T. ) ;
#25084 = CARTESIAN_POINT ( 'NONE',  ( 32.33217928425140997, -6.376774720514426953, -12.20610769812822483 ) ) ;
#25085 = LINE ( 'NONE', #72283, #13017 ) ;
#25086 = DIRECTION ( 'NONE',  ( 0.000000000000000000, 2.173523156925980399E-06, -0.9999999999976378895 ) ) ;
#25087 = CARTESIAN_POINT ( 'NONE',  ( 17.35315496411208613, -10.91789592880838811, -1.500000000000002220 ) ) ;
#25088 = CIRCLE ( 'NONE', #81815, 28.45799999999999486 ) ;
#25089 = ORIENTED_EDGE ( 'NONE', *, *, #79261, .T. ) ;
#25090 = CARTESIAN_POINT ( 'NONE',  ( -71.62287095715004170, -23.96177878511308990, 10.65340807706330217 ) ) ;
#25091 = LINE ( 'NONE', #80391, #33702 ) ;
#25092 = CARTESIAN_POINT ( 'NONE',  ( -15.87499999999997868, 0.000000000000000000, 0.000000000000000000 ) ) ;
#25093 = CARTESIAN_POINT ( 'NONE',  ( 3.885606641962014329, -21.97303888676646721, 11.49999999999998934 ) ) ;
#25094 = CARTESIAN_POINT ( 'NONE',  ( -90.58953762381672448, -23.47593901973091235, -1.443836447539002865 ) ) ;
#25095 = DIRECTION ( 'NONE',  ( -3.773278334444166432E-23, 1.000000000000000000, 0.000000000000000000 ) ) ;
#25096 = ORIENTED_EDGE ( 'NONE', *, *, #21050, .F. ) ;
#25097 = CARTESIAN_POINT ( 'NONE',  ( 22.81105451610979173, 1.682774720514426114, -18.46691820600746681 ) ) ;
#25098 = CARTESIAN_POINT ( 'NONE',  ( -73.52287095715007581, -23.73907113216989728, -1.053371485793252793 ) ) ;
#25099 = B_SPLINE_CURVE_WITH_KNOTS ( 'NONE', 3,
 ( #49365, #80294, #41751, #72692, #67087, #5167, #21372, #29488, #66601, #13760, #89905, #4679, #59969, #51348, #90404, #37613, #75170, #97513 ),
 .UNSPECIFIED., .F., .F.,
 ( 4, 2, 2, 2, 2, 2, 2, 2, 4 ),
 ( 0.000000000000000000, 0.0005980878512858794297, 0.001196175702571757558, 0.001794263553857635470, 0.002392351405143513382, 0.002990439256429391728, 0.003588527107715270073, 0.004186614959001148419, 0.004784702810287026764 ),
 .UNSPECIFIED. ) ;
#25100 = CARTESIAN_POINT ( 'NONE',  ( -15.88994834598175387, -13.44966708658631838, -1.500000000000002220 ) ) ;
#25101 = VERTEX_POINT ( 'NONE', #67558 ) ;
#25103 = EDGE_LOOP ( 'NONE', ( #83362, #2233, #29512, #1262, #40235, #36696, #44638, #3742, #52030, #57453, #29138, #36867, #44598, #91313, #52391, #41182, #66960, #80024, #67666, #90642, #37959, #7740, #26360, #94768 ) ) ;
#25102 = CARTESIAN_POINT ( 'NONE',  ( -116.5228709571500900, -24.51283580621456792, 0.6167428607047249489 ) ) ;
#25104 = ORIENTED_EDGE ( 'NONE', *, *, #6973, .T. ) ;
#25105 = CARTESIAN_POINT ( 'NONE',  ( -70.28247728326880406, -25.25935350244192534, 7.560916518431925581 ) ) ;
#25106 = CARTESIAN_POINT ( 'NONE',  ( 1.225302832070333636, 21.05158420706169764, -1.500000000000002220 ) ) ;
#25107 = ORIENTED_EDGE ( 'NONE', *, *, #48666, .F. ) ;
#25108 = CARTESIAN_POINT ( 'NONE',  ( -110.6228709571500701, -23.84047902841603062, -0.8780736468305480047 ) ) ;
#25109 = CARTESIAN_POINT ( 'NONE',  ( 5.109298100548420152, -3.316774720514426456, -27.55941679637948383 ) ) ;
#25110 = CARTESIAN_POINT ( 'NONE',  ( -120.5169633428488254, -24.83644354573579349, 8.397322867130096569 ) ) ;
#25111 = CARTESIAN_POINT ( 'NONE',  ( -101.8248201165894073, -25.03152257312019202, 6.680466978398867717 ) ) ;
#25112 = CARTESIAN_POINT ( 'NONE',  ( -36.52287095715006870, -24.65952944569304606, 1.056160979905691910 ) ) ;
#25113 = CARTESIAN_POINT ( 'NONE',  ( -127.6228709571500559, -29.50248528299804818, 1.056150453629047137 ) ) ;
#25114 = CARTESIAN_POINT ( 'NONE',  ( -65.62287095715005592, -23.48786465467241058, 11.44779295918254647 ) ) ;
#25116 = VERTEX_POINT ( 'NONE', #44217 ) ;
#25115 = CARTESIAN_POINT ( 'NONE',  ( -15.96568504569681402, -15.38390974582250692, 11.49999999999999645 ) ) ;
#25117 = CARTESIAN_POINT ( 'NONE',  ( -108.9228709571500531, -23.47593901973090169, -1.443836447538996648 ) ) ;
#25118 = DIRECTION ( 'NONE',  ( -0.000000000000000000, -1.000000000000000000, -0.000000000000000000 ) ) ;
#25119 = ORIENTED_EDGE ( 'NONE', *, *, #26672, .T. ) ;
#25120 = CARTESIAN_POINT ( 'NONE',  ( 16.59953334139655468, -15.42474913338910980, 11.49999999999998934 ) ) ;
#25121 = EDGE_CURVE ( 'NONE', #97326, #19469, #6137, .T. ) ;
#25123 = VERTEX_POINT ( 'NONE', #69039 ) ;
#25122 = CARTESIAN_POINT ( 'NONE',  ( -125.6228709571500559, -29.50247984919015209, -1.443849546365044922 ) ) ;
#25124 = ORIENTED_EDGE ( 'NONE', *, *, #49282, .T. ) ;
#25125 = AXIS2_PLACEMENT_3D ( 'NONE', #97553, #13303, #6698 ) ;
#25126 = DIRECTION ( 'NONE',  ( 0.000000000000000000, 1.000000000000000000, 1.020425574104004246E-16 ) ) ;
#25127 = CARTESIAN_POINT ( 'NONE',  ( -17.16780662754360520, -10.58209718439171176, -1.500000000000002220 ) ) ;
#25128 = DIRECTION ( 'NONE',  ( 0.000000000000000000, -1.000000000000000000, 0.000000000000000000 ) ) ;
#25129 = ORIENTED_EDGE ( 'NONE', *, *, #4429, .T. ) ;
#25130 = EDGE_CURVE ( 'NONE', #84112, #34210, #36790, .T. ) ;
#25131 = CARTESIAN_POINT ( 'NONE',  ( -130.5728709571500588, -24.88826271230664489, 8.528479341549758175 ) ) ;
#25132 = CARTESIAN_POINT ( 'NONE',  ( -22.37156870845955225, 0.5457896250522937809, -1.500000000000002220 ) ) ;
#25133 = VERTEX_POINT ( 'NONE', #21349 ) ;
#25134 = ORIENTED_EDGE ( 'NONE', *, *, #6389, .F. ) ;
#25135 = CARTESIAN_POINT ( 'NONE',  ( -112.6283950228135495, -23.96169478059713498, 10.65365249895717348 ) ) ;
#25136 = CARTESIAN_POINT ( 'NONE',  ( -4.495793269230770939, -6.376774720514410077, 19.27714342948718595 ) ) ;
#25137 = ADVANCED_FACE ( 'NONE', ( #91871 ), #22342, .F. ) ;
#25138 = CARTESIAN_POINT ( 'NONE',  ( -40.29313279566920869, -25.31535333371619956, 5.078344701801774441 ) ) ;
#25139 = CARTESIAN_POINT ( 'NONE',  ( 31.62300803125484094, 5.234178280976530928, -3.660617518925037395 ) ) ;
#25140 = EDGE_CURVE ( 'NONE', #82652, #95350, #99967, .T. ) ;
#25141 = DIRECTION ( 'NONE',  ( -1.000000000000000000, -0.000000000000000000, -0.000000000000000000 ) ) ;
#25142 = CARTESIAN_POINT ( 'NONE',  ( -16.13938233076020268, 11.07636124087057183, 11.49999999999998934 ) ) ;
#25143 = B_SPLINE_CURVE_WITH_KNOTS ( 'NONE', 3,
 ( #30945, #8116, #77608, #41959 ),
 .UNSPECIFIED., .F., .F.,
 ( 4, 4 ),
 ( 0.000000000000000000, 0.0001000000000000167422 ),
 .UNSPECIFIED. ) ;
#25144 = ADVANCED_FACE ( 'NONE', ( #59949 ), #32859, .T. ) ;
#25145 = FACE_OUTER_BOUND ( 'NONE', #31859, .T. ) ;
#25146 = ORIENTED_EDGE ( 'NONE', *, *, #10972, .T. ) ;
#25147 = CARTESIAN_POINT ( 'NONE',  ( 19.88731969966643476, 8.162773808193900749, -1.500000000000002220 ) ) ;
#25148 = CARTESIAN_POINT ( 'NONE',  ( -128.5218876873007616, -23.96119346886882084, -0.6495511937831803806 ) ) ;
#25149 = EDGE_CURVE ( 'NONE', #84636, #85130, #7643, .T. ) ;
#25150 = CARTESIAN_POINT ( 'NONE',  ( 4.143214286797170409, 4.821574250326516875, -2.677392948487098267E-15 ) ) ;
#25151 = DIRECTION ( 'NONE',  ( -0.000000000000000000, -1.000000000000000000, -0.000000000000000000 ) ) ;
#25152 = CARTESIAN_POINT ( 'NONE',  ( -80.62287095715005592, -24.91570333823099759, 8.075032458375547506 ) ) ;
#25154 = AXIS2_PLACEMENT_3D ( 'NONE', #42072, #73506, #49684 ) ;
#25153 = CARTESIAN_POINT ( 'NONE',  ( -18.54830753475928518, 13.48922247889305837, -1.500000000000002220 ) ) ;
#25155 = PERSON_AND_ORGANIZATION ( #70597, #27821 ) ;
#25156 = CARTESIAN_POINT ( 'NONE',  ( -103.5228709571500758, -23.47596703998600631, 11.44779298504228215 ) ) ;
#25157 = CARTESIAN_POINT ( 'NONE',  ( -2.532641601674031850, -5.876774720514410077, 19.55266968305501507 ) ) ;
#25158 = CARTESIAN_POINT ( 'NONE',  ( -19.87929632332335927, 2.386914507623989490, 11.49999999999999645 ) ) ;
#25159 = CARTESIAN_POINT ( 'NONE',  ( -26.09636659181000340, -24.96935267319560126, 4.940287552382958580 ) ) ;
#25160 = CARTESIAN_POINT ( 'NONE',  ( -107.5895376238167387, -24.64898659630368272, 1.056161002820392270 ) ) ;
#25161 = LINE ( 'NONE', #50027, #36049 ) ;
#25162 = CARTESIAN_POINT ( 'NONE',  ( -103.5895376238167245, -24.64898659630368627, 1.056161002820392270 ) ) ;
#25163 = EDGE_CURVE ( 'NONE', #45754, #44715, #6833, .T. ) ;
#25164 = DIRECTION ( 'NONE',  ( 0.000000000000000000, -1.000000000000000000, 0.000000000000000000 ) ) ;
#25165 = CARTESIAN_POINT ( 'NONE',  ( 5.644138345009856117, 19.01542066204735448, 11.49999999999998934 ) ) ;
#25166 = VECTOR ( 'NONE', #78262, 1000.000000000000000 ) ;
#25167 = CARTESIAN_POINT ( 'NONE',  ( -19.76859095128058996, -9.124614402804876789, 11.49999999999998934 ) ) ;
#25168 = CARTESIAN_POINT ( 'NONE',  ( -90.62287095715001328, -24.83620972994592790, 8.398175272781360334 ) ) ;
#25169 = CARTESIAN_POINT ( 'NONE',  ( 3.778003860535555702, 19.31821889988591323, -1.500000000000002220 ) ) ;
#25170 = CIRCLE ( 'NONE', #2519, 2.249999999999998668 ) ;
#25171 = CARTESIAN_POINT ( 'NONE',  ( -42.66379183916900786, -23.48783264082477373, -1.443836473390076147 ) ) ;
#25172 = LINE ( 'NONE', #90445, #3014 ) ;
#25173 = DATE_TIME_ROLE ( 'classification_date' ) ;
#25174 = DIRECTION ( 'NONE',  ( 3.773278334444166432E-23, -1.000000000000000000, 0.000000000000000000 ) ) ;
#25175 = CARTESIAN_POINT ( 'NONE',  ( 2.627412086454235851, -6.376774720514420736, 20.59155478446653831 ) ) ;
#25176 = CARTESIAN_POINT ( 'NONE',  ( 15.34425395324244867, 13.73259486114767114, 11.49999999999999645 ) ) ;
#25177 = PLANE ( 'NONE',  #16508 ) ;
#25178 = CARTESIAN_POINT ( 'NONE',  ( -120.5880715386675064, -24.92564183028979485, 1.928384488918253092 ) ) ;
#25179 = CARTESIAN_POINT ( 'NONE',  ( -9.785633969878258398, 20.35780147342342516, 11.49999999999999645 ) ) ;
#25180 = VERTEX_POINT ( 'NONE', #8148 ) ;
#25181 = LINE ( 'NONE', #17575, #57321 ) ;
#25182 = CARTESIAN_POINT ( 'NONE',  ( -26.61313021603985263, -24.83282438599244912, 7.069134266065987937 ) ) ;
#25183 = CARTESIAN_POINT ( 'NONE',  ( -97.63250698802460192, -23.96119346886881374, -0.6495511937832058047 ) ) ;
#25184 = CARTESIAN_POINT ( 'NONE',  ( -72.62287095715005592, -23.47596703998600631, 11.44779298504227860 ) ) ;
#25185 = ADVANCED_FACE ( 'NONE', ( #69550 ), #79147, .T. ) ;
#25186 = DIRECTION ( 'NONE',  ( 0.000000000000000000, 1.000000000000000000, 0.000000000000000000 ) ) ;
#25187 = CARTESIAN_POINT ( 'NONE',  ( -125.5228709571500616, -23.47596703998600631, 11.44779298504227683 ) ) ;
#25188 = ADVANCED_FACE ( 'NONE', ( #78131 ), #41810, .T. ) ;
#25189 = ORIENTED_EDGE ( 'NONE', *, *, #4122, .T. ) ;
#25190 = CARTESIAN_POINT ( 'NONE',  ( -79.36292229018619082, -25.26750046495177671, 5.750285965674462041 ) ) ;
#25191 = CARTESIAN_POINT ( 'NONE',  ( 19.70479270790718829, 11.56945388388114360, -1.500000000000002220 ) ) ;
#25192 = DIRECTION ( 'NONE',  ( 0.000000000000000000, 1.000000000000000000, -0.000000000000000000 ) ) ;
#25193 = CARTESIAN_POINT ( 'NONE',  ( -106.6228709571500559, -23.48786465467241769, 11.44779295918253759 ) ) ;
#25194 = CARTESIAN_POINT ( 'NONE',  ( -82.58519193231559541, -24.51419770103156281, 9.386484678747187615 ) ) ;
#25195 = VECTOR ( 'NONE', #19445, 1000.000000000000000 ) ;
#25196 = CARTESIAN_POINT ( 'NONE',  ( 14.32739804834607256, 17.34395043298086847, 11.49999999999999645 ) ) ;
#25197 = ORIENTED_EDGE ( 'NONE', *, *, #26970, .F. ) ;
#25198 = CARTESIAN_POINT ( 'NONE',  ( 0.000000000000000000, 0.3850000000000053935, -1.529999999999998916 ) ) ;
#25199 = B_SPLINE_CURVE_WITH_KNOTS ( 'NONE', 3,
 ( #46543, #30306, #14582, #69878, #60781, #68875 ),
 .UNSPECIFIED., .F., .F.,
 ( 4, 2, 4 ),
 ( 6.384118678617110714E-06, 0.001386860460828379755, 0.002767336802978142326 ),
 .UNSPECIFIED. ) ;
#25200 = CARTESIAN_POINT ( 'NONE',  ( -15.43752342082821905, -15.63289427301443801, 11.49999999999998934 ) ) ;
#25201 = DIRECTION ( 'NONE',  ( -3.773278334453079030E-23, 0.9999999999976377785, 2.173523156925979128E-06 ) ) ;
#25202 = CARTESIAN_POINT ( 'NONE',  ( -34.53214318888519330, -24.51419770103156637, 9.386484678747176957 ) ) ;
#25203 = CARTESIAN_POINT ( 'NONE',  ( -68.94185455919210881, -25.23897982886904856, 6.276681587599555634 ) ) ;
#25204 = VERTEX_POINT ( 'NONE', #30974 ) ;
#25205 = CARTESIAN_POINT ( 'NONE',  ( -48.48926359912356077, -24.51419770103156637, 9.386484678747178734 ) ) ;
#25206 = ADVANCED_FACE ( 'NONE', ( #77137 ), #93876, .T. ) ;
#25207 = DIRECTION ( 'NONE',  ( -3.773278334453079030E-23, 0.9999999999976377785, 2.173523156925979128E-06 ) ) ;
#25208 = ORIENTED_EDGE ( 'NONE', *, *, #27811, .F. ) ;
#25209 = CARTESIAN_POINT ( 'NONE',  ( -2.888065500968368227, -20.30684875360264741, 11.49999999999998934 ) ) ;
#25210 = APPLICATION_CONTEXT ( 'configuration controlled 3d designs of mechanical parts and assemblies' ) ;
#25211 = ORIENTED_EDGE ( 'NONE', *, *, #3465, .T. ) ;
#25212 = EDGE_LOOP ( 'NONE', ( #47571, #77357, #36674, #1173 ) ) ;
#25213 = ORIENTED_EDGE ( 'NONE', *, *, #10597, .F. ) ;
#25214 = ORIENTED_EDGE ( 'NONE', *, *, #78157, .T. ) ;
#25215 = CARTESIAN_POINT ( 'NONE',  ( 8.651921485055520833, -21.43433228965458781, -1.500000000000002220 ) ) ;
#25216 = CARTESIAN_POINT ( 'NONE',  ( -112.5228709571500616, -23.48786465467241769, 11.44779295918253936 ) ) ;
#25217 = CARTESIAN_POINT ( 'NONE',  ( 13.61570878652767291, 15.11107311891478666, -1.500000000000002220 ) ) ;
#25218 = ADVANCED_FACE ( 'NONE', ( #92869 ), #17448, .T. ) ;
#25219 = ORIENTED_EDGE ( 'NONE', *, *, #48552, .T. ) ;
#25220 = FACE_OUTER_BOUND ( 'NONE', #70819, .T. ) ;
#25221 = CARTESIAN_POINT ( 'NONE',  ( -92.50939861997672153, -24.34968618360935011, 0.1864209137778966296 ) ) ;
#25222 = DIRECTION ( 'NONE',  ( 3.773278334444166432E-23, -1.000000000000000000, 0.000000000000000000 ) ) ;
#25223 = CARTESIAN_POINT ( 'NONE',  ( -97.62287095715008434, -23.47596703998600631, 11.44779298504227860 ) ) ;
#25225 = ORIENTED_EDGE ( 'NONE', *, *, #32363, .T. ) ;
#25224 = CARTESIAN_POINT ( 'NONE',  ( -7.189238790567602067, -20.27908067168375794, 11.49999999999999645 ) ) ;
#25226 = CARTESIAN_POINT ( 'NONE',  ( -75.59183437362925417, -24.40034930558991633, 0.3402023900116103450 ) ) ;
#25227 = CARTESIAN_POINT ( 'NONE',  ( -49.14050969713319716, -25.26385701502970704, 4.284284378226445256 ) ) ;
#25228 = VERTEX_POINT ( 'NONE', #25365 ) ;
#25229 = CARTESIAN_POINT ( 'NONE',  ( -15.27568272636907665, 14.01247568063241999, 11.49999999999998934 ) ) ;
#25230 = VERTEX_POINT ( 'NONE', #87263 ) ;
#25231 = PRODUCT_RELATED_PRODUCT_CATEGORY ( 'detail', '', ( #44230 ) ) ;
#25233 = ORIENTED_EDGE ( 'NONE', *, *, #48249, .T. ) ;
#25232 = CARTESIAN_POINT ( 'NONE',  ( -125.6240015775084942, -24.73486907724918638, 1.287355809206972346 ) ) ;
#25234 = AXIS2_PLACEMENT_3D ( 'NONE', #53422, #68644, #43811 ) ;
#25235 = CARTESIAN_POINT ( 'NONE',  ( -86.62287095715001328, -23.73907113216991149, -1.053371485793227924 ) ) ;
#25236 = CARTESIAN_POINT ( 'NONE',  ( -48.52287095715004739, -23.48783264083430211, -1.443836473375264440 ) ) ;
#25237 = ORIENTED_EDGE ( 'NONE', *, *, #56277, .T. ) ;
#25238 = EDGE_LOOP ( 'NONE', ( #75301, #17309, #86394, #94620 ) ) ;
#25239 = VECTOR ( 'NONE', #70430, 1000.000000000000000 ) ;
#25240 = CARTESIAN_POINT ( 'NONE',  ( -6.185411026474866958, -5.876774720514411854, 19.34586827028016742 ) ) ;
#25241 = DIRECTION ( 'NONE',  ( -0.000000000000000000, 2.173523156925979552E-06, -0.9999999999976378895 ) ) ;
#25242 = VECTOR ( 'NONE', #4054, 1000.000000000000114 ) ;
#25243 = CARTESIAN_POINT ( 'NONE',  ( -29.81066105410539535, -25.25535961780526861, 4.756373910324647625 ) ) ;
#25245 = ORIENTED_EDGE ( 'NONE', *, *, #92352, .F. ) ;
#25244 = CARTESIAN_POINT ( 'NONE',  ( -5.411813039392390223, -21.34095290059367755, 11.49999999999999645 ) ) ;
#25246 = VECTOR ( 'NONE', #6484, 1000.000000000000114 ) ;
#25247 = CARTESIAN_POINT ( 'NONE',  ( -103.6288243288032760, -24.15543982623907482, -0.2315651400026619011 ) ) ;
#25248 = CARTESIAN_POINT ( 'NONE',  ( 0.2737972009257602091, 22.58959237946467624, -1.500000000000002220 ) ) ;
#25249 = TOROIDAL_SURFACE ( 'NONE', #12269, 3.060000000000000053, 3.060000000000000053 ) ;
#25250 = CARTESIAN_POINT ( 'NONE',  ( 17.94697546605861760, -10.91086909363634838, 11.49999999999998934 ) ) ;
#25252 = ORIENTED_EDGE ( 'NONE', *, *, #82765, .T. ) ;
#25251 = CARTESIAN_POINT ( 'NONE',  ( -33.52287095715006160, -29.50250243563736774, 8.947779886222150481 ) ) ;
#25253 = ORIENTED_EDGE ( 'NONE', *, *, #12585, .T. ) ;
#25254 = DIRECTION ( 'NONE',  ( -0.000000000000000000, 1.000000000000000000, 0.000000000000000000 ) ) ;
#25255 = CYLINDRICAL_SURFACE ( 'NONE', #18145, 3.979149600822063704 ) ;
#25256 = ORIENTED_EDGE ( 'NONE', *, *, #31267, .F. ) ;
#25257 = CARTESIAN_POINT ( 'NONE',  ( -5.075574613727041218, 20.51645923614106337, 11.49999999999998934 ) ) ;
#25258 = CARTESIAN_POINT ( 'NONE',  ( -66.62287095715009855, -24.50321055353805022, 9.387540953477525818 ) ) ;
#25259 = CARTESIAN_POINT ( 'NONE',  ( -50.75822869421170225, -25.03148736841117739, 7.539273415008683976 ) ) ;
#25260 = CARTESIAN_POINT ( 'NONE',  ( -75.62287095715008434, -24.82558206586144323, 1.605769216559443269 ) ) ;
#25261 = CARTESIAN_POINT ( 'NONE',  ( -7.188523146553190912, -6.376774720514413630, 19.66116880005639800 ) ) ;
#25262 = LINE ( 'NONE', #56241, #66536 ) ;
#25263 = CARTESIAN_POINT ( 'NONE',  ( 16.02632597834478645, 15.35701383120132313, -1.500000000000002220 ) ) ;
#25264 = CARTESIAN_POINT ( 'NONE',  ( -114.6278450564630589, -23.96119346886881729, -0.6495511937831860427 ) ) ;
#25265 = EDGE_CURVE ( 'NONE', #87961, #17471, #87898, .T. ) ;
#25266 = ORIENTED_EDGE ( 'NONE', *, *, #22037, .T. ) ;
#25267 = FACE_OUTER_BOUND ( 'NONE', #49707, .T. ) ;
#25268 = DIRECTION ( 'NONE',  ( -1.000000000000000000, -0.000000000000000000, -0.000000000000000000 ) ) ;
#25269 = CARTESIAN_POINT ( 'NONE',  ( -1.608633542659107629, -19.34071428503001755, 11.49999999999999645 ) ) ;
#25270 = CARTESIAN_POINT ( 'NONE',  ( -71.52287095715010423, -23.48783264082477018, -1.443836473390091246 ) ) ;
#25271 = CARTESIAN_POINT ( 'NONE',  ( -100.4381051993576506, -25.11033443737754212, 2.832404817301930056 ) ) ;
#25272 = CARTESIAN_POINT ( 'NONE',  ( 18.70946937610417038, -5.484834493922766896, 11.49999999999998934 ) ) ;
#25273 = ADVANCED_FACE ( 'NONE', ( #33477 ), #80657, .F. ) ;
#25274 = CARTESIAN_POINT ( 'NONE',  ( 19.99361899508246765, -7.638522130635823082, -1.500000000000002220 ) ) ;
#25275 = LINE ( 'NONE', #86677, #75775 ) ;
#25276 = CARTESIAN_POINT ( 'NONE',  ( -60.58905053272714269, -24.52399227489755518, 9.353111116819372128 ) ) ;
#25277 = ADVANCED_FACE ( 'NONE', ( #3047 ), #56378, .T. ) ;
#25278 = CARTESIAN_POINT ( 'NONE',  ( -116.5228709571500616, -29.50248528299804818, 1.056150453629045360 ) ) ;
#25279 = CARTESIAN_POINT ( 'NONE',  ( 30.32108885906865936, 6.376774720514426953, 3.274824222184972822 ) ) ;
#25280 = CARTESIAN_POINT ( 'NONE',  ( 22.50852769316577096, -3.342225187595919689, -1.500000000000002220 ) ) ;
#25281 = DIRECTION ( 'NONE',  ( 1.000000000000000000, 0.000000000000000000, 0.000000000000000000 ) ) ;
#25282 = CARTESIAN_POINT ( 'NONE',  ( -102.5149031412999676, -24.15543982623908192, -0.2315651400026460249 ) ) ;
#25283 = DIRECTION ( 'NONE',  ( 1.000000000000000000, 3.773278334444167608E-23, 8.201307833595939069E-29 ) ) ;
#25284 = CARTESIAN_POINT ( 'NONE',  ( -19.08307359429613825, -5.530936995296134917, 11.49999999999999645 ) ) ;
#25285 = CARTESIAN_POINT ( 'NONE',  ( -84.52287095715001897, -24.51283580621364067, 0.6167428607019780351 ) ) ;
#25286 = CARTESIAN_POINT ( 'NONE',  ( -73.62287095715005592, -24.64898659630367916, 1.056161002820824368 ) ) ;
#25287 = CARTESIAN_POINT ( 'NONE',  ( -61.64687923781919920, -29.50248939449842922, 2.947779886236309377 ) ) ;
#25288 = EDGE_LOOP ( 'NONE', ( #39471, #48482, #88834, #10371 ) ) ;
#25289 = EDGE_CURVE ( 'NONE', #71512, #41368, #11142, .T. ) ;
#25290 = CARTESIAN_POINT ( 'NONE',  ( 10.86264265030973952, -0.3587747205144257157, -28.64597719988137570 ) ) ;
#25291 = DIRECTION ( 'NONE',  ( -1.000000000000000000, 0.000000000000000000, -0.000000000000000000 ) ) ;
#25292 = CARTESIAN_POINT ( 'NONE',  ( -63.62287095715004881, -23.48786465467241058, 11.44779295918254824 ) ) ;
#25293 = CARTESIAN_POINT ( 'NONE',  ( -6.994818212361641585, 20.52682044044541598, -1.500000000000002220 ) ) ;
#25294 = DIRECTION ( 'NONE',  ( 0.000000000000000000, 0.000000000000000000, 1.000000000000000000 ) ) ;
#25295 = CARTESIAN_POINT ( 'NONE',  ( -12.17249226084429203, 15.20430173202493940, -1.500000000000002220 ) ) ;
#25296 = AXIS2_PLACEMENT_3D ( 'NONE', #18187, #49160, #80086 ) ;
#25297 = CARTESIAN_POINT ( 'NONE',  ( -61.62287095715004881, -24.64965695001468404, 8.947790433994185832 ) ) ;
#25298 = ORIENTED_EDGE ( 'NONE', *, *, #79796, .T. ) ;
#25299 = CARTESIAN_POINT ( 'NONE',  ( -4.163110563111144913, -19.98234244090558320, 11.49999999999999645 ) ) ;
#25300 = PLANE ( 'NONE',  #73173 ) ;
#25301 = B_SPLINE_CURVE_WITH_KNOTS ( 'NONE', 3,
 ( #21144, #44502, #36382, #68834 ),
 .UNSPECIFIED., .F., .F.,
 ( 4, 4 ),
 ( 0.000000000000000000, 0.0001000000000000167422 ),
 .UNSPECIFIED. ) ;
#25302 = VECTOR ( 'NONE', #72511, 1000.000000000000000 ) ;
#25303 = CARTESIAN_POINT ( 'NONE',  ( -104.6228709571500559, -23.48783264082478794, -1.443836473390062158 ) ) ;
#25304 = ORIENTED_EDGE ( 'NONE', *, *, #14791, .T. ) ;
#25305 = CARTESIAN_POINT ( 'NONE',  ( -0.07401571716935598233, -22.09180837669121544, 9.787827635114012992 ) ) ;
#25306 = CARTESIAN_POINT ( 'NONE',  ( 33.57588617459661151, 3.431642488465076912, -12.05779067269562255 ) ) ;
#25307 = CARTESIAN_POINT ( 'NONE',  ( -39.04303308397306438, -25.27985266284889931, 4.215216948853407253 ) ) ;
#25308 = AXIS2_PLACEMENT_3D ( 'NONE', #63184, #33216, #25095 ) ;
#25309 = CARTESIAN_POINT ( 'NONE',  ( -49.27764846858840997, -25.31439483164234971, 6.145204854548993012 ) ) ;
#25310 = CIRCLE ( 'NONE', #82034, 1.149999999999998135 ) ;
#25311 = DIRECTION ( 'NONE',  ( -0.7071067811865507924, 0.000000000000000000, 0.7071067811865442421 ) ) ;
#25312 = VECTOR ( 'NONE', #48375, 1000.000000000000000 ) ;
#25313 = FACE_OUTER_BOUND ( 'NONE', #24629, .T. ) ;
#25314 = EDGE_LOOP ( 'NONE', ( #15139, #88715, #32927, #56188 ) ) ;
#25315 = CARTESIAN_POINT ( 'NONE',  ( -66.62364627127672634, -24.66019654487199375, 8.947790411086119278 ) ) ;
#25316 = AXIS2_PLACEMENT_3D ( 'NONE', #23681, #6972, #45546 ) ;
#25317 = EDGE_CURVE ( 'NONE', #33670, #47722, #73058, .T. ) ;
#25318 = CARTESIAN_POINT ( 'NONE',  ( 21.75294195941402364, -7.338126679257295670, 11.49999999999999645 ) ) ;
#25319 = CARTESIAN_POINT ( 'NONE',  ( 19.47892149737544187, 11.75266795981601753, -1.500000000000002220 ) ) ;
#25320 = ORIENTED_EDGE ( 'NONE', *, *, #76347, .T. ) ;
#25321 = CARTESIAN_POINT ( 'NONE',  ( 4.400426145423703694, -6.376774720514426065, 21.64763382324305852 ) ) ;
#25322 = CARTESIAN_POINT ( 'NONE',  ( 0.000000000000000000, 1.477225279485574028, 0.000000000000000000 ) ) ;
#25323 = CARTESIAN_POINT ( 'NONE',  ( -90.62618102488053751, -24.83618233451450763, 1.606449574219535492 ) ) ;
#25324 = CARTESIAN_POINT ( 'NONE',  ( -49.52287095715007581, -24.34917612406836440, 0.1852690917426526029 ) ) ;
#25325 = EDGE_CURVE ( 'NONE', #98147, #33008, #93996, .T. ) ;
#25326 = CARTESIAN_POINT ( 'NONE',  ( -69.51616040274272734, -23.73791477778911485, 11.05961554403170766 ) ) ;
#25327 = ADVANCED_FACE ( 'NONE', ( #22602 ), #34524, .T. ) ;
#25328 = CARTESIAN_POINT ( 'NONE',  ( -49.30270511914022080, -25.31386613526229823, 5.220951978813658023 ) ) ;
#25329 = CARTESIAN_POINT ( 'NONE',  ( -77.22287095715006444, -23.47596703998600631, 11.44779298504227860 ) ) ;
#25330 = CARTESIAN_POINT ( 'NONE',  ( -99.09705801370142808, -25.31200589627714237, 5.399822298496539830 ) ) ;
#25331 = EDGE_LOOP ( 'NONE', ( #4733, #88375, #50470, #84223 ) ) ;
#25332 = CARTESIAN_POINT ( 'NONE',  ( 20.39576089869593289, -0.2533167397448486957, -1.500000000000002220 ) ) ;
#25333 = ORIENTED_EDGE ( 'NONE', *, *, #82139, .T. ) ;
#25334 = ORIENTED_EDGE ( 'NONE', *, *, #99248, .F. ) ;
#25335 = CARTESIAN_POINT ( 'NONE',  ( 0.2859537766682072601, -23.01552763051285666, -1.500000000000002220 ) ) ;
#25336 = CARTESIAN_POINT ( 'NONE',  ( -1.540913562699879114, -6.376774720514410077, 19.44316438561912008 ) ) ;
#25337 = EDGE_LOOP ( 'NONE', ( #2546, #46932, #85262, #88897 ) ) ;
#25338 = AXIS2_PLACEMENT_3D ( 'NONE', #59228, #45506, #21635 ) ;
#25339 = CARTESIAN_POINT ( 'NONE',  ( -101.5895376238167245, -24.65952944569304606, 1.056160979905695907 ) ) ;
#25340 = CARTESIAN_POINT ( 'NONE',  ( -64.58953762381672448, -24.66019654487199020, 8.947790411086133489 ) ) ;
#25341 = LINE ( 'NONE', #95356, #54415 ) ;
#25342 = CARTESIAN_POINT ( 'NONE',  ( -29.52287095715007581, -24.57618165405973087, 1.056161296257514870 ) ) ;
#25344 = EDGE_LOOP ( 'NONE', ( #99719, #69659, #54603, #73911 ) ) ;
#25343 = CARTESIAN_POINT ( 'NONE',  ( 19.98943718749924159, -7.363913660680385220, 11.49999999999999645 ) ) ;
#25345 = ORIENTED_EDGE ( 'NONE', *, *, #14930, .F. ) ;
#25346 = CARTESIAN_POINT ( 'NONE',  ( -20.66209241242137296, -8.185968977665980972, -1.500000000000002220 ) ) ;
#25347 = CARTESIAN_POINT ( 'NONE',  ( 14.23986175545555355, -14.96101607593195304, 11.49999999999998934 ) ) ;
#25348 = ADVANCED_FACE ( 'NONE', ( #97380 ), #6409, .F. ) ;
#25349 = EDGE_CURVE ( 'NONE', #69866, #88394, #30330, .T. ) ;
#25350 = ORIENTED_EDGE ( 'NONE', *, *, #741, .T. ) ;
#25351 = FACE_OUTER_BOUND ( 'NONE', #33627, .T. ) ;
#25352 = CARTESIAN_POINT ( 'NONE',  ( -95.63174276445451483, -24.40133493613050319, 9.663955038902802386 ) ) ;
#25353 = ORIENTED_EDGE ( 'NONE', *, *, #30758, .T. ) ;
#25354 = CARTESIAN_POINT ( 'NONE',  ( -95.52287095715011844, -24.91544648472627088, 1.928969306349431090 ) ) ;
#25355 = ORIENTED_EDGE ( 'NONE', *, *, #91821, .F. ) ;
#25356 = CARTESIAN_POINT ( 'NONE',  ( -58.49786823486456200, -24.35071581493543036, 9.817618358456028815 ) ) ;
#25357 = CARTESIAN_POINT ( 'NONE',  ( 15.14581745102402088, -14.33592658440916523, -1.500000000000002220 ) ) ;
#25358 = CARTESIAN_POINT ( 'NONE',  ( -13.92312151449838531, -16.86485062357919773, 11.49999999999999645 ) ) ;
#25359 = CARTESIAN_POINT ( 'NONE',  ( 2.499999999999994671, 18.99999999999977618, 2.100000000000000089 ) ) ;
#25360 = CARTESIAN_POINT ( 'NONE',  ( -83.62287095715005592, -29.50247984919015209, -1.443849546365053582 ) ) ;
#25361 = CARTESIAN_POINT ( 'NONE',  ( -14.31525571501011207, 17.33968770572689166, -1.500000000000002220 ) ) ;
#25362 = EDGE_CURVE ( 'NONE', #18132, #55233, #75844, .T. ) ;
#25363 = EDGE_CURVE ( 'NONE', #12265, #10530, #58822, .T. ) ;
#25364 = AXIS2_PLACEMENT_3D ( 'NONE', #49778, #16799, #65015 ) ;
#25365 = CARTESIAN_POINT ( 'NONE',  ( 31.55236408230781819, -5.965225279485572685, 19.84760796525321780 ) ) ;
#25366 = DIRECTION ( 'NONE',  ( 1.000000000000000000, 0.000000000000000000, 0.000000000000000000 ) ) ;
#25367 = CARTESIAN_POINT ( 'NONE',  ( 4.038745349937860496, -5.876774720514428729, 21.81354843764681206 ) ) ;
#25368 = ORIENTED_EDGE ( 'NONE', *, *, #29760, .F. ) ;
#25369 = ORIENTED_EDGE ( 'NONE', *, *, #11967, .F. ) ;
#25370 = ORIENTED_EDGE ( 'NONE', *, *, #36199, .F. ) ;
#25371 = CARTESIAN_POINT ( 'NONE',  ( -52.52205781783337102, -23.48783264082478794, -1.443836473390069708 ) ) ;
#25372 = ORIENTED_EDGE ( 'NONE', *, *, #28255, .F. ) ;
#25373 = AXIS2_PLACEMENT_3D ( 'NONE', #4618, #11709, #49805 ) ;
#25374 = CARTESIAN_POINT ( 'NONE',  ( -9.048234560742015375, 19.43086790383670603, -1.500000000000002220 ) ) ;
#25375 = CARTESIAN_POINT ( 'NONE',  ( 19.81157572017019319, -10.35993776028809421, 11.49999999999999645 ) ) ;
#25376 = ORIENTED_EDGE ( 'NONE', *, *, #76008, .T. ) ;
#25377 = FACE_OUTER_BOUND ( 'NONE', #70024, .T. ) ;
#25378 = CIRCLE ( 'NONE', #82098, 1.306876713926001354 ) ;
#25379 = CARTESIAN_POINT ( 'NONE',  ( -19.04630365209304799, -9.011775662611203330, -1.500000000000002220 ) ) ;
#25380 = CARTESIAN_POINT ( 'NONE',  ( -30.46018077524497869, -23.77895705106414326, 10.97490056816818971 ) ) ;
#25381 = CARTESIAN_POINT ( 'NONE',  ( -13.91458393394894166, 14.26456941660895339, -1.500000000000002220 ) ) ;
#25382 = CARTESIAN_POINT ( 'NONE',  ( -50.47999461636793939, -24.83644354573578639, 8.397322867130096569 ) ) ;
#25383 = VECTOR ( 'NONE', #26871, 1000.000000000000114 ) ;
#25384 = CARTESIAN_POINT ( 'NONE',  ( -69.62287095715005592, -29.50248528299804818, 1.056150453629036701 ) ) ;
#25385 = CARTESIAN_POINT ( 'NONE',  ( -8.753671783739276790, -20.25744411100385634, -1.500000000000002220 ) ) ;
#25386 = ORIENTED_EDGE ( 'NONE', *, *, #35715, .F. ) ;
#25387 = CARTESIAN_POINT ( 'NONE',  ( -116.5903548954868825, -24.15543982623908548, -0.2315651400026406959 ) ) ;
#25388 = ADVANCED_FACE ( 'NONE', ( #100219 ), #77891, .T. ) ;
#25389 = PLANE ( 'NONE',  #96783 ) ;
#25390 = CARTESIAN_POINT ( 'NONE',  ( -2.238888094254589234, -20.74146561784671761, 11.49999999999999645 ) ) ;
#25391 = AXIS2_PLACEMENT_3D ( 'NONE', #10791, #27520, #74189 ) ;
#25392 = CARTESIAN_POINT ( 'NONE',  ( -62.64211077482075041, -23.96169478059712432, 10.65365249895718414 ) ) ;
#25393 = CARTESIAN_POINT ( 'NONE',  ( -54.62287095715005592, -29.50250243563736774, 8.947779886222146928 ) ) ;
#25394 = CARTESIAN_POINT ( 'NONE',  ( -79.11611000704996854, -29.50248939449842922, 2.947779886236309377 ) ) ;
#25395 = CARTESIAN_POINT ( 'NONE',  ( -14.93283513470682067, -15.21490397768744529, 11.49999999999998934 ) ) ;
#25396 = DIRECTION ( 'NONE',  ( -3.773278334453079618E-23, 0.9999999999976377785, 2.173523156925978705E-06 ) ) ;
#25397 = CARTESIAN_POINT ( 'NONE',  ( -124.5228709571500758, -24.33832256527049864, 0.1851278514138631481 ) ) ;
#25398 = B_SPLINE_CURVE_WITH_KNOTS ( 'NONE', 3,
 ( #62009, #77204, #46781, #1616, #39659, #38658 ),
 .UNSPECIFIED., .F., .F.,
 ( 4, 2, 4 ),
 ( 1.571346490231738784E-05, 0.001397069180539135423, 0.002778424896175953149 ),
 .UNSPECIFIED. ) ;
#25399 = EDGE_CURVE ( 'NONE', #3013, #49044, #57727, .T. ) ;
#25400 = CARTESIAN_POINT ( 'NONE',  ( -96.52287095715006160, -23.73934037231757443, 11.05740245334328087 ) ) ;
#25401 = CARTESIAN_POINT ( 'NONE',  ( -5.563047341353722253, -5.876774720514414518, 20.06599527532950589 ) ) ;
#25402 = CARTESIAN_POINT ( 'NONE',  ( 22.42242567092132433, 2.420433022335332751, -1.500000000000002220 ) ) ;
#25403 = EDGE_CURVE ( 'NONE', #53678, #93213, #24983, .T. ) ;
#25404 = CARTESIAN_POINT ( 'NONE',  ( -51.52287095715006870, -24.51387760970724372, 9.387446482453414731 ) ) ;
#25405 = VERTEX_POINT ( 'NONE', #16497 ) ;
#25406 = CARTESIAN_POINT ( 'NONE',  ( -35.62287095715006302, -24.83620972994591369, 8.398175272781365663 ) ) ;
#25407 = CARTESIAN_POINT ( 'NONE',  ( -31.66886117127272371, -23.48786465467240347, 11.44779295918255535 ) ) ;
#25408 = CARTESIAN_POINT ( 'NONE',  ( 18.28535361393070957, 7.309334553982634652, 11.49999999999999645 ) ) ;
#25409 = FACE_BOUND ( 'NONE', #74733, .T. ) ;
#25410 = DIRECTION ( 'NONE',  ( -1.334402673828313586E-16, 0.000000000000000000, 1.000000000000000000 ) ) ;
#25411 = EDGE_LOOP ( 'NONE', ( #10214, #29441, #26879, #88753 ) ) ;
#25412 = ADVANCED_FACE ( 'NONE', ( #786 ), #33233, .F. ) ;
#25413 = CARTESIAN_POINT ( 'NONE',  ( -44.52287095715006160, -23.47593901973090169, -1.443836447538997092 ) ) ;
#25414 = CARTESIAN_POINT ( 'NONE',  ( -61.52287095715006160, -23.48786465467241058, 11.44779295918254824 ) ) ;
#25415 = CIRCLE ( 'NONE', #95086, 1.000000000000000000 ) ;
#25416 = CARTESIAN_POINT ( 'NONE',  ( 5.109298100548420152, 3.316774720514426456, -27.55941679637948383 ) ) ;
#25417 = DIRECTION ( 'NONE',  ( 0.000000000000000000, 1.000000000000000000, 1.020425574104004246E-16 ) ) ;
#25418 = EDGE_CURVE ( 'NONE', #91672, #76346, #31095, .T. ) ;
#25419 = LINE ( 'NONE', #9695, #57835 ) ;
#25420 = CARTESIAN_POINT ( 'NONE',  ( 19.18382676146983457, -4.683391092530263755, -1.500000000000002220 ) ) ;
#25421 = ORIENTED_EDGE ( 'NONE', *, *, #9954, .F. ) ;
#25422 = VECTOR ( 'NONE', #93510, 1000.000000000000000 ) ;
#25423 = CARTESIAN_POINT ( 'NONE',  ( -19.33604739795523741, 5.927148246271303655, 11.49999999999999645 ) ) ;
#25424 = CARTESIAN_POINT ( 'NONE',  ( 5.642655980204820843, -5.876774720514418959, 20.71586687040766961 ) ) ;
#25425 = ORIENTED_EDGE ( 'NONE', *, *, #40383, .F. ) ;
#25426 = DIRECTION ( 'NONE',  ( 0.1478094111296165691, -0.9890158633619158257, 0.000000000000000000 ) ) ;
#25427 = CARTESIAN_POINT ( 'NONE',  ( -80.60265468748725937, -25.30556074514798937, 4.974404013225617760 ) ) ;
#25428 = CARTESIAN_POINT ( 'NONE',  ( -50.44873633328847262, -25.30399780216363226, 5.199041709259373256 ) ) ;
#25429 = CARTESIAN_POINT ( 'NONE',  ( 11.78947449592735275, -0.3587747205144256601, -28.08498176919931666 ) ) ;
#25430 = DIRECTION ( 'NONE',  ( 0.000000000000000000, 1.000000000000000000, 0.000000000000000000 ) ) ;
#25431 = CARTESIAN_POINT ( 'NONE',  ( -31.52287095715006160, -23.47596703998600631, 11.44779298504229459 ) ) ;
#25432 = CARTESIAN_POINT ( 'NONE',  ( 13.83478396660306942, -14.44641118834825910, 11.49999999999998934 ) ) ;
#25433 = DIRECTION ( 'NONE',  ( -0.9903949459893287566, -0.09776975748868939331, -0.09776975748869010108 ) ) ;
#25434 = CARTESIAN_POINT ( 'NONE',  ( 10.86264265030973952, -0.3587747205144257157, -27.62597719988137612 ) ) ;
#25435 = VERTEX_POINT ( 'NONE', #55087 ) ;
#25436 = AXIS2_PLACEMENT_3D ( 'NONE', #7546, #78542, #93779 ) ;
#25437 = EDGE_CURVE ( 'NONE', #61918, #65344, #26262, .T. ) ;
#25438 = CARTESIAN_POINT ( 'NONE',  ( -104.6228709571500843, -23.73934037231757799, 11.05740245334328442 ) ) ;
#25439 = CARTESIAN_POINT ( 'NONE',  ( -33.62287095715006302, -23.73907113216990794, -1.053371485793237472 ) ) ;
#25440 = CARTESIAN_POINT ( 'NONE',  ( 10.24059822343757808, -6.376774720514426953, 22.08128695274315945 ) ) ;
#25441 = CARTESIAN_POINT ( 'NONE',  ( -80.64675904551154417, -25.21083105912962807, 3.409327675794629808 ) ) ;
#25442 = CARTESIAN_POINT ( 'NONE',  ( -101.7776484685884242, -25.26303730729093644, 3.986250639247583827 ) ) ;
#25443 = AXIS2_PLACEMENT_3D ( 'NONE', #18583, #56679, #48567 ) ;
#25444 = CARTESIAN_POINT ( 'NONE',  ( 15.37486457892693181, 3.577890193782808037, -28.28298033016838886 ) ) ;
#25446 = CIRCLE ( 'NONE', #14066, 18.50000000000000000 ) ;
#25445 = CARTESIAN_POINT ( 'NONE',  ( -99.90788617779853098, -25.11539320716599732, 2.804431449967498491 ) ) ;
#25447 = ORIENTED_EDGE ( 'NONE', *, *, #81530, .F. ) ;
#25448 = AXIS2_PLACEMENT_3D ( 'NONE', #93751, #25241, #77014 ) ;
#25449 = CARTESIAN_POINT ( 'NONE',  ( 11.01437679584920026, 17.03896688766576517, 11.49999999999998934 ) ) ;
#25450 = B_SPLINE_CURVE_WITH_KNOTS ( 'NONE', 3,
 ( #51597, #97760, #90645, #42502, #58217, #21125 ),
 .UNSPECIFIED., .F., .F.,
 ( 4, 2, 4 ),
 ( 6.391158118956848875E-06, 0.001387004593080777039, 0.002767618028042597225 ),
 .UNSPECIFIED. ) ;
#25451 = CARTESIAN_POINT ( 'NONE',  ( -126.5228709571499763, -23.48783264082477018, -1.443836473390082142 ) ) ;
#25452 = CARTESIAN_POINT ( 'NONE',  ( -127.6236462943679015, -24.51419770103158768, 9.386484678747160970 ) ) ;
#25453 = CARTESIAN_POINT ( 'NONE',  ( -59.62768243989484063, -24.51419770103156281, 9.386484678747184063 ) ) ;
#25454 = CARTESIAN_POINT ( 'NONE',  ( -2.449489742783178770, -16.94322527948557422, 2.499999999999999556 ) ) ;
#25455 = CARTESIAN_POINT ( 'NONE',  ( -30.47287095715007510, -23.47596703474403768, 11.44538124590455830 ) ) ;
#25456 = CARTESIAN_POINT ( 'NONE',  ( -5.075574613727041218, 20.51645923614106337, 11.49999999999999645 ) ) ;
#25457 = CARTESIAN_POINT ( 'NONE',  ( -5.973063517705734071, 21.31661749205449041, -1.500000000000002220 ) ) ;
#25458 = CARTESIAN_POINT ( 'NONE',  ( -19.39287000742378453, 6.875061630626206011, -1.500000000000002220 ) ) ;
#25459 = ADVANCED_FACE ( 'NONE', ( #57096 ), #2086, .T. ) ;
#25460 = ORIENTED_EDGE ( 'NONE', *, *, #87977, .F. ) ;
#25461 = CARTESIAN_POINT ( 'NONE',  ( -88.62287095715004170, -23.47596703998600631, 11.44779298504227860 ) ) ;
#25462 = ORIENTED_EDGE ( 'NONE', *, *, #18771, .F. ) ;
#25463 = DIRECTION ( 'NONE',  ( 0.000000000000000000, 0.9999999999976377785, 2.173523156925979128E-06 ) ) ;
#25464 = DIRECTION ( 'NONE',  ( -3.773278334453079030E-23, 0.9999999999976377785, 2.173523156925979128E-06 ) ) ;
#25465 = ORIENTED_EDGE ( 'NONE', *, *, #89296, .F. ) ;
#25466 = ORIENTED_EDGE ( 'NONE', *, *, #92775, .T. ) ;
#25467 = ORIENTED_EDGE ( 'NONE', *, *, #22301, .T. ) ;
#25468 = CARTESIAN_POINT ( 'NONE',  ( -81.62287095715007013, -23.72773821059536559, 11.05748984161097503 ) ) ;
#25469 = DIRECTION ( 'NONE',  ( -3.773278334453079030E-23, 0.9999999999976377785, 2.173523156925979128E-06 ) ) ;
#25470 = CARTESIAN_POINT ( 'NONE',  ( 5.367993895751241418, -6.376774720514418959, 20.45854982692612722 ) ) ;
#25471 = CARTESIAN_POINT ( 'NONE',  ( -10.81534556030752725, -17.66751395530895152, -1.500000000000002220 ) ) ;
#25472 = CARTESIAN_POINT ( 'NONE',  ( -10.04279811845843007, 19.21892966915218892, 11.49999999999999645 ) ) ;
#25473 = VERTEX_POINT ( 'NONE', #9895 ) ;
#25474 = EDGE_CURVE ( 'NONE', #60922, #88443, #38281, .T. ) ;
#25475 = DIRECTION ( 'NONE',  ( -0.000000000000000000, -0.000000000000000000, -1.000000000000000000 ) ) ;
#25476 = AXIS2_PLACEMENT_3D ( 'NONE', #39717, #87399, #62573 ) ;
#25477 = CARTESIAN_POINT ( 'NONE',  ( -109.5895376238167103, -23.48786465467242124, 11.44779295918253936 ) ) ;
#25478 = CARTESIAN_POINT ( 'NONE',  ( 22.28251467978060063, -2.329348454117679879, -1.500000000000002220 ) ) ;
#25479 = ADVANCED_FACE ( 'NONE', ( #25625 ), #56597, .T. ) ;
#25480 = EDGE_CURVE ( 'NONE', #10565, #83385, #64924, .T. ) ;
#25481 = CARTESIAN_POINT ( 'NONE',  ( -47.58715896144654778, -24.35071581493542325, 9.817618358456030592 ) ) ;
#25482 = PLANE ( 'NONE',  #22174 ) ;
#25483 = ORIENTED_EDGE ( 'NONE', *, *, #74075, .T. ) ;
#25484 = CARTESIAN_POINT ( 'NONE',  ( -41.32836283488544638, -2.803225279485573207, 39.26872235229541985 ) ) ;
#25485 = CARTESIAN_POINT ( 'NONE',  ( 12.40597316965629560, -5.152774720514427642, -26.28458722401733993 ) ) ;
#25486 = B_SPLINE_CURVE_WITH_KNOTS ( 'NONE', 3,
 ( #22869, #53854, #15272, #59, #31002, #62465, #61969, #93395 ),
 .UNSPECIFIED., .F., .F.,
 ( 4, 2, 2, 4 ),
 ( 2.306480500801492503E-11, 0.003266960683657127180, 0.004900441013953289217, 0.006533921344249451688 ),
 .UNSPECIFIED. ) ;
#25487 = B_SPLINE_SURFACE_WITH_KNOTS ( 'NONE', 3, 1, ( 
 ( #92105, #84494 ),
 ( #85487, #84989 ),
 ( #15474, #62676 ),
 ( #31200, #22572 ),
 ( #29714, #53067 ),
 ( #60682, #91604 ),
 ( #256, #62173 ),
 ( #93096, #14976 ),
 ( #23579, #77863 ),
 ( #79874, #48445 ),
 ( #64187, #71781 ),
 ( #88501, #65190 ),
 ( #8870, #70774 ),
 ( #41841, #9364 ),
 ( #26095, #96114 ),
 ( #26603, #63173 ),
 ( #39816, #95108 ),
 ( #25596, #63684 ),
 ( #57564, #72783 ) ),
 .UNSPECIFIED., .F., .F., .F.,
 ( 4, 1, 1, 1, 1, 1, 1, 1, 1, 1, 1, 1, 1, 1, 1, 1, 4 ),
 ( 2, 2 ),
 ( 0.000000000000000000, 0.07262534608343565457, 0.1419766113262349028, 0.2089849284189395640, 0.2739568703644438274, 0.3368893473968409547, 0.3987449534945883278, 0.4601158852788603260, 0.5208249225900263291, 0.5809944586324817806, 0.6401519276014631110, 0.6986224507562535102, 0.7572710809271603338, 0.8164266940046565058, 0.8762540482034655298, 0.9371652930625368194, 0.9999999999999998890 ),
 ( 0.000000000000000000, 1.000000000000000000 ),
 .UNSPECIFIED. ) ;
#25488 = EDGE_CURVE ( 'NONE', #97694, #36363, #20139, .T. ) ;
#25489 = ORIENTED_EDGE ( 'NONE', *, *, #60319, .T. ) ;
#25490 = AXIS2_PLACEMENT_3D ( 'NONE', #11925, #51000, #36763 ) ;
#25491 = EDGE_LOOP ( 'NONE', ( #98125, #49992, #1724, #28686 ) ) ;
#25492 = CARTESIAN_POINT ( 'NONE',  ( -39.55620429048339304, -24.66019654487199020, 8.947790411086135265 ) ) ;
#25493 = VERTEX_POINT ( 'NONE', #27130 ) ;
#25494 = CARTESIAN_POINT ( 'NONE',  ( 30.53060340732037048, -2.682774720514426559, -2.322449884495168870 ) ) ;
#25495 = CARTESIAN_POINT ( 'NONE',  ( 21.23515499356076930, 0.7789969333488580006, -1.500000000000002220 ) ) ;
#25496 = VERTEX_POINT ( 'NONE', #90515 ) ;
#25497 = CARTESIAN_POINT ( 'NONE',  ( -100.9048517508088310, -25.13595419642503614, 7.026370735367747145 ) ) ;
#25498 = PRODUCT_DEFINITION_SHAPE ( 'NONE', 'NONE',  #100429 ) ;
#25499 = CARTESIAN_POINT ( 'NONE',  ( -15.20188179817220231, 15.67080601223297442, 11.49999999999998934 ) ) ;
#25500 = CARTESIAN_POINT ( 'NONE',  ( -52.53219595083381677, -24.66019654487198665, 8.947790411086131712 ) ) ;
#25501 = DIRECTION ( 'NONE',  ( 0.000000000000000000, 0.9999999999976377785, 2.173523156925979975E-06 ) ) ;
#25502 = CARTESIAN_POINT ( 'NONE',  ( 6.058092820189922456, -5.876774720514413630, 19.77091638250125882 ) ) ;
#25503 = CARTESIAN_POINT ( 'NONE',  ( -21.73523922981167189, -2.474665994198115726, -1.500000000000002220 ) ) ;
#25504 = CARTESIAN_POINT ( 'NONE',  ( 10.57556460110582996, 0.7139560615726621151, -8.999999999999994671 ) ) ;
#25505 = EDGE_LOOP ( 'NONE', ( #23657, #17506, #6450, #5647 ) ) ;
#25506 = CARTESIAN_POINT ( 'NONE',  ( 27.53860345374771867, 2.682774720514426559, -9.482392034746240483 ) ) ;
#25507 = CARTESIAN_POINT ( 'NONE',  ( -85.54115924640903756, -24.83644354573578994, 8.397322867130101898 ) ) ;
#25508 = EDGE_CURVE ( 'NONE', #45390, #59310, #19005, .T. ) ;
#25509 = VERTEX_POINT ( 'NONE', #28621 ) ;
#25510 = AXIS2_PLACEMENT_3D ( 'NONE', #70581, #17291, #15784 ) ;
#25511 = EDGE_LOOP ( 'NONE', ( #94519, #66591, #35342, #97205 ) ) ;
#25512 = EDGE_CURVE ( 'NONE', #82077, #79877, #39557, .T. ) ;
#25513 = ORIENTED_EDGE ( 'NONE', *, *, #35312, .T. ) ;
#25514 = LINE ( 'NONE', #8790, #42684 ) ;
#25515 = DIRECTION ( 'NONE',  ( -0.000000000000000000, 1.000000000000000000, -0.000000000000000000 ) ) ;
#25516 = CARTESIAN_POINT ( 'NONE',  ( 21.11169859150035677, 2.410084449224629832, -1.500000000000002220 ) ) ;
#25517 = CARTESIAN_POINT ( 'NONE',  ( -91.62287095715004170, -23.48783264082478794, -1.443836473390063713 ) ) ;
#25518 = FACE_OUTER_BOUND ( 'NONE', #49351, .T. ) ;
#25519 = EDGE_CURVE ( 'NONE', #97228, #39695, #65221, .T. ) ;
#25520 = CARTESIAN_POINT ( 'NONE',  ( 29.73860345376320424, 4.772779586519632744, -4.021226786694506394 ) ) ;
#25521 = AXIS2_PLACEMENT_3D ( 'NONE', #29566, #36689, #74254 ) ;
#25522 = CARTESIAN_POINT ( 'NONE',  ( 0.3000000000000007661, 0.000000000000000000, 21.89999999999999858 ) ) ;
#25523 = CARTESIAN_POINT ( 'NONE',  ( 19.05472526407214673, 3.605321472892077050, -1.500000000000002220 ) ) ;
#25524 = CARTESIAN_POINT ( 'NONE',  ( -45.63955093759643233, -24.52300882791528380, 0.6510814631126234930 ) ) ;
#25525 = EDGE_LOOP ( 'NONE', ( #45035, #85581, #79159, #71025 ) ) ;
#25526 = CARTESIAN_POINT ( 'NONE',  ( 17.91360334016800593, 7.682165803940314674, 11.49999999999999645 ) ) ;
#25527 = CARTESIAN_POINT ( 'NONE',  ( -5.533628790199073499, -5.876774720514415407, 19.87297243748313491 ) ) ;
#25528 = AXIS2_PLACEMENT_3D ( 'NONE', #66729, #29626, #60602 ) ;
#25529 = DIRECTION ( 'NONE',  ( 1.000000000000000000, -2.464095846557964090E-17, 0.000000000000000000 ) ) ;
#25530 = ORIENTED_EDGE ( 'NONE', *, *, #97089, .F. ) ;
#25531 = EDGE_CURVE ( 'NONE', #84743, #31713, #75659, .T. ) ;
#25532 = CARTESIAN_POINT ( 'NONE',  ( 4.948291700218025113, -5.876774720514418071, 20.47145334051262111 ) ) ;
#25533 = DIRECTION ( 'NONE',  ( -0.000000000000000000, 1.000000000000000000, -0.000000000000000000 ) ) ;
#25535 = ADVANCED_FACE ( 'NONE', ( #11896 ), #80911, .T. ) ;
#25534 = CARTESIAN_POINT ( 'NONE',  ( -90.52287095715007581, -24.92579138211019085, 1.929029949965666457 ) ) ;
#25536 = CARTESIAN_POINT ( 'NONE',  ( 5.265981236333619456E-16, -1.473225279485573802, -4.300000000000000711 ) ) ;
#25537 = CARTESIAN_POINT ( 'NONE',  ( 2.289404864003111051, -19.52285375609543294, 11.49999999999998934 ) ) ;
#25538 = ADVANCED_FACE ( 'NONE', ( #59585 ), #20495, .T. ) ;
#25539 = ORIENTED_EDGE ( 'NONE', *, *, #67636, .F. ) ;
#25540 = CARTESIAN_POINT ( 'NONE',  ( -94.62287095715005592, -23.47593901973091235, -1.443836447539002865 ) ) ;
#25541 = CARTESIAN_POINT ( 'NONE',  ( 21.06059016766346659, 9.494407541345388779, -1.500000000000002220 ) ) ;
#25542 = APPROVAL_ROLE ( '' ) ;
#25543 = CARTESIAN_POINT ( 'NONE',  ( -106.6228709571500559, -24.64965695001469115, 8.947790433994176951 ) ) ;
#25544 = DIRECTION ( 'NONE',  ( -0.7512896232465892110, -0.000000000000000000, -0.6599726524652350657 ) ) ;
#25545 = CARTESIAN_POINT ( 'NONE',  ( -105.5228709571500758, -23.48786465467241769, 11.44779295918253936 ) ) ;
#25546 = CARTESIAN_POINT ( 'NONE',  ( -97.62542694680625743, -24.51419770103157703, 9.386484678747176957 ) ) ;
#25547 = CARTESIAN_POINT ( 'NONE',  ( -119.5228709571500900, -23.72747288104470442, -1.053458166803224794 ) ) ;
#25548 = CARTESIAN_POINT ( 'NONE',  ( -44.52287095715004739, -23.48783264082477018, -1.443836473390094577 ) ) ;
#25549 = DIRECTION ( 'NONE',  ( 0.000000000000000000, -1.000000000000000000, 0.000000000000000000 ) ) ;
#25550 = CARTESIAN_POINT ( 'NONE',  ( -27.25988310792305214, 5.965225279485572685, 30.32664379231667695 ) ) ;
#25551 = CARTESIAN_POINT ( 'NONE',  ( -16.79965634883036074, 10.71410036745690597, 11.49999999999998934 ) ) ;
#25552 = CARTESIAN_POINT ( 'NONE',  ( -75.54002366634762211, -24.73531770709095312, 8.716586749053512051 ) ) ;
#25553 = CARTESIAN_POINT ( 'NONE',  ( 16.46483878678964174, 11.07114234313464252, -1.500000000000002220 ) ) ;
#25554 = EDGE_LOOP ( 'NONE', ( #8282, #88862, #68588 ) ) ;
#25555 = VECTOR ( 'NONE', #83773, 1000.000000000000114 ) ;
#25556 = CARTESIAN_POINT ( 'NONE',  ( -20.27875734969026311, 3.456774720514426136, 24.00402280011862288 ) ) ;
#25557 = CARTESIAN_POINT ( 'NONE',  ( -51.46098519185604658, -25.22106701273937901, 6.517326689665016382 ) ) ;
#25558 = CARTESIAN_POINT ( 'NONE',  ( -6.741682653110981249, -5.965225279485572685, 30.62569541381301619 ) ) ;
#25559 = CARTESIAN_POINT ( 'NONE',  ( 2.677173591928626806, -20.63698567995287902, 11.49999999999999645 ) ) ;
#25560 = CARTESIAN_POINT ( 'NONE',  ( -81.52213711276834829, -23.48783264082478084, -1.443836473390067043 ) ) ;
#25561 = CARTESIAN_POINT ( 'NONE',  ( -106.5228709571500758, -24.66019654487200441, 8.947790411086112172 ) ) ;
#25562 = CARTESIAN_POINT ( 'NONE',  ( 13.80103769381473811, 18.14473668730428813, 11.49999999999999645 ) ) ;
#25563 = ORIENTED_EDGE ( 'NONE', *, *, #68630, .T. ) ;
#25564 = B_SPLINE_SURFACE_WITH_KNOTS ( 'NONE', 3, 1, ( 
 ( #36515, #57887 ),
 ( #65507, #49772 ),
 ( #90309, #27912 ),
 ( #20779, #19291 ),
 ( #80703, #88320 ),
 ( #11678, #4588 ),
 ( #5570, #82192 ),
 ( #28908, #58378 ),
 ( #66994, #42660 ),
 ( #58870, #73594 ),
 ( #89811, #51757 ),
 ( #4083, #66007 ),
 ( #51254, #35036 ),
 ( #82689, #36018 ),
 ( #42164, #12678 ),
 ( #27422, #43642 ),
 ( #50760, #81704 ),
 ( #12176, #74580 ),
 ( #13170, #44141 ),
 ( #75068, #67481 ),
 ( #51907, #7204 ),
 ( #68619, #6211 ),
 ( #84328, #44295 ),
 ( #20934, #13316 ),
 ( #76214, #7711 ),
 ( #14814, #75712 ),
 ( #100036, #30040 ) ),
 .UNSPECIFIED., .F., .F., .F.,
 ( 4, 1, 1, 1, 1, 1, 1, 1, 1, 1, 1, 1, 1, 1, 1, 1, 1, 1, 1, 1, 1, 1, 1, 1, 4 ),
 ( 2, 2 ),
 ( 0.000000000000000000, 0.06859462225874241037, 0.1332460424433008772, 0.1943125864682560267, 0.2512792231169660995, 0.3045134392563467185, 0.3542349066533245772, 0.4004805887739885661, 0.4434107549384916913, 0.4840148686163448510, 0.5232523007732025055, 0.5610423727283596618, 0.5979002393643991775, 0.6335184888561948835, 0.6683143511696510997, 0.7024956712863812403, 0.7366853535134572084, 0.7702931693607888430, 0.8034372550192488971, 0.8359129516660280812, 0.8684602457892899308, 0.9008465382431827262, 0.9334665246307074504, 0.9662575752981232835, 0.9999999999999998890 ),
 ( 0.000000000000000000, 1.000000000000000000 ),
 .UNSPECIFIED. ) ;
#25565 = LINE ( 'NONE', #39780, #28448 ) ;
#25566 = DIRECTION ( 'NONE',  ( 0.000000000000000000, 0.000000000000000000, 1.000000000000000000 ) ) ;
#25567 = ORIENTED_EDGE ( 'NONE', *, *, #67803, .F. ) ;
#25568 = CARTESIAN_POINT ( 'NONE',  ( 11.17094659993960803, -16.83544227557131023, 11.49999999999998934 ) ) ;
#25569 = CARTESIAN_POINT ( 'NONE',  ( 7.448826589983275959, -6.376774720514420736, 21.05250386848070221 ) ) ;
#25570 = CARTESIAN_POINT ( 'NONE',  ( -49.62287095715005592, -24.65952944569304250, 1.056160979905693020 ) ) ;
#25571 = CIRCLE ( 'NONE', #9418, 3.349999999999998757 ) ;
#25572 = CARTESIAN_POINT ( 'NONE',  ( -35.62287095715005592, -23.47596703998600276, 11.44779298504227505 ) ) ;
#25573 = ORIENTED_EDGE ( 'NONE', *, *, #95650, .T. ) ;
#25574 = LINE ( 'NONE', #55035, #37152 ) ;
#25575 = CARTESIAN_POINT ( 'NONE',  ( -84.52287095715007581, -23.72773821059536914, 11.05748984161097503 ) ) ;
#25576 = CARTESIAN_POINT ( 'NONE',  ( -8.876215969300202957, 17.89991547088461488, -1.500000000000002220 ) ) ;
#25577 = CARTESIAN_POINT ( 'NONE',  ( 15.58962545129234911, 1.684774720514426560, -26.91365498785467025 ) ) ;
#25578 = CARTESIAN_POINT ( 'NONE',  ( -0.6469382494902750080, 20.97623560764392181, 11.49999999999999645 ) ) ;
#25579 = CARTESIAN_POINT ( 'NONE',  ( -29.03377166159867784, -24.89244382712345427, 7.705026311424929553 ) ) ;
#25580 = CARTESIAN_POINT ( 'NONE',  ( -70.57802021803216519, -25.00182538069146787, 7.747789668545044250 ) ) ;
#25581 = CARTESIAN_POINT ( 'NONE',  ( 10.81757466760856801, -19.22619917341675588, -1.500000000000002220 ) ) ;
#25582 = VECTOR ( 'NONE', #17870, 1000.000000000000000 ) ;
#25583 = CARTESIAN_POINT ( 'NONE',  ( 2.499999999999994671, 18.99999999999977618, 2.100000000000000089 ) ) ;
#25584 = ORIENTED_EDGE ( 'NONE', *, *, #13917, .T. ) ;
#25585 = DIRECTION ( 'NONE',  ( 0.000000000000000000, 0.000000000000000000, 1.000000000000000000 ) ) ;
#25586 = DIRECTION ( 'NONE',  ( 3.773278334444166432E-23, -1.000000000000000000, 0.000000000000000000 ) ) ;
#25587 = CARTESIAN_POINT ( 'NONE',  ( -72.50702299863668543, -24.15543982623907127, -0.2315651400026662310 ) ) ;
#25588 = EDGE_LOOP ( 'NONE', ( #53806, #11124, #58085, #72958 ) ) ;
#25589 = CARTESIAN_POINT ( 'NONE',  ( 2.589743589743596086, -6.376774720514415407, 20.00140224358974095 ) ) ;
#25590 = ADVANCED_FACE ( 'NONE', ( #66715 ), #87139, .T. ) ;
#25591 = VERTEX_POINT ( 'NONE', #76764 ) ;
#25592 = VECTOR ( 'NONE', #2692, 1000.000000000000000 ) ;
#25593 = EDGE_CURVE ( 'NONE', #46066, #93369, #69681, .T. ) ;
#25594 = ORIENTED_EDGE ( 'NONE', *, *, #50600, .T. ) ;
#25595 = CARTESIAN_POINT ( 'NONE',  ( 22.02124265030973760, -4.776774720514394446, 17.60402280011861009 ) ) ;
#25596 = CARTESIAN_POINT ( 'NONE',  ( -100.4784170818037552, -25.27404630553893483, 2.833155736553538695 ) ) ;
#25597 = DIRECTION ( 'NONE',  ( 0.000000000000000000, 1.000000000000000000, 0.000000000000000000 ) ) ;
#25598 = CARTESIAN_POINT ( 'NONE',  ( -15.16157141410761966, -13.82251119679066953, -1.500000000000002220 ) ) ;
#25599 = EDGE_CURVE ( 'NONE', #6180, #28046, #11691, .T. ) ;
#25600 = ORIENTED_EDGE ( 'NONE', *, *, #38542, .F. ) ;
#25601 = PLANE ( 'NONE',  #59151 ) ;
#25602 = DIRECTION ( 'NONE',  ( -0.000000000000000000, -1.000000000000000000, -0.000000000000000000 ) ) ;
#25603 = CARTESIAN_POINT ( 'NONE',  ( -59.52287095715006160, -29.50250243563736774, 8.947779886222145151 ) ) ;
#25604 = CARTESIAN_POINT ( 'NONE',  ( -22.22805510923732086, 2.117028069546627922, -1.500000000000002220 ) ) ;
#25605 = EDGE_CURVE ( 'NONE', #58179, #30443, #31104, .T. ) ;
#25606 = EDGE_CURVE ( 'NONE', #11920, #80847, #79445, .T. ) ;
#25607 = CARTESIAN_POINT ( 'NONE',  ( -81.62287095715005592, -24.64898659630528854, 1.056161002820826145 ) ) ;
#25608 = CARTESIAN_POINT ( 'NONE',  ( -1.359251851468251449, -5.876774720514419847, 20.71116975788854120 ) ) ;
#25609 = ORIENTED_EDGE ( 'NONE', *, *, #53445, .T. ) ;
#25610 = LINE ( 'NONE', #48460, #43623 ) ;
#25611 = DIRECTION ( 'NONE',  ( 0.000000000000000000, -0.000000000000000000, -1.000000000000000000 ) ) ;
#25612 = AXIS2_PLACEMENT_3D ( 'NONE', #72733, #65637, #79326 ) ;
#25613 = CARTESIAN_POINT ( 'NONE',  ( 2.550444227103870531, -20.70361394434535285, 11.49999999999998934 ) ) ;
#25614 = ORIENTED_EDGE ( 'NONE', *, *, #89398, .T. ) ;
#25616 = ORIENTED_EDGE ( 'NONE', *, *, #65667, .T. ) ;
#25615 = PLANE ( 'NONE',  #55205 ) ;
#25617 = VERTEX_POINT ( 'NONE', #38719 ) ;
#25618 = CARTESIAN_POINT ( 'NONE',  ( -2.499999999999993339, 18.99999999999977618, 2.100000000000000089 ) ) ;
#25619 = CARTESIAN_POINT ( 'NONE',  ( -14.29351441246084065, -15.47709782942846424, -1.500000000000002220 ) ) ;
#25620 = VERTEX_POINT ( 'NONE', #51965 ) ;
#25621 = CARTESIAN_POINT ( 'NONE',  ( -110.6228709571500559, -23.47593901973091235, -1.443836447538999312 ) ) ;
#25622 = DIRECTION ( 'NONE',  ( 0.000000000000000000, 0.000000000000000000, -1.000000000000000000 ) ) ;
#25623 = DIRECTION ( 'NONE',  ( 0.000000000000000000, -0.9999999999976377785, -2.173523156925979128E-06 ) ) ;
#25624 = CARTESIAN_POINT ( 'NONE',  ( -86.56264435747982589, -23.48786465467241058, 11.44779295918254647 ) ) ;
#25625 = FACE_OUTER_BOUND ( 'NONE', #30110, .T. ) ;
#25626 = CARTESIAN_POINT ( 'NONE',  ( 15.89274262425319861, 14.76810421718133171, -1.500000000000002220 ) ) ;
#25627 = CARTESIAN_POINT ( 'NONE',  ( -64.52287095715009002, -23.95044443724992078, 10.65354141964649592 ) ) ;
#25629 = ORIENTED_EDGE ( 'NONE', *, *, #4084, .T. ) ;
#25628 = CARTESIAN_POINT ( 'NONE',  ( 12.24756355222007898, 18.56953561607567238, 11.49999999999999645 ) ) ;
#25630 = CARTESIAN_POINT ( 'NONE',  ( -51.11433842476665035, -25.31441771568657018, 5.424622361140696292 ) ) ;
#25631 = EDGE_CURVE ( 'NONE', #95103, #100181, #98852, .T. ) ;
#25632 = CARTESIAN_POINT ( 'NONE',  ( -71.27633360938686735, -25.26738409628678639, 5.967369320731084059 ) ) ;
#25633 = ORIENTED_EDGE ( 'NONE', *, *, #3292, .T. ) ;
#25635 = ORIENTED_EDGE ( 'NONE', *, *, #95955, .F. ) ;
#25634 = CARTESIAN_POINT ( 'NONE',  ( -118.6228709571500701, -23.95044443724993144, 10.65354141964649415 ) ) ;
#25636 = EDGE_CURVE ( 'NONE', #95664, #23547, #60588, .T. ) ;
#25637 = VERTEX_POINT ( 'NONE', #52964 ) ;
#25638 = CARTESIAN_POINT ( 'NONE',  ( 31.71875899258513698, -3.424184405370887863, -3.672337713816452354 ) ) ;
#25639 = CARTESIAN_POINT ( 'NONE',  ( -15.35229381799144299, -13.07563953244551591, -1.500000000000002220 ) ) ;
#25640 = CARTESIAN_POINT ( 'NONE',  ( -126.5228709571500616, -23.47596703998600631, 11.44779298504227683 ) ) ;
#25641 = ORIENTED_EDGE ( 'NONE', *, *, #14807, .T. ) ;
#25642 = CARTESIAN_POINT ( 'NONE',  ( -130.5728709571500872, -24.41126829859231151, 0.1249348357876886167 ) ) ;
#25643 = CARTESIAN_POINT ( 'NONE',  ( 22.22467975111640470, 2.813832150844377100, -1.500000000000002220 ) ) ;
#25644 = EDGE_LOOP ( 'NONE', ( #7437, #82885, #44973, #87794 ) ) ;
#25645 = ORIENTED_EDGE ( 'NONE', *, *, #42286, .F. ) ;
#25646 = CARTESIAN_POINT ( 'NONE',  ( -20.27875734969026311, -7.835183881457444599, 22.60402280011862430 ) ) ;
#25647 = DIRECTION ( 'NONE',  ( -0.1875268396392987258, 0.000000000000000000, -0.9822594791677485837 ) ) ;
#25648 = CARTESIAN_POINT ( 'NONE',  ( -61.52287095715006870, -23.95044443724991368, 10.65354141964649415 ) ) ;
#25649 = CARTESIAN_POINT ( 'NONE',  ( -125.5228709571500616, -24.63287334234355441, 0.9662140553097673390 ) ) ;
#25650 = VECTOR ( 'NONE', #1092, 1000.000000000000114 ) ;
#25652 = EDGE_CURVE ( 'NONE', #7215, #7141, #58980, .T. ) ;
#25651 = CARTESIAN_POINT ( 'NONE',  ( -130.5728709571500588, -24.66459861931857134, 1.095224832288509420 ) ) ;
#25653 = CARTESIAN_POINT ( 'NONE',  ( -16.69004703121433408, -10.21020960635683394, 11.49999999999998934 ) ) ;
#25654 = CARTESIAN_POINT ( 'NONE',  ( -46.61531915723985264, -23.48783264082476663, -1.443836473390096575 ) ) ;
#25655 = ORIENTED_EDGE ( 'NONE', *, *, #8362, .T. ) ;
#25656 = CARTESIAN_POINT ( 'NONE',  ( -14.35963886870962192, 16.04489112172382903, -1.500000000000002220 ) ) ;
#25657 = CARTESIAN_POINT ( 'NONE',  ( 5.184553252003285984, -5.965225279485572685, -28.06387035751381731 ) ) ;
#25658 = CARTESIAN_POINT ( 'NONE',  ( -71.26594616156928907, -25.12219007819659566, 6.471658164502055222 ) ) ;
#25659 = CARTESIAN_POINT ( 'NONE',  ( -50.52287095715006160, -29.50248789122583659, 2.256150453626215580 ) ) ;
#25660 = EDGE_CURVE ( 'NONE', #38725, #54291, #30106, .T. ) ;
#25661 = DIRECTION ( 'NONE',  ( 0.000000000000000000, 0.000000000000000000, 1.000000000000000000 ) ) ;
#25662 = CARTESIAN_POINT ( 'NONE',  ( 19.54225192528841859, -11.95493969655435151, -1.500000000000002220 ) ) ;
#25663 = PERSON_AND_ORGANIZATION ( #70597, #27821 ) ;
#25664 = LINE ( 'NONE', #1839, #4592 ) ;
#25665 = CARTESIAN_POINT ( 'NONE',  ( -71.25889396629347061, -25.28176302922261343, 5.910822557617488648 ) ) ;
#25666 = CARTESIAN_POINT ( 'NONE',  ( -13.75281105048956576, 14.62798779934380811, 11.49999999999999645 ) ) ;
#25667 = FACE_OUTER_BOUND ( 'NONE', #90487, .T. ) ;
#25668 = CARTESIAN_POINT ( 'NONE',  ( -4.141025641025641413, -6.376774720514420736, 20.67377804487180271 ) ) ;
#25669 = AXIS2_PLACEMENT_3D ( 'NONE', #60895, #84707, #90330 ) ;
#25670 = DIRECTION ( 'NONE',  ( 0.000000000000000000, -1.000000000000000000, 0.000000000000000000 ) ) ;
#25671 = CYLINDRICAL_SURFACE ( 'NONE', #89363, 2.249999999999998668 ) ;
#25672 = CARTESIAN_POINT ( 'NONE',  ( -65.58953762381672448, -23.47593901973091235, -1.443836447539006196 ) ) ;
#25673 = CARTESIAN_POINT ( 'NONE',  ( -4.880483578727112359, 19.22116399702514045, 11.49999999999998934 ) ) ;
#25674 = CARTESIAN_POINT ( 'NONE',  ( -94.52287095715007581, -24.33927499327854349, 9.819080762295815390 ) ) ;
#25675 = CARTESIAN_POINT ( 'NONE',  ( -2.223759785643201869, -19.53228827767608777, -1.500000000000002220 ) ) ;
#25676 = CARTESIAN_POINT ( 'NONE',  ( 15.03220655128773942, -5.152774720514418760, -26.94699118253608816 ) ) ;
#25677 = AXIS2_PLACEMENT_3D ( 'NONE', #79208, #40665, #74111 ) ;
#25678 = CARTESIAN_POINT ( 'NONE',  ( -41.62287095715007013, -23.96177878511307924, 10.65340807706330928 ) ) ;
#25679 = APPROVAL_STATUS ( 'not_yet_approved' ) ;
#25680 = CARTESIAN_POINT ( 'NONE',  ( -60.52287095715006870, -24.62285846331436545, 9.038163153548243400 ) ) ;
#25681 = CARTESIAN_POINT ( 'NONE',  ( -39.06126217483156182, -25.29335695875766987, 4.454111424760057503 ) ) ;
#25682 = CARTESIAN_POINT ( 'NONE',  ( 20.52162115075873672, 2.272738508513782119, 11.49999999999999645 ) ) ;
#25683 = CARTESIAN_POINT ( 'NONE',  ( 7.749999999999998224, 25.69999999999999574, 0.000000000000000000 ) ) ;
#25684 = CARTESIAN_POINT ( 'NONE',  ( 32.16024265030974050, -5.965225279485572685, 14.03360796525321774 ) ) ;
#25685 = CARTESIAN_POINT ( 'NONE',  ( -22.43363504178351775, 2.973318333978472339, 11.49999999999999645 ) ) ;
#25686 = ORIENTED_EDGE ( 'NONE', *, *, #13837, .F. ) ;
#25687 =( NAMED_UNIT ( * ) SI_UNIT ( $, .STERADIAN. ) SOLID_ANGLE_UNIT ( ) );
#25688 = CARTESIAN_POINT ( 'NONE',  ( -69.45438311041971247, -25.12219042273241953, 6.630173073956423302 ) ) ;
#25689 = CARTESIAN_POINT ( 'NONE',  ( -45.52287095715006160, -29.50248528299804818, 1.056150453629033370 ) ) ;
#25690 = CARTESIAN_POINT ( 'NONE',  ( -97.51109013237558543, -24.34968618360934300, 0.1864209137778855829 ) ) ;
#25691 = CARTESIAN_POINT ( 'NONE',  ( -39.62287095715004170, -24.50216790748098461, 0.6166512839513541566 ) ) ;
#25692 = CARTESIAN_POINT ( 'NONE',  ( -110.5228709571500616, -23.48783264082477018, -1.443836473390086583 ) ) ;
#25693 = CARTESIAN_POINT ( 'NONE',  ( -28.52287095715007226, -24.35281102363228811, 9.387565062279906059 ) ) ;
#25694 = VERTEX_POINT ( 'NONE', #13880 ) ;
#25695 = PLANE ( 'NONE',  #82495 ) ;
#25696 = CARTESIAN_POINT ( 'NONE',  ( -16.39533425382319720, 15.89506036719111037, -1.500000000000002220 ) ) ;
#25697 = CARTESIAN_POINT ( 'NONE',  ( -110.4032350430226614, -25.18518318255442523, 3.295734047008243905 ) ) ;
#25698 = CARTESIAN_POINT ( 'NONE',  ( -106.6228709571500275, -24.51387760970725083, 9.387446482453409402 ) ) ;
#25699 = CARTESIAN_POINT ( 'NONE',  ( -63.49956169734852551, -24.35071581493543036, 9.817618358456027039 ) ) ;
#25700 = CARTESIAN_POINT ( 'NONE',  ( 20.52096793114426276, -9.243637136814692568, 11.49999999999999645 ) ) ;
#25701 = ORIENTED_EDGE ( 'NONE', *, *, #16424, .T. ) ;
#25702 = CARTESIAN_POINT ( 'NONE',  ( -78.52287095715006160, -29.50248528299804818, 1.056150453629038477 ) ) ;
#25703 = CARTESIAN_POINT ( 'NONE',  ( 21.77894307773758698, -2.757304969434911879, 11.49999999999998934 ) ) ;
#25704 = CARTESIAN_POINT ( 'NONE',  ( -114.5228709571500616, -24.64965694238408034, 8.947790433994192938 ) ) ;
#25705 = CARTESIAN_POINT ( 'NONE',  ( -34.54551871025724807, -24.15620529776627379, 10.23563542870661003 ) ) ;
#25706 = CARTESIAN_POINT ( 'NONE',  ( -69.88946996337978135, -25.04737768561031785, 7.495009054863854381 ) ) ;
#25707 = ORIENTED_EDGE ( 'NONE', *, *, #6354, .F. ) ;
#25708 = LINE ( 'NONE', #24208, #73498 ) ;
#25709 = LINE ( 'NONE', #95228, #85070 ) ;
#25710 = EDGE_LOOP ( 'NONE', ( #12143, #52718, #42003, #34369 ) ) ;
#25711 = CARTESIAN_POINT ( 'NONE',  ( -54.59888109123160405, -23.96169478059712787, 10.65365249895718947 ) ) ;
#25712 = EDGE_CURVE ( 'NONE', #5913, #84492, #75777, .T. ) ;
#25713 = CARTESIAN_POINT ( 'NONE',  ( 20.39306652673287701, -2.074774109220689500, -1.500000000000002220 ) ) ;
#25714 = ORIENTED_EDGE ( 'NONE', *, *, #55908, .T. ) ;
#25715 = VECTOR ( 'NONE', #95781, 1000.000000000000000 ) ;
#25716 = VERTEX_POINT ( 'NONE', #6769 ) ;
#25717 = ORIENTED_EDGE ( 'NONE', *, *, #24095, .F. ) ;
#25718 = ORIENTED_EDGE ( 'NONE', *, *, #39975, .F. ) ;
#25719 = CARTESIAN_POINT ( 'NONE',  ( 3.025806405283164136, -6.376774720514420736, 20.84867811309776542 ) ) ;
#25720 = CARTESIAN_POINT ( 'NONE',  ( -5.338719972479099241, 22.46511350730333589, -1.500000000000002220 ) ) ;
#25721 = DIRECTION ( 'NONE',  ( -3.773278334453079618E-23, 0.9999999999976377785, 2.173523156925979975E-06 ) ) ;
#25722 = CARTESIAN_POINT ( 'NONE',  ( 2.178911383790714584, -20.24183328246387958, -1.500000000000002220 ) ) ;
#25723 = EDGE_CURVE ( 'NONE', #49812, #32014, #14878, .T. ) ;
#25724 = VERTEX_POINT ( 'NONE', #93498 ) ;
#25725 = DIRECTION ( 'NONE',  ( -1.000000000000000000, 0.000000000000000000, 0.000000000000000000 ) ) ;
#25726 = CIRCLE ( 'NONE', #9574, 2.040000000000000036 ) ;
#25727 = CARTESIAN_POINT ( 'NONE',  ( -50.46347206883352499, -25.12095147923715643, 2.834909179762350906 ) ) ;
#25728 = ADVANCED_FACE ( 'NONE', ( #86896 ), #24493, .F. ) ;
#25729 = PLANE ( 'NONE',  #98263 ) ;
#25730 = CARTESIAN_POINT ( 'NONE',  ( 3.787259615384621192, -6.376774720514404748, 18.51923076923076295 ) ) ;
#25732 = ORIENTED_EDGE ( 'NONE', *, *, #97424, .F. ) ;
#25731 = CARTESIAN_POINT ( 'NONE',  ( 14.33184905138074683, -16.10332302735202958, 11.49999999999999645 ) ) ;
#25733 = CARTESIAN_POINT ( 'NONE',  ( -28.74075323809458737, -25.21531770609978906, 2.791732177081652555 ) ) ;
#25734 = CARTESIAN_POINT ( 'NONE',  ( -43.62287095715003460, -23.47596703998600276, 11.44779298504227505 ) ) ;
#25735 = EDGE_CURVE ( 'NONE', #16980, #12582, #78924, .T. ) ;
#25736 = B_SPLINE_CURVE_WITH_KNOTS ( 'NONE', 3,
 ( #96032, #71703, #33130, #25520, #56493 ),
 .UNSPECIFIED., .F., .F.,
 ( 4, 1, 4 ),
 ( 0.09110967255127218334, 0.09110974468632360157, 0.09110981682137500592 ),
 .UNSPECIFIED. ) ;
#25737 = ORIENTED_EDGE ( 'NONE', *, *, #89703, .F. ) ;
#25738 = VECTOR ( 'NONE', #46907, 1000.000000000000227 ) ;
#25739 = EDGE_CURVE ( 'NONE', #7414, #71653, #46844, .T. ) ;
#25740 = CARTESIAN_POINT ( 'NONE',  ( -5.109682455881146446, -20.12422286529520932, 11.49999999999998934 ) ) ;
#25741 = ORIENTED_EDGE ( 'NONE', *, *, #5143, .F. ) ;
#25743 = VERTEX_POINT ( 'NONE', #17894 ) ;
#25742 = CARTESIAN_POINT ( 'NONE',  ( -125.5209409955973854, -24.15503026093915295, -0.2815557561904348804 ) ) ;
#25744 = CARTESIAN_POINT ( 'NONE',  ( -77.52287095715009002, -23.72747288104470087, -1.053458166803226792 ) ) ;
#25745 = CARTESIAN_POINT ( 'NONE',  ( -38.62287095715005592, -29.50250243563736774, 8.947779886222148704 ) ) ;
#25746 = ORIENTED_EDGE ( 'NONE', *, *, #82080, .T. ) ;
#25747 = ORIENTED_EDGE ( 'NONE', *, *, #13333, .F. ) ;
#25748 = CARTESIAN_POINT ( 'NONE',  ( -5.837039262820512775, -5.876774720514413630, 19.76512419871795245 ) ) ;
#25749 = AXIS2_PLACEMENT_3D ( 'NONE', #19192, #66401, #82101 ) ;
#25750 = CARTESIAN_POINT ( 'NONE',  ( 13.91401389203221406, 5.965225279485572685, 158.0376437107427137 ) ) ;
#25751 = DIRECTION ( 'NONE',  ( 0.000000000000000000, 0.000000000000000000, 1.000000000000000000 ) ) ;
#25753 = ORIENTED_EDGE ( 'NONE', *, *, #70134, .F. ) ;
#25752 = CARTESIAN_POINT ( 'NONE',  ( -11.61111146657235871, -18.70866699758865792, 11.49999999999999645 ) ) ;
#25754 = CARTESIAN_POINT ( 'NONE',  ( -103.5114003720115221, -24.51314013834316086, 0.6176544820404170633 ) ) ;
#25755 = CARTESIAN_POINT ( 'NONE',  ( 15.88279217892459094, 16.07415641707351384, -1.500000000000002220 ) ) ;
#25756 = EDGE_CURVE ( 'NONE', #23622, #98743, #74592, .T. ) ;
#25758 = ORIENTED_EDGE ( 'NONE', *, *, #48524, .F. ) ;
#25757 = CARTESIAN_POINT ( 'NONE',  ( 16.30000000000000071, 0.000000000000000000, 0.000000000000000000 ) ) ;
#25759 = ORIENTED_EDGE ( 'NONE', *, *, #59915, .F. ) ;
#25760 = DIRECTION ( 'NONE',  ( 1.000000000000000000, 3.773278334444166432E-23, 8.201307841325785021E-29 ) ) ;
#25761 = AXIS2_PLACEMENT_3D ( 'NONE', #28173, #59132, #83946 ) ;
#25762 = CARTESIAN_POINT ( 'NONE',  ( -57.48874627035196028, -24.66019654487198665, 8.947790411086121054 ) ) ;
#25763 = ORIENTED_EDGE ( 'NONE', *, *, #11711, .T. ) ;
#25764 = CARTESIAN_POINT ( 'NONE',  ( -14.79452276021403634, 15.15755283273500531, 11.49999999999998934 ) ) ;
#25765 = CARTESIAN_POINT ( 'NONE',  ( -82.62287095715007013, -23.96127896941631619, -0.6493128931037839280 ) ) ;
#25766 = FACE_OUTER_BOUND ( 'NONE', #26621, .T. ) ;
#25767 = CARTESIAN_POINT ( 'NONE',  ( -7.294102189209645815, -5.876774720514413630, 19.89644244529368677 ) ) ;
#25768 = CARTESIAN_POINT ( 'NONE',  ( -41.33134938142555370, -25.30281732168844044, 5.289835615799674429 ) ) ;
#25769 = CARTESIAN_POINT ( 'NONE',  ( 22.20243239366838850, -0.07139729354238147363, -1.500000000000002220 ) ) ;
#25770 = CARTESIAN_POINT ( 'NONE',  ( -74.62287095715004170, -23.95044443724992789, 10.65354141964649415 ) ) ;
#25771 = ORIENTED_EDGE ( 'NONE', *, *, #36471, .F. ) ;
#25772 = CARTESIAN_POINT ( 'NONE',  ( 8.462785143989153269, 5.965225279485592225, -28.02084008811334215 ) ) ;
#25773 = LINE ( 'NONE', #12040, #75153 ) ;
#25774 = CARTESIAN_POINT ( 'NONE',  ( 14.52268490272241408, 12.84546865777419455, 11.49999999999999645 ) ) ;
#25775 = CARTESIAN_POINT ( 'NONE',  ( -36.60923577182816757, -23.73791477778911130, 11.05961554403171121 ) ) ;
#25776 = CARTESIAN_POINT ( 'NONE',  ( -116.5228709571500616, -24.64898659630368627, 1.056161002820833028 ) ) ;
#25777 = CARTESIAN_POINT ( 'NONE',  ( 19.19537281719634336, 3.394423509666608663, 11.49999999999998934 ) ) ;
#25778 = CARTESIAN_POINT ( 'NONE',  ( 6.029407872858970840, -20.54391778677962677, 11.49999999999998934 ) ) ;
#25779 = CARTESIAN_POINT ( 'NONE',  ( -85.52287095715006160, -24.51254535375845833, 9.355368624242183628 ) ) ;
#25780 = CARTESIAN_POINT ( 'NONE',  ( -108.5228709571500616, -29.50250243563736774, 8.947779886222136270 ) ) ;
#25781 = CARTESIAN_POINT ( 'NONE',  ( -51.52205508352526664, -23.48783264082476308, -1.443836473390094133 ) ) ;
#25782 = LINE ( 'NONE', #5437, #11733 ) ;
#25783 = CARTESIAN_POINT ( 'NONE',  ( -20.99730734726578874, -8.693733401623333634, -1.500000000000002220 ) ) ;
#25784 = ADVANCED_FACE ( 'NONE', ( #33115 ), #63079, .F. ) ;
#25785 = DIRECTION ( 'NONE',  ( -2.110806104557723378E-18, -1.000000000000000000, 1.734723475976817880E-18 ) ) ;
#25786 = CARTESIAN_POINT ( 'NONE',  ( -98.55008637382228187, -24.34968618360934300, 0.1864209137778828629 ) ) ;
#25787 = CARTESIAN_POINT ( 'NONE',  ( -80.52287095715006160, -24.91544648472620338, 1.928969306349231028 ) ) ;
#25788 = CARTESIAN_POINT ( 'NONE',  ( 17.36586316225375981, 9.700842922841564686, 11.49999999999999645 ) ) ;
#25789 = CARTESIAN_POINT ( 'NONE',  ( -123.5552286427682986, -24.15620529776629510, 10.23563542870659404 ) ) ;
#25790 = VECTOR ( 'NONE', #13962, 1000.000000000000000 ) ;
#25791 = VECTOR ( 'NONE', #77839, 1000.000000000000000 ) ;
#25792 = CARTESIAN_POINT ( 'NONE',  ( -67.62287095715005592, -24.65952944569304606, 1.056160979905697017 ) ) ;
#25793 = CARTESIAN_POINT ( 'NONE',  ( -17.64648606763744354, 5.965225279485594001, -23.04404205923972526 ) ) ;
#25794 = ORIENTED_EDGE ( 'NONE', *, *, #36586, .F. ) ;
#25795 = DIRECTION ( 'NONE',  ( -0.000000000000000000, 0.000000000000000000, -1.000000000000000000 ) ) ;
#25796 = EDGE_CURVE ( 'NONE', #96494, #59593, #85555, .T. ) ;
#25797 = CARTESIAN_POINT ( 'NONE',  ( -31.22207807101783317, -25.16370864782812689, 7.203858152271859439 ) ) ;
#25798 = CARTESIAN_POINT ( 'NONE',  ( -51.69862270353959843, -25.10935997717551160, 3.939198411942864020 ) ) ;
#25799 = CARTESIAN_POINT ( 'NONE',  ( -19.97641003480726241, 8.421946895145676848, 11.49999999999998934 ) ) ;
#25800 = DIRECTION ( 'NONE',  ( 0.8788171126619707119, -0.4771587602595987465, 0.000000000000000000 ) ) ;
#25801 = VECTOR ( 'NONE', #52446, 1000.000000000000000 ) ;
#25802 = CARTESIAN_POINT ( 'NONE',  ( -18.83898130102433299, -4.906684326670742280, -1.500000000000002220 ) ) ;
#25803 = DIRECTION ( 'NONE',  ( 0.000000000000000000, 0.000000000000000000, -1.000000000000000000 ) ) ;
#25804 = EDGE_LOOP ( 'NONE', ( #55998, #14623, #24369, #89650 ) ) ;
#25805 = AXIS2_PLACEMENT_3D ( 'NONE', #91335, #45675, #15214 ) ;
#25806 = CARTESIAN_POINT ( 'NONE',  ( -51.52287095715005449, -24.66019654487199375, 8.947790411086119278 ) ) ;
#25807 = CARTESIAN_POINT ( 'NONE',  ( -13.67433444753018534, -15.09191755960682890, 11.49999999999999645 ) ) ;
#25808 = DIRECTION ( 'NONE',  ( -0.000000000000000000, 1.000000000000000000, -0.000000000000000000 ) ) ;
#25809 = CC_DESIGN_DATE_AND_TIME_ASSIGNMENT ( #41538, #28796, ( #16578 ) ) ;
#25810 = CARTESIAN_POINT ( 'NONE',  ( -89.52287095715006160, -24.64898659630528854, 1.056161002820827921 ) ) ;
#25811 = ORIENTED_EDGE ( 'NONE', *, *, #93765, .F. ) ;
#25812 = CARTESIAN_POINT ( 'NONE',  ( -62.62287095715003460, -23.73907113216991505, -1.053371485793230811 ) ) ;
#25813 = CARTESIAN_POINT ( 'NONE',  ( -116.6228709571500275, -23.47596703998600631, 11.44779298504227860 ) ) ;
#25814 = FACE_OUTER_BOUND ( 'NONE', #28850, .T. ) ;
#25815 = AXIS2_PLACEMENT_3D ( 'NONE', #55801, #78596, #9607 ) ;
#25816 = CARTESIAN_POINT ( 'NONE',  ( -49.40320226356282518, -25.31439389004907525, 5.711994248101696314 ) ) ;
#25817 = DIRECTION ( 'NONE',  ( 0.000000000000000000, -1.000000000000000000, 0.000000000000000000 ) ) ;
#25818 = CARTESIAN_POINT ( 'NONE',  ( -109.6276325182596878, -24.15543982623907482, -0.2315651400026587092 ) ) ;
#25819 = ORIENTED_EDGE ( 'NONE', *, *, #84923, .T. ) ;
#25820 = CARTESIAN_POINT ( 'NONE',  ( -42.52287095715005449, -24.65952944569303895, 1.056160979905691910 ) ) ;
#25821 = CARTESIAN_POINT ( 'NONE',  ( 1.269710630819723463, 22.90746787927615102, 11.49999999999999645 ) ) ;
#25822 = CARTESIAN_POINT ( 'NONE',  ( 15.01325480956343483, 17.08929600257393489, 11.49999999999998934 ) ) ;
#25823 = CARTESIAN_POINT ( 'NONE',  ( 4.948291700218025113, -6.376774720514418959, 20.47145334051262111 ) ) ;
#25824 = CARTESIAN_POINT ( 'NONE',  ( 8.000000000000003553, -5.876774720514426953, 22.50000000000000355 ) ) ;
#25825 = CARTESIAN_POINT ( 'NONE',  ( -90.63103312429373659, -24.52300882791528380, 0.6510814631126311536 ) ) ;
#25826 = CARTESIAN_POINT ( 'NONE',  ( -54.62287095715005592, -23.48786465467240347, 11.44779295918255180 ) ) ;
#25827 = CARTESIAN_POINT ( 'NONE',  ( -6.542779104410481494, 20.88585256366161502, -1.500000000000002220 ) ) ;
#25828 = CARTESIAN_POINT ( 'NONE',  ( -69.54933722304251376, -24.15620529776627734, 10.23563542870660825 ) ) ;
#25829 = CARTESIAN_POINT ( 'NONE',  ( -27.12033265819623296, -24.75670803537512654, 2.403093704482753612 ) ) ;
#25830 = CARTESIAN_POINT ( 'NONE',  ( -54.52287095715008292, -23.72747288104469732, -1.053458166803227680 ) ) ;
#25831 = CARTESIAN_POINT ( 'NONE',  ( -58.61166247586906763, -23.48783264082476663, -1.443836473390093689 ) ) ;
#25832 = ORIENTED_EDGE ( 'NONE', *, *, #100331, .T. ) ;
#25833 = CARTESIAN_POINT ( 'NONE',  ( -14.48729221511043441, 14.40292172154154926, -1.500000000000002220 ) ) ;
#25834 = ORIENTED_EDGE ( 'NONE', *, *, #52682, .F. ) ;
#25835 = ORIENTED_EDGE ( 'NONE', *, *, #41905, .T. ) ;
#25836 = CARTESIAN_POINT ( 'NONE',  ( 5.527175565732886042, -22.34193536506064603, -1.500000000000002220 ) ) ;
#25837 = CARTESIAN_POINT ( 'NONE',  ( 32.76111974776238611, -3.316774720514426900, -3.850861272813261849 ) ) ;
#25838 = ORIENTED_EDGE ( 'NONE', *, *, #72044, .F. ) ;
#25839 = LINE ( 'NONE', #57810, #63960 ) ;
#25840 = PLANE ( 'NONE',  #35234 ) ;
#25841 = CARTESIAN_POINT ( 'NONE',  ( -122.5895376238167245, -24.66019654487200086, 8.947790411086115725 ) ) ;
#25842 = CARTESIAN_POINT ( 'NONE',  ( -118.3655821056664905, -25.21790522177258609, 6.461928009673355788 ) ) ;
#25844 = VERTEX_POINT ( 'NONE', #54960 ) ;
#25843 = CARTESIAN_POINT ( 'NONE',  ( -20.23222619987061677, -6.887663580918623296, 11.49999999999999645 ) ) ;
#25845 = EDGE_CURVE ( 'NONE', #33324, #27253, #62564, .T. ) ;
#25846 = ORIENTED_EDGE ( 'NONE', *, *, #61370, .F. ) ;
#25847 = CARTESIAN_POINT ( 'NONE',  ( 14.93699691249320693, 16.48547057857716425, -1.500000000000002220 ) ) ;
#25848 = ADVANCED_FACE ( 'NONE', ( #71184 ), #86399, .T. ) ;
#25849 = CARTESIAN_POINT ( 'NONE',  ( 0.1934390699377774303, 20.68474938276070318, 11.49999999999998934 ) ) ;
#25850 = PERSON ( 'NAUO-PER11', 'UNSPECIFIED', 'UNSPECIFIED', ('UNSPECIFIED'), ('UNSPECIFIED'), ('UNSPECIFIED') ) ;
#25851 = VERTEX_POINT ( 'NONE', #9267 ) ;
#25852 = LINE ( 'NONE', #10126, #41488 ) ;
#25853 = CARTESIAN_POINT ( 'NONE',  ( 3.160575456146155204, -5.876774720514408301, 18.86877352677795372 ) ) ;
#25854 = VERTEX_POINT ( 'NONE', #64600 ) ;
#25855 = CARTESIAN_POINT ( 'NONE',  ( -127.5562042904833930, -24.64898659630529920, 1.056161002820838579 ) ) ;
#25856 = VECTOR ( 'NONE', #69778, 1000.000000000000000 ) ;
#25857 = EDGE_LOOP ( 'NONE', ( #68533, #19639, #88742, #67272 ) ) ;
#25858 = CARTESIAN_POINT ( 'NONE',  ( 14.61581676225068449, 6.475225279485576912, -27.35847991880143226 ) ) ;
#25859 = B_SPLINE_CURVE_WITH_KNOTS ( 'NONE', 3,
 ( #27808, #28804, #20684, #28306 ),
 .UNSPECIFIED., .F., .F.,
 ( 4, 4 ),
 ( 0.000000000000000000, 9.999999999998206125E-05 ),
 .UNSPECIFIED. ) ;
#25860 = CARTESIAN_POINT ( 'NONE',  ( -71.27267509207285912, -25.21912432202341492, 6.451068343402560856 ) ) ;
#25861 = CARTESIAN_POINT ( 'NONE',  ( 2.299058169534009100, 20.76012671103276475, -1.500000000000002220 ) ) ;
#25862 = EDGE_CURVE ( 'NONE', #17845, #83405, #61136, .T. ) ;
#25863 = CARTESIAN_POINT ( 'NONE',  ( 17.34737195785526609, 13.27887811287985187, 11.49999999999999645 ) ) ;
#25864 = CARTESIAN_POINT ( 'NONE',  ( -73.63909330937920572, -23.96169478059713143, 10.65365249895718236 ) ) ;
#25865 = DIRECTION ( 'NONE',  ( -3.773278334453079030E-23, 0.9999999999976377785, 2.173523156925979128E-06 ) ) ;
#25866 = CARTESIAN_POINT ( 'NONE',  ( -21.16806448877717628, 7.570426553894726851, 11.49999999999998934 ) ) ;
#25867 = AXIS2_PLACEMENT_3D ( 'NONE', #8150, #528, #31479 ) ;
#25868 = CARTESIAN_POINT ( 'NONE',  ( -19.40224465947428456, -7.824916089261592766, 11.49999999999998934 ) ) ;
#25869 = CARTESIAN_POINT ( 'NONE',  ( -38.55293158061942194, -23.96119346886880663, -0.6495511937831989213 ) ) ;
#25870 = CARTESIAN_POINT ( 'NONE',  ( -52.58953762381673158, -24.66019654487199020, 8.947790411086131712 ) ) ;
#25871 = CARTESIAN_POINT ( 'NONE',  ( -126.5228709571500616, -24.66019654487200441, 8.947790411086108620 ) ) ;
#25872 = ORIENTED_EDGE ( 'NONE', *, *, #99520, .T. ) ;
#25873 = VECTOR ( 'NONE', #49070, 1000.000000000000000 ) ;
#25874 = ORIENTED_EDGE ( 'NONE', *, *, #93165, .F. ) ;
#25875 = VECTOR ( 'NONE', #91828, 1000.000000000000000 ) ;
#25876 = ORIENTED_EDGE ( 'NONE', *, *, #52998, .T. ) ;
#25877 = CARTESIAN_POINT ( 'NONE',  ( -28.98875734969026041, -5.965225279485572685, 23.37402280011862743 ) ) ;
#25878 = ORIENTED_EDGE ( 'NONE', *, *, #2009, .T. ) ;
#25879 = VECTOR ( 'NONE', #92626, 999.9999999999998863 ) ;
#25880 = CARTESIAN_POINT ( 'NONE',  ( 21.20698605602738951, -2.876969938318672870, -1.500000000000002220 ) ) ;
#25881 = CARTESIAN_POINT ( 'NONE',  ( -1.986123035288760885, 22.30159847666916662, 11.49999999999999645 ) ) ;
#25882 = VERTEX_POINT ( 'NONE', #79280 ) ;
#25883 = CARTESIAN_POINT ( 'NONE',  ( 0.3627416911114360598, -6.376774720514411854, 19.59793130852656873 ) ) ;
#25884 = CARTESIAN_POINT ( 'NONE',  ( 0.4554788648648982474, -21.05657754196055009, -1.500000000000002220 ) ) ;
#25885 = CARTESIAN_POINT ( 'NONE',  ( -30.51840328450298756, -23.78345446126201068, 10.97490056816818971 ) ) ;
#25886 = CARTESIAN_POINT ( 'NONE',  ( 18.73470368118781693, 6.836574088118649861, -1.500000000000002220 ) ) ;
#25887 = CARTESIAN_POINT ( 'NONE',  ( -50.48313689439709862, -24.73531770709094602, 8.716586749053508498 ) ) ;
#25888 = CARTESIAN_POINT ( 'NONE',  ( 29.73860345376316872, 5.356774720514427379, 17.30421508979850387 ) ) ;
#25889 = CARTESIAN_POINT ( 'NONE',  ( 20.91424602935089894, 6.983905699820807556, -1.500000000000002220 ) ) ;
#25890 = ORIENTED_EDGE ( 'NONE', *, *, #3414, .F. ) ;
#25891 = CARTESIAN_POINT ( 'NONE',  ( -116.5196432029274973, -23.96119346886881729, -0.6495511937831834892 ) ) ;
#25892 = PLANE ( 'NONE',  #61088 ) ;
#25893 = CARTESIAN_POINT ( 'NONE',  ( -41.02425807142757463, -25.27956050905338259, 5.449277030247038134 ) ) ;
#25894 = EDGE_CURVE ( 'NONE', #46787, #22811, #52853, .T. ) ;
#25895 = CARTESIAN_POINT ( 'NONE',  ( -47.52287095715007581, -23.94994826722564696, -0.6494450866342728057 ) ) ;
#25896 = DIRECTION ( 'NONE',  ( -0.000000000000000000, -1.000000000000000000, -0.000000000000000000 ) ) ;
#25897 = LINE ( 'NONE', #17789, #35136 ) ;
#25898 = CARTESIAN_POINT ( 'NONE',  ( -1.825377252022436281, -21.23478267787193730, -1.500000000000002220 ) ) ;
#25899 = CARTESIAN_POINT ( 'NONE',  ( -97.52287095715006160, -24.64898659630367916, 1.056161002820829697 ) ) ;
#25900 = DIRECTION ( 'NONE',  ( 0.000000000000000000, -0.9999999999976377785, -2.173523156925979128E-06 ) ) ;
#25901 = EDGE_CURVE ( 'NONE', #39794, #46605, #80539, .T. ) ;
#25902 = CARTESIAN_POINT ( 'NONE',  ( -32.22287095715006444, -23.47596703998600276, 11.44779298504227683 ) ) ;
#25903 = CARTESIAN_POINT ( 'NONE',  ( -107.6228709571500701, -29.50250243563736774, 8.947779886222136270 ) ) ;
#25904 = CARTESIAN_POINT ( 'NONE',  ( 15.88279217892459094, 16.07415641707351384, -1.500000000000002220 ) ) ;
#25905 = CARTESIAN_POINT ( 'NONE',  ( -81.52287095715006160, -24.64898659630367916, 1.056161002820826145 ) ) ;
#25906 = ORIENTED_EDGE ( 'NONE', *, *, #24045, .F. ) ;
#25907 = CARTESIAN_POINT ( 'NONE',  ( 4.653846153846159517, -5.876774720514419847, 19.99999999999999289 ) ) ;
#25908 = CARTESIAN_POINT ( 'NONE',  ( 2.903846153846159517, -6.376774720514415407, 19.99999999999999289 ) ) ;
#25909 = CARTESIAN_POINT ( 'NONE',  ( -11.90832679833862073, -15.64659449181510986, 11.49999999999999645 ) ) ;
#25910 = FACE_OUTER_BOUND ( 'NONE', #26228, .T. ) ;
#25911 = CARTESIAN_POINT ( 'NONE',  ( -67.64073392607424751, -23.96119346886880308, -0.6495511937832114668 ) ) ;
#25912 = ORIENTED_EDGE ( 'NONE', *, *, #29263, .F. ) ;
#25913 = CARTESIAN_POINT ( 'NONE',  ( 5.399550031317769339, -5.965225279485594001, -28.54570968858208246 ) ) ;
#25914 = FACE_OUTER_BOUND ( 'NONE', #82738, .T. ) ;
#25915 = CARTESIAN_POINT ( 'NONE',  ( -124.5563175255059605, -23.73791477778912551, 11.05961554403169878 ) ) ;
#25916 = FACE_OUTER_BOUND ( 'NONE', #63578, .T. ) ;
#25917 = CARTESIAN_POINT ( 'NONE',  ( -58.52287095715006160, -23.47596703998600631, 11.44779298504228926 ) ) ;
#25918 = B_SPLINE_CURVE_WITH_KNOTS ( 'NONE', 3,
 ( #18976, #3281, #40325, #40818 ),
 .UNSPECIFIED., .F., .F.,
 ( 4, 4 ),
 ( 0.5401716478292172274, 0.5491780791013332053 ),
 .UNSPECIFIED. ) ;
#25919 = CARTESIAN_POINT ( 'NONE',  ( 8.160000000000000142, 7.891155995661682354, 5.788828319098143105 ) ) ;
#25920 = CARTESIAN_POINT ( 'NONE',  ( -1.996473883165060581, 19.68112600131995293, 11.49999999999998934 ) ) ;
#25921 = EDGE_LOOP ( 'NONE', ( #27960, #96041, #51431, #26064 ) ) ;
#25922 = CARTESIAN_POINT ( 'NONE',  ( 3.569899647507075890, 19.86734082857295647, 11.49999999999999645 ) ) ;
#25923 = CARTESIAN_POINT ( 'NONE',  ( 5.641025641025643189, -5.876774720514419847, 20.78665865384615330 ) ) ;
#25924 = CIRCLE ( 'NONE', #59908, 1.500000000000000666 ) ;
#25925 = EDGE_CURVE ( 'NONE', #95782, #59162, #8105, .T. ) ;
#25926 = ORIENTED_EDGE ( 'NONE', *, *, #6222, .F. ) ;
#25927 = CARTESIAN_POINT ( 'NONE',  ( -52.58953762381672448, -24.65952944569304250, 1.056160979905697239 ) ) ;
#25928 = CARTESIAN_POINT ( 'NONE',  ( -65.55620429048339304, -23.48786465467240703, 11.44779295918254647 ) ) ;
#25929 = CARTESIAN_POINT ( 'NONE',  ( 8.160000000000000142, -9.123836073446797812, -2.666350264951732552 ) ) ;
#25930 = DIRECTION ( 'NONE',  ( 0.02119372647573786531, -9.594337693711052596E-15, 0.9997753877537052247 ) ) ;
#25931 = AXIS2_PLACEMENT_3D ( 'NONE', #73764, #4759, #74267 ) ;
#25932 = CARTESIAN_POINT ( 'NONE',  ( -62.52287095715006160, -23.48786465467241058, 11.44779295918254824 ) ) ;
#25933 = CARTESIAN_POINT ( 'NONE',  ( -120.5895376238167245, -23.48786465467241769, 11.44779295918253759 ) ) ;
#25934 = CARTESIAN_POINT ( 'NONE',  ( 19.36564117097816862, 5.170944958934900804, 11.49999999999998934 ) ) ;
#25935 = CARTESIAN_POINT ( 'NONE',  ( -34.52287095715006160, -24.64898659630366851, 1.056161002820817485 ) ) ;
#25936 = ORIENTED_EDGE ( 'NONE', *, *, #96604, .F. ) ;
#25937 = ADVANCED_FACE ( 'NONE', ( #3678 ), #56972, .F. ) ;
#25938 = CIRCLE ( 'NONE', #71282, 0.8160000000000000586 ) ;
#25939 = AXIS2_PLACEMENT_3D ( 'NONE', #16619, #30852, #69417 ) ;
#25940 = CARTESIAN_POINT ( 'NONE',  ( -51.52287095715009002, -23.48783264082477018, -1.443836473390092578 ) ) ;
#25941 = CARTESIAN_POINT ( 'NONE',  ( -35.52138534232717859, -24.92564183028978775, 1.928384488918258199 ) ) ;
#25942 = CARTESIAN_POINT ( 'NONE',  ( -80.43221577628075636, -25.30553498687082481, 4.967019777649441359 ) ) ;
#25943 = CIRCLE ( 'NONE', #58410, 18.50000000000000355 ) ;
#25944 = DIRECTION ( 'NONE',  ( -0.000000000000000000, 1.000000000000000000, -0.000000000000000000 ) ) ;
#25945 = CARTESIAN_POINT ( 'NONE',  ( -103.5228709571501042, -23.48783264082477018, -1.443836473390087916 ) ) ;
#25946 = AXIS2_PLACEMENT_3D ( 'NONE', #45374, #76291, #15393 ) ;
#25947 = PLANE ( 'NONE',  #54358 ) ;
#25948 = DIRECTION ( 'NONE',  ( 0.000000000000000000, 0.9513357669802769978, -0.3081562241202473462 ) ) ;
#25949 = VERTEX_POINT ( 'NONE', #73188 ) ;
#25950 = CARTESIAN_POINT ( 'NONE',  ( 12.41260344771940360, 16.11316662856288318, -1.500000000000002220 ) ) ;
#25951 = ORIENTED_EDGE ( 'NONE', *, *, #52994, .F. ) ;
#25952 = EDGE_CURVE ( 'NONE', #47563, #65800, #97013, .T. ) ;
#25953 = DIRECTION ( 'NONE',  ( 1.700709290173338723E-14, 0.000000000000000000, 1.000000000000000000 ) ) ;
#25954 = CARTESIAN_POINT ( 'NONE',  ( -127.5896351818574459, -24.35071581493543746, 9.817618358456011052 ) ) ;
#25955 = ORIENTED_EDGE ( 'NONE', *, *, #79716, .T. ) ;
#25956 = CARTESIAN_POINT ( 'NONE',  ( -59.64911270062432891, -23.73791477778911840, 11.05961554403171299 ) ) ;
#25957 = CARTESIAN_POINT ( 'NONE',  ( -49.84148113843717454, -25.26264154704761111, 6.992077779497625656 ) ) ;
#25958 = CARTESIAN_POINT ( 'NONE',  ( -30.47287095715006799, -24.99299043464974091, 2.200638162335478487 ) ) ;
#25959 = CARTESIAN_POINT ( 'NONE',  ( 19.97935793590388442, -6.945280299276400449, 11.49999999999999645 ) ) ;
#25960 = CARTESIAN_POINT ( 'NONE',  ( 21.88104185797606505, 3.448541436957560880, 11.49999999999998934 ) ) ;
#25961 = EDGE_CURVE ( 'NONE', #46475, #80523, #89164, .T. ) ;
#25962 = CARTESIAN_POINT ( 'NONE',  ( -4.563637348303267949, -20.04915943051449645, -1.500000000000002220 ) ) ;
#25963 = ORIENTED_EDGE ( 'NONE', *, *, #50384, .F. ) ;
#25964 = CARTESIAN_POINT ( 'NONE',  ( -41.58133722831164647, -24.51314013834315375, 0.6176544820404115121 ) ) ;
#25965 = VERTEX_POINT ( 'NONE', #49864 ) ;
#25966 = ADVANCED_FACE ( 'NONE', ( #10783 ), #42257, .F. ) ;
#25967 = CARTESIAN_POINT ( 'NONE',  ( -54.59888152181910215, -23.96119346886879953, -0.6495511937832153526 ) ) ;
#25968 = CARTESIAN_POINT ( 'NONE',  ( -110.6228709571500701, -24.92604778743018912, 8.074972756849355449 ) ) ;
#25969 = ORIENTED_EDGE ( 'NONE', *, *, #33415, .T. ) ;
#25970 = ORIENTED_EDGE ( 'NONE', *, *, #7671, .T. ) ;
#25971 = VERTEX_POINT ( 'NONE', #28004 ) ;
#25972 = CARTESIAN_POINT ( 'NONE',  ( -81.62287095715008434, -23.47596703998600631, 11.44779298504227860 ) ) ;
#25973 = CARTESIAN_POINT ( 'NONE',  ( 7.052174998393318184, -6.376774720514418959, 20.39928653130861136 ) ) ;
#25974 = CARTESIAN_POINT ( 'NONE',  ( 5.400898774349120579, -6.376774720514417183, 20.36357656736558042 ) ) ;
#25975 = CARTESIAN_POINT ( 'NONE',  ( 7.914317726235799100, 19.11507755054979896, -1.500000000000002220 ) ) ;
#25976 = EDGE_CURVE ( 'NONE', #74588, #91432, #49775, .T. ) ;
#25977 = CARTESIAN_POINT ( 'NONE',  ( 16.53012286974688294, -13.99140274789385252, 11.49999999999999645 ) ) ;
#25978 = ORIENTED_EDGE ( 'NONE', *, *, #28875, .F. ) ;
#25979 = CARTESIAN_POINT ( 'NONE',  ( -69.55126625704998844, -25.16221347177320666, 3.076695569926833684 ) ) ;
#25980 = CARTESIAN_POINT ( 'NONE',  ( -111.2965753446675450, -25.17176379221491800, 3.202224473218894030 ) ) ;
#25981 = CARTESIAN_POINT ( 'NONE',  ( 0.2029947971921062799, -22.41465419638480228, 11.49999999999998934 ) ) ;
#25982 = EDGE_CURVE ( 'NONE', #57364, #56711, #2001, .T. ) ;
#25983 = DIRECTION ( 'NONE',  ( 0.000000000000000000, 1.478457507934778393E-16, -1.000000000000000000 ) ) ;
#25984 = DIRECTION ( 'NONE',  ( 0.000000000000000000, 0.000000000000000000, -1.000000000000000000 ) ) ;
#25985 = ORIENTED_EDGE ( 'NONE', *, *, #216, .T. ) ;
#25986 = DIRECTION ( 'NONE',  ( -0.000000000000000000, -1.000000000000000000, -0.000000000000000000 ) ) ;
#25987 = CARTESIAN_POINT ( 'NONE',  ( -35.53214346113144728, -24.63419186844611630, 9.035850630976925757 ) ) ;
#25988 = EDGE_LOOP ( 'NONE', ( #72082, #29524, #24562, #8615 ) ) ;
#25989 = ORIENTED_EDGE ( 'NONE', *, *, #13634, .T. ) ;
#25990 = AXIS2_PLACEMENT_3D ( 'NONE', #79375, #2775, #56061 ) ;
#25991 = CARTESIAN_POINT ( 'NONE',  ( -46.58712800869141546, -24.35071581493542325, 9.817618358456032368 ) ) ;
#25992 = VERTEX_POINT ( 'NONE', #43732 ) ;
#25993 = FACE_OUTER_BOUND ( 'NONE', #70420, .T. ) ;
#25994 = CARTESIAN_POINT ( 'NONE',  ( 20.00388196354723291, 7.160935007556333609, -1.500000000000002220 ) ) ;
#25995 = ORIENTED_EDGE ( 'NONE', *, *, #98934, .T. ) ;
#25996 = CARTESIAN_POINT ( 'NONE',  ( -88.63497506943951976, -23.96119346886881019, -0.6495511937832099125 ) ) ;
#25997 = CARTESIAN_POINT ( 'NONE',  ( 3.468383421097696928, -21.53508805063734854, 11.49999999999998934 ) ) ;
#25998 = CARTESIAN_POINT ( 'NONE',  ( -103.5221972247327784, -23.48786465467241058, 11.44779295918254292 ) ) ;
#25999 = CARTESIAN_POINT ( 'NONE',  ( -51.62287095715005592, -29.50247984919015209, -1.443849546365058689 ) ) ;
#26000 = CARTESIAN_POINT ( 'NONE',  ( 5.344006250707635353, -5.876774720514418959, 20.55781796641452885 ) ) ;
#26001 = CARTESIAN_POINT ( 'NONE',  ( 17.34737195785526609, 13.27887811287985187, -1.500000000000002220 ) ) ;
#26002 = LINE ( 'NONE', #96513, #83604 ) ;
#26003 = ORIENTED_EDGE ( 'NONE', *, *, #96759, .T. ) ;
#26004 = CARTESIAN_POINT ( 'NONE',  ( -89.62287095715004170, -24.64965695001468404, 8.947790433994180503 ) ) ;
#26005 = CARTESIAN_POINT ( 'NONE',  ( -48.91945971812886995, -25.26337384518503271, 6.515678376904751268 ) ) ;
#26006 = EDGE_LOOP ( 'NONE', ( #33712, #58550, #99546, #9330 ) ) ;
#26007 = CARTESIAN_POINT ( 'NONE',  ( 27.86270917940689174, -6.376774720514426953, 29.02104833056109001 ) ) ;
#26008 = VECTOR ( 'NONE', #93268, 1000.000000000000000 ) ;
#26009 = ORIENTED_EDGE ( 'NONE', *, *, #63900, .F. ) ;
#26010 = CARTESIAN_POINT ( 'NONE',  ( -128.5895376238167103, -23.47596703998600631, 11.44779298504227683 ) ) ;
#26011 = AXIS2_PLACEMENT_3D ( 'NONE', #32684, #79856, #96098 ) ;
#26012 = DIRECTION ( 'NONE',  ( 0.000000000000000000, 0.000000000000000000, -1.000000000000000000 ) ) ;
#26013 = CARTESIAN_POINT ( 'NONE',  ( 12.23393567461250697, 17.36540613969008007, -1.500000000000002220 ) ) ;
#26014 = LINE ( 'NONE', #87412, #54731 ) ;
#26015 = CARTESIAN_POINT ( 'NONE',  ( -30.59167141582165783, -24.92410949913933038, 1.600845668900849672 ) ) ;
#26016 = FACE_OUTER_BOUND ( 'NONE', #29825, .T. ) ;
#26017 = CARTESIAN_POINT ( 'NONE',  ( -68.58036413909906059, -24.65952944569304606, 1.056160979905701236 ) ) ;
#26018 = VECTOR ( 'NONE', #66496, 1000.000000000000000 ) ;
#26019 = CARTESIAN_POINT ( 'NONE',  ( -7.106217341473486826, 18.08270997100935418, 11.49999999999998934 ) ) ;
#26020 = EDGE_CURVE ( 'NONE', #68431, #76612, #42746, .T. ) ;
#26021 = CARTESIAN_POINT ( 'NONE',  ( -93.62287095715005592, -29.50248528299804818, 1.056150453629040253 ) ) ;
#26022 = ORIENTED_EDGE ( 'NONE', *, *, #70527, .F. ) ;
#26023 = CARTESIAN_POINT ( 'NONE',  ( 6.966380261627926451, -18.21767524041069564, 11.49999999999999645 ) ) ;
#26024 = DIRECTION ( 'NONE',  ( 0.000000000000000000, 0.000000000000000000, -1.000000000000000000 ) ) ;
#26025 = FACE_OUTER_BOUND ( 'NONE', #91994, .T. ) ;
#26026 = ORIENTED_EDGE ( 'NONE', *, *, #41579, .T. ) ;
#26027 = CARTESIAN_POINT ( 'NONE',  ( 4.689770114687411784, -5.876774720514423400, 21.33175327469028915 ) ) ;
#26028 = CARTESIAN_POINT ( 'NONE',  ( -75.62287095715005592, -23.48783264082478084, -1.443836473390065489 ) ) ;
#26029 = CARTESIAN_POINT ( 'NONE',  ( 0.8126045299064811323, -1.450440077808301975, 8.999999999999998224 ) ) ;
#26030 = CARTESIAN_POINT ( 'NONE',  ( -81.23841534186585989, -25.03156017793848420, 7.364952925001797546 ) ) ;
#26031 = CARTESIAN_POINT ( 'NONE',  ( -16.08770303010339831, 11.32657509950784736, 11.49999999999998934 ) ) ;
#26032 = VERTEX_POINT ( 'NONE', #50850 ) ;
#26033 = CYLINDRICAL_SURFACE ( 'NONE', #45646, 18.50000000000000000 ) ;
#26034 = CARTESIAN_POINT ( 'NONE',  ( 21.72910700495702230, 7.846448622349001312, -1.500000000000002220 ) ) ;
#26035 = ADVANCED_FACE ( 'NONE', ( #96016 ), #66096, .T. ) ;
#26036 = APPROVAL_STATUS ( 'not_yet_approved' ) ;
#26037 = ORIENTED_EDGE ( 'NONE', *, *, #89908, .T. ) ;
#26038 = CARTESIAN_POINT ( 'NONE',  ( -108.5228709571500616, -29.50250243563736774, 8.947779886222136270 ) ) ;
#26039 = CARTESIAN_POINT ( 'NONE',  ( -51.52287095715008292, -23.47593901973090169, -1.443836447538997092 ) ) ;
#26040 = DIRECTION ( 'NONE',  ( -1.000000000000000000, -0.000000000000000000, -0.000000000000000000 ) ) ;
#26041 = CARTESIAN_POINT ( 'NONE',  ( -97.59657388994536120, -23.73791477778912196, 11.05961554403170410 ) ) ;
#26043 = EDGE_CURVE ( 'NONE', #76027, #12135, #74178, .T. ) ;
#26042 = CARTESIAN_POINT ( 'NONE',  ( -78.92547529514705218, -25.27183487616304447, 3.712349674769177543 ) ) ;
#26044 = CARTESIAN_POINT ( 'NONE',  ( -69.38261850605717029, -25.31201727726708128, 5.944601339124433004 ) ) ;
#26045 = B_SPLINE_CURVE_WITH_KNOTS ( 'NONE', 3,
 ( #84723, #69002, #17213, #92331 ),
 .UNSPECIFIED., .F., .F.,
 ( 4, 4 ),
 ( 1.788112030672749005E-18, 0.0002127494369525745788 ),
 .UNSPECIFIED. ) ;
#26046 = LINE ( 'NONE', #95064, #47802 ) ;
#26047 = CARTESIAN_POINT ( 'NONE',  ( -1.345660788846553935, -19.86331345790170033, 11.49999999999998934 ) ) ;
#26048 = CARTESIAN_POINT ( 'NONE',  ( -75.64171577028287174, -24.15602025860895807, 10.28564288303536678 ) ) ;
#26049 = CARTESIAN_POINT ( 'NONE',  ( 2.793900936927258272, 19.68708943014846469, -1.500000000000002220 ) ) ;
#26050 = ORIENTED_EDGE ( 'NONE', *, *, #67258, .T. ) ;
#26051 = ADVANCED_FACE ( 'NONE', ( #66597 ), #97509, .F. ) ;
#26052 = PLANE ( 'NONE',  #16730 ) ;
#26053 = EDGE_CURVE ( 'NONE', #30745, #92987, #99986, .T. ) ;
#26054 = EDGE_CURVE ( 'NONE', #54341, #46190, #91463, .T. ) ;
#26055 = CARTESIAN_POINT ( 'NONE',  ( -104.6228709571500985, -24.50321055353805377, 9.387540953477529371 ) ) ;
#26056 = CARTESIAN_POINT ( 'NONE',  ( -29.52287095715007226, -23.87625476476128128, 10.65359472914277816 ) ) ;
#26057 = CARTESIAN_POINT ( 'NONE',  ( -80.49261886157198376, -25.00182538069146787, 7.747789668545041586 ) ) ;
#26058 = CARTESIAN_POINT ( 'NONE',  ( 0.4431998670617953717, 20.78131286043265646, 11.49999999999999645 ) ) ;
#26059 = CARTESIAN_POINT ( 'NONE',  ( -7.421417143192116761, -5.876774720514411854, 19.43823095447975291 ) ) ;
#26060 = CIRCLE ( 'NONE', #34183, 3.060000000000001830 ) ;
#26061 = CARTESIAN_POINT ( 'NONE',  ( -51.08354598259256107, -25.21593214439643305, 3.527498281770244493 ) ) ;
#26062 = B_SPLINE_CURVE_WITH_KNOTS ( 'NONE', 3,
 ( #59965, #37107, #60959, #91884, #82779, #7149, #61458, #90400 ),
 .UNSPECIFIED., .F., .F.,
 ( 4, 2, 2, 4 ),
 ( 0.06220205793350375156, 0.06492579111525004221, 0.06628765770612317365, 0.06764952429699631897 ),
 .UNSPECIFIED. ) ;
#26063 = CARTESIAN_POINT ( 'NONE',  ( -21.74551633039419585, 6.958787177381512201, 11.49999999999999645 ) ) ;
#26064 = ORIENTED_EDGE ( 'NONE', *, *, #87184, .F. ) ;
#26065 = CARTESIAN_POINT ( 'NONE',  ( -108.5895376238167387, -24.64965694238407679, 8.947790433994649462 ) ) ;
#26066 = CARTESIAN_POINT ( 'NONE',  ( -84.62287095715008434, -23.47596703998600631, 11.44779298504227860 ) ) ;
#26067 = VERTEX_POINT ( 'NONE', #6154 ) ;
#26068 = CARTESIAN_POINT ( 'NONE',  ( -16.41926757845921614, -11.79510067912178606, -1.500000000000002220 ) ) ;
#26069 = ADVANCED_FACE ( 'NONE', ( #67083 ), #97993, .T. ) ;
#26070 = CARTESIAN_POINT ( 'NONE',  ( 7.176111537430461595, -5.876774720514424288, 21.53668079471899333 ) ) ;
#26071 = CARTESIAN_POINT ( 'NONE',  ( 5.949073730962466833, 5.965225279485572685, -27.94053387008862188 ) ) ;
#26072 = DIRECTION ( 'NONE',  ( -0.3133898629642195011, -5.365801633547207373E-16, 0.9496245541219264785 ) ) ;
#26073 = EDGE_LOOP ( 'NONE', ( #64954, #73440, #41813, #24269 ) ) ;
#26074 = CARTESIAN_POINT ( 'NONE',  ( -70.62287095715008434, -24.82576562982391977, 8.398263435472967942 ) ) ;
#26075 = CARTESIAN_POINT ( 'NONE',  ( -10.15655021453082263, 4.851073166933324465, 30.10912256999369774 ) ) ;
#26076 = CIRCLE ( 'NONE', #60069, 3.349999999999998757 ) ;
#26077 = CARTESIAN_POINT ( 'NONE',  ( 19.86090765050778728, -2.328952942160339212, -1.500000000000002220 ) ) ;
#26078 = CARTESIAN_POINT ( 'NONE',  ( 7.117523389609132778, 19.69228268689324324, 11.49999999999999645 ) ) ;
#26079 = VECTOR ( 'NONE', #25721, 1000.000000000000114 ) ;
#26080 = CARTESIAN_POINT ( 'NONE',  ( -54.62287095715004170, -24.51387760970723662, 9.387446482453421837 ) ) ;
#26081 = CARTESIAN_POINT ( 'NONE',  ( -93.52287095715006160, -24.51387760970725083, 9.387446482453398744 ) ) ;
#26082 = CARTESIAN_POINT ( 'NONE',  ( 7.103389721457689099, 20.86620700561973862, -1.500000000000002220 ) ) ;
#26083 = EDGE_CURVE ( 'NONE', #86142, #10167, #60468, .T. ) ;
#26084 = CARTESIAN_POINT ( 'NONE',  ( -39.93582354980947002, -25.27806084964504407, 4.982375622346077115 ) ) ;
#26085 = ORIENTED_EDGE ( 'NONE', *, *, #46920, .F. ) ;
#26086 = CARTESIAN_POINT ( 'NONE',  ( -60.52287095715007581, -24.82558206586143612, 1.605769216559444379 ) ) ;
#26087 = CYLINDRICAL_SURFACE ( 'NONE', #97888, 6.000000000000000888 ) ;
#26088 = EDGE_CURVE ( 'NONE', #58916, #31553, #26062, .T. ) ;
#26089 = CARTESIAN_POINT ( 'NONE',  ( -8.749999999999767297, 18.74999999999999645, 2.100000000000000089 ) ) ;
#26090 = VERTEX_POINT ( 'NONE', #20875 ) ;
#26091 = CARTESIAN_POINT ( 'NONE',  ( 3.116263380642223968, -6.376774720514401196, 18.40799819116699609 ) ) ;
#26092 = VERTEX_POINT ( 'NONE', #13261 ) ;
#26093 = ORIENTED_EDGE ( 'NONE', *, *, #34767, .F. ) ;
#26094 = DIRECTION ( 'NONE',  ( 0.09824042138329625029, 2.980407940728111021E-17, -0.9951627101165079203 ) ) ;
#26095 = CARTESIAN_POINT ( 'NONE',  ( -100.7878122855614293, -25.27404639244512907, 2.873139757414048479 ) ) ;
#26096 = CARTESIAN_POINT ( 'NONE',  ( -110.5228709571500616, -29.50249982740957577, 7.747779886224967605 ) ) ;
#26097 = CARTESIAN_POINT ( 'NONE',  ( -9.284664653622879626, 18.31210316397345395, -1.500000000000002220 ) ) ;
#26098 = B_SPLINE_CURVE_WITH_KNOTS ( 'NONE', 3,
 ( #74383, #57190, #26716, #95728, #57677, #80498 ),
 .UNSPECIFIED., .F., .F.,
 ( 4, 2, 4 ),
 ( 0.000000000000000000, 0.001380901958385393966, 0.002761803916770787931 ),
 .UNSPECIFIED. ) ;
#26099 = EDGE_CURVE ( 'NONE', #63660, #37998, #84774, .T. ) ;
#26100 = ORIENTED_EDGE ( 'NONE', *, *, #39779, .F. ) ;
#26101 = DIRECTION ( 'NONE',  ( 1.000000000000000000, 0.000000000000000000, 1.084136044942898696E-16 ) ) ;
#26102 = CARTESIAN_POINT ( 'NONE',  ( -102.6228709571500559, -24.65952944569304606, 1.056160979905702124 ) ) ;
#26103 = DIRECTION ( 'NONE',  ( -1.000000000000000000, -0.000000000000000000, -0.000000000000000000 ) ) ;
#26104 = CARTESIAN_POINT ( 'NONE',  ( -7.907391756136429528, -20.87048397725295956, -1.500000000000002220 ) ) ;
#26105 = EDGE_CURVE ( 'NONE', #65645, #93691, #51846, .T. ) ;
#26106 = CARTESIAN_POINT ( 'NONE',  ( -0.1490770655183801252, -21.12008023607309681, -1.443836447538997758 ) ) ;
#26107 = CARTESIAN_POINT ( 'NONE',  ( -113.5228709571500616, -23.47596703998600631, 11.44779298504228038 ) ) ;
#26108 = EDGE_LOOP ( 'NONE', ( #9595, #82987, #13183, #28303 ) ) ;
#26109 = EDGE_CURVE ( 'NONE', #63576, #73782, #22856, .T. ) ;
#26110 = CARTESIAN_POINT ( 'NONE',  ( -32.62287095715005592, -24.33927499327854704, 9.819080762295817166 ) ) ;
#26111 = PLANE ( 'NONE',  #32934 ) ;
#26112 = CARTESIAN_POINT ( 'NONE',  ( -9.832896139050584239, -18.40278743011522877, 11.49999999999998934 ) ) ;
#26113 = ORIENTED_EDGE ( 'NONE', *, *, #50598, .T. ) ;
#26115 = ORIENTED_EDGE ( 'NONE', *, *, #93991, .F. ) ;
#26114 = CARTESIAN_POINT ( 'NONE',  ( -0.08860454909227881426, -6.376774720514410077, 19.21747685089457036 ) ) ;
#26116 = EDGE_LOOP ( 'NONE', ( #80142, #88906, #50717, #67035 ) ) ;
#26118 = ADVANCED_FACE ( 'NONE', ( #36607 ), #14255, .T. ) ;
#26117 = CARTESIAN_POINT ( 'NONE',  ( 27.53860345374808105, 5.356774720514427379, 1.647607965253217399 ) ) ;
#26119 = CARTESIAN_POINT ( 'NONE',  ( 2.700122536338566359, 20.86363338933649558, -1.500000000000002220 ) ) ;
#26120 = ORIENTED_EDGE ( 'NONE', *, *, #94255, .T. ) ;
#26121 = CARTESIAN_POINT ( 'NONE',  ( -114.6228709571500275, -24.33927499327855060, 9.819080762295804732 ) ) ;
#26122 = DIRECTION ( 'NONE',  ( 0.000000000000000000, -1.000000000000000000, 0.000000000000000000 ) ) ;
#26123 = CARTESIAN_POINT ( 'NONE',  ( -120.6241460807069075, -24.83644354573579349, 8.397322867130096569 ) ) ;
#26124 = CARTESIAN_POINT ( 'NONE',  ( -101.2262178754702120, -25.25419513428566987, 7.375460839105605793 ) ) ;
#26125 = CARTESIAN_POINT ( 'NONE',  ( -36.58953762381673158, -24.65952944569304250, 1.056160979905695019 ) ) ;
#26126 = CARTESIAN_POINT ( 'NONE',  ( -10.04279811845843007, 19.21892966915218892, -1.500000000000002220 ) ) ;
#26127 = CARTESIAN_POINT ( 'NONE',  ( 0.000000000000000000, -5.876774720514426953, 0.000000000000000000 ) ) ;
#26129 = ORIENTED_EDGE ( 'NONE', *, *, #84145, .T. ) ;
#26128 = CARTESIAN_POINT ( 'NONE',  ( -21.31523168734759466, -6.469442287714795015, 11.49999999999999645 ) ) ;
#26130 = CARTESIAN_POINT ( 'NONE',  ( -72.62287095715004170, -23.96177878511307568, 10.65340807706330217 ) ) ;
#26131 = DIRECTION ( 'NONE',  ( 3.773278334444167608E-23, -1.000000000000000000, 0.000000000000000000 ) ) ;
#26132 = CARTESIAN_POINT ( 'NONE',  ( -75.52287095715007581, -29.50250786944525672, 11.44777988621623521 ) ) ;
#26133 = EDGE_LOOP ( 'NONE', ( #12229, #78219, #31940, #23221 ) ) ;
#26135 = ORIENTED_EDGE ( 'NONE', *, *, #9917, .F. ) ;
#26134 = CARTESIAN_POINT ( 'NONE',  ( -65.05438548721848235, 6.475225279485573360, 29.49402280011861777 ) ) ;
#26136 = ORIENTED_EDGE ( 'NONE', *, *, #5582, .F. ) ;
#26137 = CARTESIAN_POINT ( 'NONE',  ( -86.52287095715006160, -24.64965694238575011, 8.947790433994196491 ) ) ;
#26138 = VECTOR ( 'NONE', #71983, 1000.000000000000114 ) ;
#26139 = CARTESIAN_POINT ( 'NONE',  ( 31.53822845103994865, 4.132774720514425404, -2.786383594989611634 ) ) ;
#26140 = LINE ( 'NONE', #2819, #29503 ) ;
#26141 = ORIENTED_EDGE ( 'NONE', *, *, #95020, .T. ) ;
#26142 = CARTESIAN_POINT ( 'NONE',  ( -130.5728709571500588, -24.25872324547561831, -0.2236092734016485173 ) ) ;
#26143 = CARTESIAN_POINT ( 'NONE',  ( 8.126467401150291536, 20.86698325809501497, -1.500000000000002220 ) ) ;
#26144 = B_SPLINE_CURVE_WITH_KNOTS ( 'NONE', 3,
 ( #90851, #22816, #38059, #92839, #31450, #14212 ),
 .UNSPECIFIED., .F., .F.,
 ( 4, 2, 4 ),
 ( 0.000000000000000000, 0.001380901958385390930, 0.002761803916770781860 ),
 .UNSPECIFIED. ) ;
#26145 = ORIENTED_EDGE ( 'NONE', *, *, #33154, .F. ) ;
#26146 = ORIENTED_EDGE ( 'NONE', *, *, #42404, .T. ) ;
#26147 = LINE ( 'NONE', #72837, #41753 ) ;
#26148 = CARTESIAN_POINT ( 'NONE',  ( -101.5985644930808007, -23.48786465467240703, 11.44779295918254114 ) ) ;
#26149 = CARTESIAN_POINT ( 'NONE',  ( -61.52287095715007581, -24.33927499327854349, 9.819080762295813614 ) ) ;
#26150 = DIRECTION ( 'NONE',  ( 1.000000000000000000, 0.000000000000000000, 0.000000000000000000 ) ) ;
#26151 = CARTESIAN_POINT ( 'NONE',  ( -30.60521428952115741, -24.47917135695840685, 9.440663514584130667 ) ) ;
#26152 = VECTOR ( 'NONE', #31147, 1000.000000000000000 ) ;
#26153 = CARTESIAN_POINT ( 'NONE',  ( -16.94305004876727239, 9.801747318927828800, 11.49999999999998934 ) ) ;
#26154 = CARTESIAN_POINT ( 'NONE',  ( -49.56549000277595241, -25.29186519241541831, 4.241630633777523585 ) ) ;
#26156 = ORIENTED_EDGE ( 'NONE', *, *, #24334, .F. ) ;
#26155 = AXIS2_PLACEMENT_3D ( 'NONE', #2458, #19659, #71976 ) ;
#26157 = CARTESIAN_POINT ( 'NONE',  ( -20.54356019850136050, 6.435454313062578535, 11.49999999999998934 ) ) ;
#26158 = LINE ( 'NONE', #97172, #85208 ) ;
#26159 = CARTESIAN_POINT ( 'NONE',  ( -71.14319566529317740, -25.12219058256228266, 6.703707996014909298 ) ) ;
#26160 = CARTESIAN_POINT ( 'NONE',  ( -100.4381051993576364, -25.12049752546738191, 2.832404795212222215 ) ) ;
#26161 = DIRECTION ( 'NONE',  ( 0.000000000000000000, 1.000000000000000000, 0.000000000000000000 ) ) ;
#26162 = CARTESIAN_POINT ( 'NONE',  ( 19.00551534866085746, 12.86435971046890359, -1.500000000000002220 ) ) ;
#26163 = EDGE_CURVE ( 'NONE', #96476, #41375, #53843, .T. ) ;
#26164 = COORDINATED_UNIVERSAL_TIME_OFFSET ( 0, 0, .AHEAD. ) ;
#26165 = LINE ( 'NONE', #26674, #28843 ) ;
#26166 = CARTESIAN_POINT ( 'NONE',  ( -49.59948389210610742, -23.96119346886879953, -0.6495511937832114668 ) ) ;
#26167 = CARTESIAN_POINT ( 'NONE',  ( 3.315226082619958881, 19.80964767386612380, 11.49999999999999645 ) ) ;
#26168 = DIRECTION ( 'NONE',  ( -1.000000000000000000, 0.000000000000000000, 0.000000000000000000 ) ) ;
#26169 = CARTESIAN_POINT ( 'NONE',  ( -31.52287095715007581, -23.73907113217667231, -1.053371485781312344 ) ) ;
#26170 = EDGE_CURVE ( 'NONE', #11739, #64035, #45494, .T. ) ;
#26171 = DIRECTION ( 'NONE',  ( 0.000000000000000000, 0.9999999999976377785, 2.173523156925979975E-06 ) ) ;
#26172 = CARTESIAN_POINT ( 'NONE',  ( -65.62287095715008434, -24.62226745350439217, 0.9660975649728189563 ) ) ;
#26173 = PLANE ( 'NONE',  #65650 ) ;
#26174 = CARTESIAN_POINT ( 'NONE',  ( 1.158388978951967463, 19.79969207489630634, 11.49999999999998934 ) ) ;
#26175 = EDGE_CURVE ( 'NONE', #51553, #79008, #83027, .T. ) ;
#26176 = CARTESIAN_POINT ( 'NONE',  ( -90.62287095715009855, -24.15516710230295061, 10.28746687063727450 ) ) ;
#26177 = CARTESIAN_POINT ( 'NONE',  ( -19.50520112914412252, -2.896358124273927359, -1.500000000000002220 ) ) ;
#26178 = ADVANCED_FACE ( 'NONE', ( #75653 ), #29484, .F. ) ;
#26179 = CARTESIAN_POINT ( 'NONE',  ( -89.49044894935767047, -25.12049752546738191, 2.832404795212222659 ) ) ;
#26180 = EDGE_CURVE ( 'NONE', #66017, #59957, #6653, .T. ) ;
#26181 = FACE_OUTER_BOUND ( 'NONE', #67843, .T. ) ;
#26182 = DATE_AND_TIME ( #65278, #60427 ) ;
#26183 = ADVANCED_FACE ( 'NONE', ( #14755 ), #82344, .T. ) ;
#26184 = FACE_OUTER_BOUND ( 'NONE', #44448, .T. ) ;
#26185 = CARTESIAN_POINT ( 'NONE',  ( 15.92621150404962371, -5.965225279485572685, -27.29681269571043245 ) ) ;
#26186 = CARTESIAN_POINT ( 'NONE',  ( -16.41017380093149214, -12.48182641202616416, 11.49999999999999645 ) ) ;
#26187 = B_SPLINE_CURVE_WITH_KNOTS ( 'NONE', 3,
 ( #36694, #29074, #60049, #90976, #83356, #6235 ),
 .UNSPECIFIED., .F., .F.,
 ( 4, 2, 4 ),
 ( 0.000000000000000000, 0.0005049716539041804782, 0.001009943307808368112 ),
 .UNSPECIFIED. ) ;
#26188 = CARTESIAN_POINT ( 'NONE',  ( -9.940598223437577374, -5.876774720514426953, 17.91871304725684766 ) ) ;
#26189 = CARTESIAN_POINT ( 'NONE',  ( 18.14931799402153345, 13.46472642042223633, 11.49999999999999645 ) ) ;
#26190 = AXIS2_PLACEMENT_3D ( 'NONE', #99611, #87787, #49242 ) ;
#26191 = ORIENTED_EDGE ( 'NONE', *, *, #63336, .T. ) ;
#26192 = CARTESIAN_POINT ( 'NONE',  ( -126.5228709571500616, -23.47593901973090524, -1.443836447538996204 ) ) ;
#26193 = CARTESIAN_POINT ( 'NONE',  ( -51.15093573314597819, -25.30062286728702148, 4.392258012681271140 ) ) ;
#26194 = CARTESIAN_POINT ( 'NONE',  ( 9.940598223437573822, -5.876774720514426953, 21.78128695274315874 ) ) ;
#26195 = EDGE_CURVE ( 'NONE', #86736, #57446, #55853, .T. ) ;
#26196 = CARTESIAN_POINT ( 'NONE',  ( -27.40807623642065494, -24.61460109215988723, 8.230616185672861462 ) ) ;
#26197 = FACE_OUTER_BOUND ( 'NONE', #79200, .T. ) ;
#26198 = B_SPLINE_CURVE_WITH_KNOTS ( 'NONE', 3,
 ( #11612, #81133, #42089, #12109 ),
 .UNSPECIFIED., .F., .F.,
 ( 4, 4 ),
 ( 0.000000000000000000, 1.000000000000000000 ),
 .UNSPECIFIED. ) ;
#26199 = VERTEX_POINT ( 'NONE', #70557 ) ;
#26200 = EDGE_CURVE ( 'NONE', #99597, #88647, #81780, .T. ) ;
#26201 = CARTESIAN_POINT ( 'NONE',  ( 16.03631736716203449, -16.64276770305488284, 11.49999999999999645 ) ) ;
#26202 = CARTESIAN_POINT ( 'NONE',  ( 13.94817355369617751, 18.09530419158152625, -1.500000000000002220 ) ) ;
#26203 = CARTESIAN_POINT ( 'NONE',  ( -9.149999999999996803, -5.876774720514426953, 11.88602120139452012 ) ) ;
#26204 = CARTESIAN_POINT ( 'NONE',  ( -106.6228709571501412, -24.35013146730204170, 9.818937971375106599 ) ) ;
#26205 = CARTESIAN_POINT ( 'NONE',  ( -82.62936503442081460, -24.35071581493543036, 9.817618358456032368 ) ) ;
#26206 = CARTESIAN_POINT ( 'NONE',  ( -21.13723655771239152, -7.639886366525781014, 11.49999999999999645 ) ) ;
#26207 = VERTEX_POINT ( 'NONE', #40114 ) ;
#26208 = DIRECTION ( 'NONE',  ( -1.000000000000000000, -0.000000000000000000, -0.000000000000000000 ) ) ;
#26209 = VECTOR ( 'NONE', #23148, 1000.000000000000000 ) ;
#26210 = CARTESIAN_POINT ( 'NONE',  ( 1.410849576418898632, -21.91845101833037290, 11.49999999999998934 ) ) ;
#26211 = CARTESIAN_POINT ( 'NONE',  ( 32.40823333110732563, 4.442403080972329832, -4.096588619916003537 ) ) ;
#26212 = ADVANCED_FACE ( 'NONE', ( #54345 ), #46728, .F. ) ;
#26213 = CARTESIAN_POINT ( 'NONE',  ( -111.6258027458890751, -24.34968618360933945, 0.1864209137778883862 ) ) ;
#26214 = CARTESIAN_POINT ( 'NONE',  ( -70.34543693012690824, -25.03284467579916495, 7.563174216508125269 ) ) ;
#26215 = ORIENTED_EDGE ( 'NONE', *, *, #38891, .F. ) ;
#26216 = CARTESIAN_POINT ( 'NONE',  ( -48.54704611537135150, -24.15620529776628089, 10.23563542870660470 ) ) ;
#26217 = CARTESIAN_POINT ( 'NONE',  ( -0.005606649364735081555, -6.376774720514410077, 19.25713806424188235 ) ) ;
#26218 = ORIENTED_EDGE ( 'NONE', *, *, #78973, .F. ) ;
#26219 = CARTESIAN_POINT ( 'NONE',  ( -88.52287095715007581, -23.72747288104470087, -1.053458166803225460 ) ) ;
#26220 = CARTESIAN_POINT ( 'NONE',  ( -7.444040098415714013, -19.11467064512029879, 11.49999999999998934 ) ) ;
#26221 = ORIENTED_EDGE ( 'NONE', *, *, #27316, .T. ) ;
#26222 = VERTEX_POINT ( 'NONE', #9666 ) ;
#26223 = ORIENTED_EDGE ( 'NONE', *, *, #49097, .F. ) ;
#26224 = CARTESIAN_POINT ( 'NONE',  ( -50.11237177578891533, -25.31359240361684471, 5.223018419632965426 ) ) ;
#26225 = CARTESIAN_POINT ( 'NONE',  ( 1.702247502073919394, 23.03039350466679025, 11.49999999999998934 ) ) ;
#26226 = CARTESIAN_POINT ( 'NONE',  ( 14.45468597507895225, 3.471643246632551527, -28.36588305008992705 ) ) ;
#26227 = CARTESIAN_POINT ( 'NONE',  ( -14.79517943714664518, -13.99575967537150412, -1.500000000000002220 ) ) ;
#26228 = EDGE_LOOP ( 'NONE', ( #32723, #44568, #25771, #34490 ) ) ;
#26229 = CARTESIAN_POINT ( 'NONE',  ( -4.568292318365942073, -5.965225279485572685, 30.06720597538392425 ) ) ;
#26230 = CARTESIAN_POINT ( 'NONE',  ( -29.47547545905215927, -24.57318954944668832, 8.947790440257527678 ) ) ;
#26231 = EDGE_CURVE ( 'NONE', #66719, #80383, #23728, .T. ) ;
#26233 = CARTESIAN_POINT ( 'NONE',  ( -101.5292613482009898, -25.24695879370139906, 6.294269473182250607 ) ) ;
#26232 = AXIS2_PLACEMENT_3D ( 'NONE', #98416, #43164, #28919 ) ;
#26234 = DIRECTION ( 'NONE',  ( 0.000000000000000000, -2.173523156925980399E-06, 0.9999999999976378895 ) ) ;
#26235 = ORIENTED_EDGE ( 'NONE', *, *, #57251, .F. ) ;
#26236 = CARTESIAN_POINT ( 'NONE',  ( -27.89567495842467082, -25.21531660661593222, 2.285878875735976479 ) ) ;
#26237 = CARTESIAN_POINT ( 'NONE',  ( -49.19182681462018536, -25.26385729957443615, 4.415198428280462828 ) ) ;
#26238 = LOCAL_TIME ( 0, 54, 15.00000000000000000, #10945 ) ;
#26239 = ORIENTED_EDGE ( 'NONE', *, *, #54512, .T. ) ;
#26240 = CARTESIAN_POINT ( 'NONE',  ( -12.26507114386991226, -16.75673120704366426, 11.49999999999998934 ) ) ;
#26241 = EDGE_CURVE ( 'NONE', #80639, #17917, #88973, .T. ) ;
#26242 = ORIENTED_EDGE ( 'NONE', *, *, #40556, .F. ) ;
#26244 = EDGE_LOOP ( 'NONE', ( #8782, #4081, #61586, #20326 ) ) ;
#26243 = CARTESIAN_POINT ( 'NONE',  ( -102.6228709571500275, -23.48783264082478794, -1.443836473390062158 ) ) ;
#26245 = B_SPLINE_CURVE_WITH_KNOTS ( 'NONE', 3,
 ( #60539, #91454, #84344, #52918 ),
 .UNSPECIFIED., .F., .F.,
 ( 4, 4 ),
 ( 0.6809862756305058440, 0.6899927069026217108 ),
 .UNSPECIFIED. ) ;
#26246 = DIRECTION ( 'NONE',  ( -0.000000000000000000, -1.000000000000000000, -0.000000000000000000 ) ) ;
#26247 = CARTESIAN_POINT ( 'NONE',  ( -51.93149462243456327, -25.24900417239232908, 6.174051150523328424 ) ) ;
#26248 = ORIENTED_EDGE ( 'NONE', *, *, #44414, .F. ) ;
#26249 = ORIENTED_EDGE ( 'NONE', *, *, #18749, .T. ) ;
#26250 = CARTESIAN_POINT ( 'NONE',  ( -88.58953762381671027, -24.65952944569304606, 1.056160979905700570 ) ) ;
#26251 = CARTESIAN_POINT ( 'NONE',  ( -68.62287095715005592, -24.51387760970723662, 9.387446482453425389 ) ) ;
#26253 = EDGE_CURVE ( 'NONE', #23337, #59029, #24380, .T. ) ;
#26252 = DIRECTION ( 'NONE',  ( -0.4771587602595986910, -0.8788171126619707119, 0.000000000000000000 ) ) ;
#26255 = ORIENTED_EDGE ( 'NONE', *, *, #57867, .T. ) ;
#26254 = CARTESIAN_POINT ( 'NONE',  ( 13.62230711432095553, -17.35066874027886286, 11.49999999999999645 ) ) ;
#26256 = CARTESIAN_POINT ( 'NONE',  ( -49.21454750704995007, -25.13877828889947352, 7.069183601642414772 ) ) ;
#26257 = CARTESIAN_POINT ( 'NONE',  ( -21.70561270324154179, 6.225854807558039994, -1.500000000000002220 ) ) ;
#26259 = ORIENTED_EDGE ( 'NONE', *, *, #62982, .F. ) ;
#26258 = CARTESIAN_POINT ( 'NONE',  ( -28.98875734969026041, -0.3587747205144265483, 17.86602280011862476 ) ) ;
#26260 = ORIENTED_EDGE ( 'NONE', *, *, #84192, .F. ) ;
#26261 = CARTESIAN_POINT ( 'NONE',  ( -93.62287095715005592, -23.47593901973091235, -1.443836447539002865 ) ) ;
#26262 = B_SPLINE_CURVE_WITH_KNOTS ( 'NONE', 3,
 ( #25112, #49481, #26125, #8396 ),
 .UNSPECIFIED., .F., .F.,
 ( 4, 4 ),
 ( 0.000000000000000000, 9.999999999999592548E-05 ),
 .UNSPECIFIED. ) ;
#26263 = AXIS2_PLACEMENT_3D ( 'NONE', #32248, #7405, #7913 ) ;
#26264 = CARTESIAN_POINT ( 'NONE',  ( -100.6228709571500559, -23.48783264082478794, -1.443836473390061936 ) ) ;
#26265 = ORIENTED_EDGE ( 'NONE', *, *, #80711, .T. ) ;
#26266 = CARTESIAN_POINT ( 'NONE',  ( 7.804836024166685426, 19.70032748343534834, 11.49999999999998934 ) ) ;
#26267 = CARTESIAN_POINT ( 'NONE',  ( -78.94388818075310610, -25.27791636280661791, 6.014208090771517412 ) ) ;
#26268 = CARTESIAN_POINT ( 'NONE',  ( -125.6228709571499991, -24.14321612903113135, -0.2833117244521720091 ) ) ;
#26269 = FACE_BOUND ( 'NONE', #54488, .T. ) ;
#26270 = CARTESIAN_POINT ( 'NONE',  ( -21.66996937300057269, -4.939502015459471096, -1.500000000000002220 ) ) ;
#26271 = CARTESIAN_POINT ( 'NONE',  ( -74.62287095715004170, -23.72773821059536559, 11.05748984161097681 ) ) ;
#26272 = B_SPLINE_CURVE_WITH_KNOTS ( 'NONE', 3,
 ( #453, #31408, #1471, #1973, #47145, #87195, #77064, #78062 ),
 .UNSPECIFIED., .F., .F.,
 ( 4, 2, 2, 4 ),
 ( -0.001240355328177008198, -0.0002398155169400597621, 0.0007607242942968886739, 0.002761803916770776655 ),
 .UNSPECIFIED. ) ;
#26273 = EDGE_LOOP ( 'NONE', ( #68652, #21583, #9120, #77837 ) ) ;
#26274 = DIRECTION ( 'NONE',  ( 0.000000000000000000, 0.000000000000000000, -1.000000000000000000 ) ) ;
#26275 = DIRECTION ( 'NONE',  ( 0.000000000000000000, 0.000000000000000000, -1.000000000000000000 ) ) ;
#26276 = CARTESIAN_POINT ( 'NONE',  ( -36.57552185154370505, -24.66019654487199730, 8.947790411086113949 ) ) ;
#26277 = CARTESIAN_POINT ( 'NONE',  ( -58.62287095715004881, -29.50250786944525672, 11.44777988621623876 ) ) ;
#26278 = CARTESIAN_POINT ( 'NONE',  ( -8.384790838521158918, 17.58144419890746235, -1.500000000000002220 ) ) ;
#26279 = CARTESIAN_POINT ( 'NONE',  ( 21.40653236543258231, -1.377805879665675803, -1.500000000000002220 ) ) ;
#26280 = CARTESIAN_POINT ( 'NONE',  ( 32.50838937279095120, 0.6027747205144262654, -10.74666623472941218 ) ) ;
#26281 = CARTESIAN_POINT ( 'NONE',  ( -1.222978892338334012, -6.376774720514413630, 19.56655654527324373 ) ) ;
#26282 = B_SPLINE_CURVE_WITH_KNOTS ( 'NONE', 3,
 ( #89194, #3962, #57755, #3469, #35415, #18178 ),
 .UNSPECIFIED., .F., .F.,
 ( 4, 2, 4 ),
 ( 0.000000000000000000, 0.001380764517854759978, 0.002761529035709519957 ),
 .UNSPECIFIED. ) ;
#26283 = AXIS2_PLACEMENT_3D ( 'NONE', #6087, #50781, #82213 ) ;
#26284 = CARTESIAN_POINT ( 'NONE',  ( 6.650000000000004796, 0.000000000000000000, 19.30000000000000071 ) ) ;
#26285 = CARTESIAN_POINT ( 'NONE',  ( -57.92287095715005307, -23.47593901973090169, -1.443836447538997758 ) ) ;
#26286 = CARTESIAN_POINT ( 'NONE',  ( 10.71911242904675987, 20.06137936439360203, -1.500000000000002220 ) ) ;
#26287 = ADVANCED_FACE ( 'NONE', ( #88028 ), #95637, .F. ) ;
#26288 =( NAMED_UNIT ( * ) PLANE_ANGLE_UNIT ( ) SI_UNIT ( $, .RADIAN. ) );
#26289 = CARTESIAN_POINT ( 'NONE',  ( -102.5127816447745062, -24.34968618360934656, 0.1864209137778959358 ) ) ;
#26290 = DIRECTION ( 'NONE',  ( -1.000000000000000000, -3.773278334444167608E-23, -8.201307833595939069E-29 ) ) ;
#26291 = CARTESIAN_POINT ( 'NONE',  ( 0.1862606309321278575, -19.90735222434816976, 11.49999999999999645 ) ) ;
#26292 = CARTESIAN_POINT ( 'NONE',  ( -104.5511935059157480, -24.34968618360934300, 0.1864209137778872205 ) ) ;
#26293 = EDGE_CURVE ( 'NONE', #58916, #20863, #80524, .T. ) ;
#26294 = EDGE_CURVE ( 'NONE', #55826, #52307, #76904, .T. ) ;
#26295 = CARTESIAN_POINT ( 'NONE',  ( -39.49143307742559017, -24.35071581493542681, 9.817618358456035921 ) ) ;
#26296 = CARTESIAN_POINT ( 'NONE',  ( -48.61470971034470523, -23.48783264082477729, -1.443836473390069486 ) ) ;
#26297 = ORIENTED_EDGE ( 'NONE', *, *, #26868, .T. ) ;
#26298 = CARTESIAN_POINT ( 'NONE',  ( 32.16024265030974050, -0.3587747205144265483, 16.27760796525321751 ) ) ;
#26299 = CARTESIAN_POINT ( 'NONE',  ( 8.971512145086503409, -1.028487854913504362, -6.500000000000000000 ) ) ;
#26300 = EDGE_CURVE ( 'NONE', #18231, #71801, #78168, .T. ) ;
#26301 = CARTESIAN_POINT ( 'NONE',  ( 12.10466045530642631, 18.00204671274030233, -1.500000000000002220 ) ) ;
#26302 = CARTESIAN_POINT ( 'NONE',  ( -56.60508433514527837, -23.73791477778912196, 11.05961554403170766 ) ) ;
#26303 = CARTESIAN_POINT ( 'NONE',  ( -19.34354882100874562, 2.624169249526263403, -1.500000000000002220 ) ) ;
#26304 = ADVANCED_FACE ( 'NONE', ( #94629 ), #33737, .F. ) ;
#26305 = CARTESIAN_POINT ( 'NONE',  ( -55.50247564293582059, -24.15602025860896518, 10.28564288303535257 ) ) ;
#26306 = VECTOR ( 'NONE', #55151, 1000.000000000000000 ) ;
#26307 = ORIENTED_EDGE ( 'NONE', *, *, #85164, .T. ) ;
#26308 = SECURITY_CLASSIFICATION_LEVEL ( 'unclassified' ) ;
#26309 = CC_DESIGN_APPROVAL ( #85348, ( #55421 ) ) ;
#26310 = DIRECTION ( 'NONE',  ( 0.06975647374412549673, 0.9975640502598241977, 0.000000000000000000 ) ) ;
#26311 = CARTESIAN_POINT ( 'NONE',  ( -1.999887071766271784, 20.33596237858139233, 11.49999999999999645 ) ) ;
#26312 = CARTESIAN_POINT ( 'NONE',  ( -29.49875734969025842, 5.965225279485572685, 15.62202280011862321 ) ) ;
#26313 = CARTESIAN_POINT ( 'NONE',  ( -118.6228709571499564, -24.51283580621365132, 0.6167428607019855846 ) ) ;
#26314 = ORIENTED_EDGE ( 'NONE', *, *, #23414, .F. ) ;
#26315 = CARTESIAN_POINT ( 'NONE',  ( -55.62287095715006302, -23.48786465467240703, 11.44779295918255180 ) ) ;
#26316 = CARTESIAN_POINT ( 'NONE',  ( 33.24104357593923709, 3.536202174476160920, -12.73333860248705740 ) ) ;
#26317 = CARTESIAN_POINT ( 'NONE',  ( -39.22484595018107711, -25.31628611224346770, 4.963672948320522416 ) ) ;
#26318 = DIRECTION ( 'NONE',  ( -0.000000000000000000, 1.000000000000000000, -0.000000000000000000 ) ) ;
#26319 = VECTOR ( 'NONE', #54446, 1000.000000000000000 ) ;
#26320 = LINE ( 'NONE', #12074, #50026 ) ;
#26321 = VERTEX_POINT ( 'NONE', #40842 ) ;
#26322 = CARTESIAN_POINT ( 'NONE',  ( -42.55620429048338593, -24.65952944569303895, 1.056160979905692576 ) ) ;
#26323 = CARTESIAN_POINT ( 'NONE',  ( 14.22603995551189371, 18.00578905361294346, 11.49999999999999645 ) ) ;
#26324 = CARTESIAN_POINT ( 'NONE',  ( 21.64774270073068863, 7.000884456547583845, 11.49999999999998934 ) ) ;
#26325 = CARTESIAN_POINT ( 'NONE',  ( 4.967948717948723392, -6.376774720514415407, 20.00140224358974095 ) ) ;
#26326 = B_SPLINE_SURFACE_WITH_KNOTS ( 'NONE', 3, 3, ( 
 ( #43979, #29243, #27755, #58705 ),
 ( #60216, #19133, #81044, #3934 ),
 ( #65849, #34871, #27265, #4923 ),
 ( #96765, #28754, #89158, #50596 ),
 ( #81551, #74909, #51098, #42993 ),
 ( #73933, #4431, #5414, #35379 ),
 ( #82043, #59211, #35866, #12522 ),
 ( #90155, #36367, #67324, #20630 ),
 ( #44988, #61712, #85022, #62211 ),
 ( #14513, #23113, #92634, #54101 ) ),
 .UNSPECIFIED., .F., .F., .F.,
 ( 4, 3, 3, 4 ),
 ( 4, 4 ),
 ( 0.7022005934544806038, 0.7765311282028792839, 0.8508616629512779639, 0.9995227324480753239 ),
 ( 0.1495120405554173637, 0.1506138728599011600 ),
 .UNSPECIFIED. ) ;
#26327 = CARTESIAN_POINT ( 'NONE',  ( -80.52287095715006160, -29.50249982740957577, 7.747779886224967605 ) ) ;
#26328 = CARTESIAN_POINT ( 'NONE',  ( -90.54141678234942958, -24.92564183028978775, 1.928384488918253092 ) ) ;
#26329 = DIRECTION ( 'NONE',  ( 0.000000000000000000, -1.000000000000000000, 0.000000000000000000 ) ) ;
#26330 = CARTESIAN_POINT ( 'NONE',  ( 30.77564450787170003, 1.682774720514426114, -9.689394075852828081 ) ) ;
#26331 = CARTESIAN_POINT ( 'NONE',  ( -16.30586240431254197, 14.59307310709210626, -1.500000000000002220 ) ) ;
#26332 = CARTESIAN_POINT ( 'NONE',  ( -69.50621745294765219, -24.15620529776627734, 10.23563542870660825 ) ) ;
#26333 = VECTOR ( 'NONE', #17916, 1000.000000000000000 ) ;
#26334 = CARTESIAN_POINT ( 'NONE',  ( -48.89798248884767418, -25.28421271704163686, 5.878056207824126744 ) ) ;
#26335 = DIRECTION ( 'NONE',  ( 0.09824042138329625029, 0.9951627101165079203, 3.504396110891627214E-15 ) ) ;
#26336 = CARTESIAN_POINT ( 'NONE',  ( -58.62775217774146341, -24.51314013834315020, 0.6176544820404091807 ) ) ;
#26337 = ORIENTED_EDGE ( 'NONE', *, *, #93757, .T. ) ;
#26338 = PRODUCT_DEFINITION_SHAPE ( 'NONE', 'NONE',  #95340 ) ;
#26339 = CARTESIAN_POINT ( 'NONE',  ( -5.688044216684545518, -19.60349290560521140, 11.49999999999998934 ) ) ;
#26340 = VERTEX_POINT ( 'NONE', #41351 ) ;
#26341 = VERTEX_POINT ( 'NONE', #40350 ) ;
#26342 = CARTESIAN_POINT ( 'NONE',  ( -9.967090755842360039, -20.75144515299163217, -1.500000000000002220 ) ) ;
#26343 = CARTESIAN_POINT ( 'NONE',  ( -103.5228709571500758, -29.50250243563736774, 8.947779886222138046 ) ) ;
#26344 = ORIENTED_EDGE ( 'NONE', *, *, #7999, .F. ) ;
#26345 = CARTESIAN_POINT ( 'NONE',  ( 8.000000000000003553, -5.876774720514426953, 22.50000000000000355 ) ) ;
#26346 = CARTESIAN_POINT ( 'NONE',  ( -50.52287095715006160, -23.47593901973090169, -1.443836447538997092 ) ) ;
#26347 = DIRECTION ( 'NONE',  ( -1.000000000000000000, 1.232047923278981953E-16, 0.000000000000000000 ) ) ;
#26348 = DIRECTION ( 'NONE',  ( -1.000000000000000000, 0.000000000000000000, -0.000000000000000000 ) ) ;
#26350 = ORIENTED_EDGE ( 'NONE', *, *, #27938, .F. ) ;
#26349 = CARTESIAN_POINT ( 'NONE',  ( 21.39645853268639186, 0.3907444525687319703, 11.49999999999999645 ) ) ;
#26351 = CIRCLE ( 'NONE', #23133, 1.529999999999999805 ) ;
#26352 = ORIENTED_EDGE ( 'NONE', *, *, #99941, .T. ) ;
#26353 = CARTESIAN_POINT ( 'NONE',  ( -22.15176777451872425, 1.842445310382735624, 11.49999999999998934 ) ) ;
#26354 = CARTESIAN_POINT ( 'NONE',  ( 3.345817365282868217, 20.41450801592841557, 11.49999999999998934 ) ) ;
#26355 = EDGE_CURVE ( 'NONE', #34238, #26990, #18504, .T. ) ;
#26356 = ORIENTED_EDGE ( 'NONE', *, *, #90669, .F. ) ;
#26357 = DIRECTION ( 'NONE',  ( -0.000000000000000000, 2.173523156925979552E-06, -0.9999999999976378895 ) ) ;
#26358 = EDGE_CURVE ( 'NONE', #87883, #39840, #57952, .T. ) ;
#26359 = CARTESIAN_POINT ( 'NONE',  ( -70.79206301948316593, -25.20650855361216713, 6.812664954086296021 ) ) ;
#26360 = ORIENTED_EDGE ( 'NONE', *, *, #68378, .T. ) ;
#26361 = PLANE ( 'NONE',  #64032 ) ;
#26362 = B_SPLINE_CURVE_WITH_KNOTS ( 'NONE', 3,
 ( #29314, #44049, #67900, #45058 ),
 .UNSPECIFIED., .F., .F.,
 ( 4, 4 ),
 ( 0.000000000000000000, 0.0001000000000000167422 ),
 .UNSPECIFIED. ) ;
#26363 = VERTEX_POINT ( 'NONE', #87528 ) ;
#26364 = CARTESIAN_POINT ( 'NONE',  ( 9.016989526679575206, -3.316774720514426900, -27.05137190084761301 ) ) ;
#26365 = CARTESIAN_POINT ( 'NONE',  ( -2.496121100066326814, 20.73550571027955769, -1.500000000000002220 ) ) ;
#26366 = CARTESIAN_POINT ( 'NONE',  ( 21.76694381678408519, 2.417257996116004115, 11.49999999999999645 ) ) ;
#26367 = CARTESIAN_POINT ( 'NONE',  ( -106.6228709571500559, -24.65952944569304606, 1.056160979905703012 ) ) ;
#26368 = CARTESIAN_POINT ( 'NONE',  ( 32.53135143123563466, -5.965225279485572685, 6.926385399448451885 ) ) ;
#26369 = CARTESIAN_POINT ( 'NONE',  ( 19.77564376705174709, 10.73071584254150856, 11.49999999999998934 ) ) ;
#26370 = CARTESIAN_POINT ( 'NONE',  ( 7.117523389609132778, 19.69228268689324324, 11.49999999999998934 ) ) ;
#26371 = CARTESIAN_POINT ( 'NONE',  ( -38.58105435577196118, -24.51314013834316086, 0.6176544820404135105 ) ) ;
#26372 = CARTESIAN_POINT ( 'NONE',  ( -23.59123376470063960, -6.143225279485574397, 23.50402280011862288 ) ) ;
#26373 = VECTOR ( 'NONE', #9804, 1000.000000000000000 ) ;
#26374 = FACE_OUTER_BOUND ( 'NONE', #90348, .T. ) ;
#26375 = ORIENTED_EDGE ( 'NONE', *, *, #44528, .F. ) ;
#26376 = APPROVAL_PERSON_ORGANIZATION ( #90196, #64905, #91187 ) ;
#26377 = VERTEX_POINT ( 'NONE', #80408 ) ;
#26378 = EDGE_LOOP ( 'NONE', ( #57828, #71937, #71193, #3613 ) ) ;
#26379 = B_SPLINE_CURVE_WITH_KNOTS ( 'NONE', 3,
 ( #7940, #25162, #38890, #24164 ),
 .UNSPECIFIED., .F., .F.,
 ( 4, 4 ),
 ( 0.000000000000000000, 9.999999999998897304E-05 ),
 .UNSPECIFIED. ) ;
#26380 = CARTESIAN_POINT ( 'NONE',  ( -52.53220978181458634, -24.65952944569304606, 1.056160979905696351 ) ) ;
#26381 = ORIENTED_EDGE ( 'NONE', *, *, #73053, .T. ) ;
#26382 = CARTESIAN_POINT ( 'NONE',  ( 20.74164082462262471, 5.259929546262127609, -1.500000000000002220 ) ) ;
#26383 = VECTOR ( 'NONE', #38023, 1000.000000000000000 ) ;
#26384 = ORIENTED_EDGE ( 'NONE', *, *, #49221, .T. ) ;
#26385 = CARTESIAN_POINT ( 'NONE',  ( -26.11711738945389172, -24.95252434176281753, 5.477325856322839748 ) ) ;
#26386 = CARTESIAN_POINT ( 'NONE',  ( -11.11193726737652199, 17.91617163517716804, -1.500000000000002220 ) ) ;
#26387 = CARTESIAN_POINT ( 'NONE',  ( -61.62287095715004881, -23.47593901973091235, -1.443836447539007972 ) ) ;
#26388 = CARTESIAN_POINT ( 'NONE',  ( 2.989331223418256744, -6.376774720514424288, 21.46569930292093886 ) ) ;
#26389 = CARTESIAN_POINT ( 'NONE',  ( -43.55620429048339304, -23.47596703998600276, 11.44779298504227505 ) ) ;
#26390 = CARTESIAN_POINT ( 'NONE',  ( -24.55517127435777525, -0.3587747205143967943, -15.44180958690143157 ) ) ;
#26391 = CARTESIAN_POINT ( 'NONE',  ( -129.5220745341863733, -23.96169478059714208, 10.65365249895717348 ) ) ;
#26392 = CARTESIAN_POINT ( 'NONE',  ( -0.5447568859041533873, -22.05808898580190558, -1.500000000000002220 ) ) ;
#26393 = AXIS2_PLACEMENT_3D ( 'NONE', #47103, #36595, #98984 ) ;
#26394 = ORIENTED_EDGE ( 'NONE', *, *, #92724, .T. ) ;
#26395 = CARTESIAN_POINT ( 'NONE',  ( -65.55175419035504092, -24.15602025860896518, 10.28564288303534724 ) ) ;
#26396 = PLANE ( 'NONE',  #38398 ) ;
#26397 = CARTESIAN_POINT ( 'NONE',  ( -41.25901049487872996, -25.31624695023827698, 5.328837378496615429 ) ) ;
#26398 = EDGE_CURVE ( 'NONE', #31972, #76784, #39842, .T. ) ;
#26399 = CARTESIAN_POINT ( 'NONE',  ( -29.84429507560729178, -25.08342498570734591, 2.662461283694066427 ) ) ;
#26400 = DIRECTION ( 'NONE',  ( 0.000000000000000000, -0.9999999999976377785, -2.173523156925979975E-06 ) ) ;
#26401 = DIRECTION ( 'NONE',  ( 0.000000000000000000, -0.9999999999976377785, -2.173523156925979128E-06 ) ) ;
#26402 = CARTESIAN_POINT ( 'NONE',  ( 13.79380260783658407, 16.28676726024703214, 11.49999999999998934 ) ) ;
#26403 = CARTESIAN_POINT ( 'NONE',  ( -91.92287095715005307, -23.47596703998600631, 11.44779298504227860 ) ) ;
#26404 = CARTESIAN_POINT ( 'NONE',  ( -49.88863945552024148, -25.20650842489795451, 6.812665538484691474 ) ) ;
#26405 = CARTESIAN_POINT ( 'NONE',  ( -64.54379277406458471, -24.35071581493543391, 9.817618358456023486 ) ) ;
#26406 = FACE_OUTER_BOUND ( 'NONE', #40622, .T. ) ;
#26407 = CARTESIAN_POINT ( 'NONE',  ( 4.940617368476682536, -22.01678987175928981, -1.500000000000002220 ) ) ;
#26408 = VECTOR ( 'NONE', #33261, 1000.000000000000000 ) ;
#26409 = B_SPLINE_SURFACE_WITH_KNOTS ( 'NONE', 3, 3, ( 
 ( #33633, #9278, #49371, #64105 ),
 ( #87919, #95026, #86411, #32120 ),
 ( #40243, #56982, #18402, #63092 ),
 ( #86909, #64613, #78284, #65107 ),
 ( #95527, #24505, #56489, #71195 ),
 ( #3198, #87410, #9788, #63598 ),
 ( #94521, #25002, #40739, #96027 ) ),
 .UNSPECIFIED., .F., .F., .F.,
 ( 4, 3, 4 ),
 ( 4, 4 ),
 ( 0.0004766839783839066499, 0.1029713700210905941, 0.2054660560637972810 ),
 ( 0.4796160033653972810, 0.4808500218641223456 ),
 .UNSPECIFIED. ) ;
#26410 = CARTESIAN_POINT ( 'NONE',  ( -54.52287095715006870, -23.48786465467240347, 11.44779295918255002 ) ) ;
#26411 = EDGE_LOOP ( 'NONE', ( #42995, #87645, #53924, #2923 ) ) ;
#26412 = CARTESIAN_POINT ( 'NONE',  ( 13.59451591917074431, 3.316774720514426456, -28.23515841827053308 ) ) ;
#26413 = CARTESIAN_POINT ( 'NONE',  ( -31.58037117919289116, -24.51419770103156637, 9.386484678747187615 ) ) ;
#26414 = CARTESIAN_POINT ( 'NONE',  ( -5.084378373094740944, 19.06436389234985285, 11.49999999999999645 ) ) ;
#26415 = CARTESIAN_POINT ( 'NONE',  ( -10.34999999999997833, 27.69999999999999929, 0.000000000000000000 ) ) ;
#26416 = ADVANCED_FACE ( 'NONE', ( #56084 ), #10901, .T. ) ;
#26417 = CARTESIAN_POINT ( 'NONE',  ( -67.55389679207142706, -23.96119346886879953, -0.6495511937832114668 ) ) ;
#26418 = VERTEX_POINT ( 'NONE', #87017 ) ;
#26419 = LINE ( 'NONE', #18305, #45773 ) ;
#26420 = CARTESIAN_POINT ( 'NONE',  ( -127.4728709571500360, -25.21147115331108779, 5.000950862241218431 ) ) ;
#26421 = VECTOR ( 'NONE', #62689, 1000.000000000000000 ) ;
#26422 = EDGE_CURVE ( 'NONE', #47994, #56546, #48473, .T. ) ;
#26423 = DIRECTION ( 'NONE',  ( 0.000000000000000000, 0.000000000000000000, -1.000000000000000000 ) ) ;
#26424 = B_SPLINE_CURVE_WITH_KNOTS ( 'NONE', 3,
 ( #99327, #16455, #83602, #70258, #37444, #52668 ),
 .UNSPECIFIED., .F., .F.,
 ( 4, 2, 4 ),
 ( 0.000000000000000000, 0.001380901958385388545, 0.002761803916770777089 ),
 .UNSPECIFIED. ) ;
#26425 = CARTESIAN_POINT ( 'NONE',  ( -21.57561264457377348, 0.06291308125064201673, 11.49999999999998934 ) ) ;
#26426 = CARTESIAN_POINT ( 'NONE',  ( -88.62287095715004170, -23.47593901973091235, -1.443836447539002865 ) ) ;
#26427 = CARTESIAN_POINT ( 'NONE',  ( -32.66693570750084774, -24.97155988971761431, 2.105726520353297548 ) ) ;
#26428 = ADVANCED_FACE ( 'NONE', ( #72305 ), #64210, .T. ) ;
#26429 = DIRECTION ( 'NONE',  ( 0.000000000000000000, 0.000000000000000000, -1.000000000000000000 ) ) ;
#26430 = CARTESIAN_POINT ( 'NONE',  ( -81.57174390479045201, -25.13765173071444536, 7.079220311505046048 ) ) ;
#26431 = CARTESIAN_POINT ( 'NONE',  ( -11.78406182805296254, 15.88391379356440503, -1.500000000000002220 ) ) ;
#26432 = ORIENTED_EDGE ( 'NONE', *, *, #47546, .T. ) ;
#26433 = B_SPLINE_CURVE_WITH_KNOTS ( 'NONE', 3,
 ( #29060, #90961, #20942, #53412, #82843, #84337 ),
 .UNSPECIFIED., .F., .F.,
 ( 4, 2, 4 ),
 ( 1.570755371634170283E-05, 0.001396183895866089705, 0.002776660238015837747 ),
 .UNSPECIFIED. ) ;
#26434 = VECTOR ( 'NONE', #63245, 1000.000000000000227 ) ;
#26435 = EDGE_CURVE ( 'NONE', #79539, #9124, #54686, .T. ) ;
#26436 = CARTESIAN_POINT ( 'NONE',  ( 17.43904876784772284, 10.37648870149486413, 11.49999999999999645 ) ) ;
#26437 = CARTESIAN_POINT ( 'NONE',  ( 13.64113475014448618, 3.316774720514425567, -28.24100986136700442 ) ) ;
#26438 = EDGE_CURVE ( 'NONE', #27719, #34332, #34243, .T. ) ;
#26439 = ORIENTED_EDGE ( 'NONE', *, *, #66964, .F. ) ;
#26440 = CARTESIAN_POINT ( 'NONE',  ( 33.69795529655567634, 6.475225279485573360, 20.86760796525322093 ) ) ;
#26441 = CARTESIAN_POINT ( 'NONE',  ( -107.5228709571500758, -29.50250243563736774, 8.947779886222136270 ) ) ;
#26442 = CARTESIAN_POINT ( 'NONE',  ( -51.48648995077594748, -25.27191416516480871, 5.909279887552581378 ) ) ;
#26443 = DIRECTION ( 'NONE',  ( -1.000000000000000000, 0.000000000000000000, 0.000000000000000000 ) ) ;
#26444 = CARTESIAN_POINT ( 'NONE',  ( 32.25249349869195470, -1.684774720514423674, -12.65342752644894553 ) ) ;
#26445 = CARTESIAN_POINT ( 'NONE',  ( -89.62287095715004170, -29.50248528299804818, 1.056150453629040253 ) ) ;
#26446 = CARTESIAN_POINT ( 'NONE',  ( -5.935188749463110369, 19.13178230186815298, 11.49999999999998934 ) ) ;
#26447 = EDGE_CURVE ( 'NONE', #62297, #12467, #12752, .T. ) ;
#26448 = LINE ( 'NONE', #57412, #6178 ) ;
#26449 = ORIENTED_EDGE ( 'NONE', *, *, #92593, .F. ) ;
#26450 = VECTOR ( 'NONE', #100267, 1000.000000000000114 ) ;
#26452 = CARTESIAN_POINT ( 'NONE',  ( -90.62287095715004170, -23.47596703998600631, 11.44779298504227860 ) ) ;
#26451 = CC_DESIGN_SECURITY_CLASSIFICATION ( #78282, ( #100425 ) ) ;
#26453 = CARTESIAN_POINT ( 'NONE',  ( -122.6228709571500417, -29.50250243563736774, 8.947779886222134493 ) ) ;
#26454 = CARTESIAN_POINT ( 'NONE',  ( -92.62287095715004170, -24.50321055353805377, 9.387540953477525818 ) ) ;
#26455 = PLANE ( 'NONE',  #73985 ) ;
#26456 = CARTESIAN_POINT ( 'NONE',  ( -103.5228709571500758, -24.65952944569304606, 1.056160979905702346 ) ) ;
#26457 = CARTESIAN_POINT ( 'NONE',  ( 2.230654205607476737, -2.168404344971008868E-16, 0.1647943925233645579 ) ) ;
#26458 = AXIS2_PLACEMENT_3D ( 'NONE', #36379, #67845, #91158 ) ;
#26459 = CARTESIAN_POINT ( 'NONE',  ( -98.87475183225456021, -25.25978491487772004, 3.590542621692357717 ) ) ;
#26460 = EDGE_LOOP ( 'NONE', ( #88864, #71275, #50086, #39288 ) ) ;
#26461 = CARTESIAN_POINT ( 'NONE',  ( -19.38859340154505873, -6.080128201517944753, 11.49999999999998934 ) ) ;
#26462 = VECTOR ( 'NONE', #57859, 1000.000000000000114 ) ;
#26463 = VERTEX_POINT ( 'NONE', #66211 ) ;
#26464 = CARTESIAN_POINT ( 'NONE',  ( -12.73177969873712279, -19.06072230859735939, 11.49999999999998934 ) ) ;
#26465 = CARTESIAN_POINT ( 'NONE',  ( -32.48910047119002087, -24.34968618360933590, 0.1864209137778856384 ) ) ;
#26466 = CARTESIAN_POINT ( 'NONE',  ( -127.5208712269004252, -24.66019654487200441, 8.947790411086106843 ) ) ;
#26467 = EDGE_LOOP ( 'NONE', ( #62289, #79204, #44599, #50825 ) ) ;
#26468 = CARTESIAN_POINT ( 'NONE',  ( -59.49820692736138028, -24.35071581493543391, 9.817618358456035921 ) ) ;
#26470 = EDGE_CURVE ( 'NONE', #38206, #97546, #36235, .T. ) ;
#26469 = CARTESIAN_POINT ( 'NONE',  ( 14.98548720554672187, 3.495622884075268999, -27.33451462832999113 ) ) ;
#26471 = CARTESIAN_POINT ( 'NONE',  ( -30.47287095715006444, -24.38745407128210019, 0.3244550880798094949 ) ) ;
#26472 = CARTESIAN_POINT ( 'NONE',  ( -19.96038302963917488, -7.207760892512529161, 11.49999999999999645 ) ) ;
#26473 = CARTESIAN_POINT ( 'NONE',  ( 17.03105324785762420, 14.15717209551829647, 11.49999999999998934 ) ) ;
#26474 = ADVANCED_FACE ( 'NONE', ( #20002 ), #97130, .F. ) ;
#26475 = CARTESIAN_POINT ( 'NONE',  ( 18.07347782881280907, 9.871946371954690491, 11.49999999999998934 ) ) ;
#26476 = ORIENTED_EDGE ( 'NONE', *, *, #37996, .T. ) ;
#26477 = DIRECTION ( 'NONE',  ( 3.773278334444167608E-23, -1.000000000000000000, 0.000000000000000000 ) ) ;
#26478 = VERTEX_POINT ( 'NONE', #58576 ) ;
#26479 = CARTESIAN_POINT ( 'NONE',  ( 7.081057417352553784, -6.376774720514424288, 21.11453472826393352 ) ) ;
#26480 = CARTESIAN_POINT ( 'NONE',  ( 2.589743589743596086, -5.876774720514419847, 20.00140224358974095 ) ) ;
#26481 = ORIENTED_EDGE ( 'NONE', *, *, #14979, .F. ) ;
#26482 = ORIENTED_EDGE ( 'NONE', *, *, #83320, .F. ) ;
#26483 = ORIENTED_EDGE ( 'NONE', *, *, #44779, .T. ) ;
#26484 = PLANE ( 'NONE',  #94003 ) ;
#26485 = FACE_OUTER_BOUND ( 'NONE', #7492, .T. ) ;
#26486 = CARTESIAN_POINT ( 'NONE',  ( -91.62287095715004170, -24.34917612406837861, 0.1852690917426654815 ) ) ;
#26487 = CARTESIAN_POINT ( 'NONE',  ( -10.32638548400381673, 17.97674989526738898, -1.500000000000002220 ) ) ;
#26488 = CARTESIAN_POINT ( 'NONE',  ( 21.03555826204448209, -5.341079136732027166, 11.49999999999999645 ) ) ;
#26489 = ORIENTED_EDGE ( 'NONE', *, *, #55776, .T. ) ;
#26490 = VECTOR ( 'NONE', #14883, 1000.000000000000000 ) ;
#26491 = LINE ( 'NONE', #96489, #25582 ) ;
#26492 = CARTESIAN_POINT ( 'NONE',  ( 13.57151214508650305, 0.000000000000000000, 0.000000000000000000 ) ) ;
#26493 = CARTESIAN_POINT ( 'NONE',  ( -14.11974515630795501, -17.41659395067913962, -1.500000000000002220 ) ) ;
#26494 = DIRECTION ( 'NONE',  ( -1.000000000000000000, 0.000000000000000000, 0.000000000000000000 ) ) ;
#26495 = CARTESIAN_POINT ( 'NONE',  ( -58.22287095715005734, -23.47596703998600276, 11.44779298504227683 ) ) ;
#26496 = ORIENTED_EDGE ( 'NONE', *, *, #97973, .F. ) ;
#26497 = CARTESIAN_POINT ( 'NONE',  ( 33.74607884027702909, -0.3587747205144265483, -4.999864028243830916 ) ) ;
#26498 = DIRECTION ( 'NONE',  ( 0.000000000000000000, 0.000000000000000000, 1.000000000000000000 ) ) ;
#26499 = VECTOR ( 'NONE', #20930, 1000.000000000000000 ) ;
#26500 = ORIENTED_EDGE ( 'NONE', *, *, #30820, .T. ) ;
#26501 = EDGE_LOOP ( 'NONE', ( #46211, #9993, #88373, #65001 ) ) ;
#26502 = CARTESIAN_POINT ( 'NONE',  ( -87.62287095715004170, -24.50216790748098816, 0.6166512839513664801 ) ) ;
#26503 = PRODUCT_RELATED_PRODUCT_CATEGORY ( 'detail', '', ( #28832 ) ) ;
#26504 = VERTEX_POINT ( 'NONE', #43357 ) ;
#26505 = CARTESIAN_POINT ( 'NONE',  ( -17.82860346875387947, 11.52481846644873187, -1.500000000000002220 ) ) ;
#26506 = ORIENTED_EDGE ( 'NONE', *, *, #8092, .T. ) ;
#26507 = CARTESIAN_POINT ( 'NONE',  ( -88.60252077244210511, -23.48783264082477018, -1.443836473390093467 ) ) ;
#26508 = CARTESIAN_POINT ( 'NONE',  ( 4.989390281198801347, -21.28523531580253803, -1.500000000000002220 ) ) ;
#26509 = CARTESIAN_POINT ( 'NONE',  ( -52.58731372522222358, -24.35071581493542681, 9.817618358456035921 ) ) ;
#26510 = CARTESIAN_POINT ( 'NONE',  ( -40.55984193903805846, -25.28892422735297174, 3.296901279442651322 ) ) ;
#26511 = CARTESIAN_POINT ( 'NONE',  ( 5.367993895751241418, -5.876774720514418071, 20.45854982692612722 ) ) ;
#26512 = CARTESIAN_POINT ( 'NONE',  ( 20.64021973274467570, 7.317367941133321452, -1.500000000000002220 ) ) ;
#26513 = CARTESIAN_POINT ( 'NONE',  ( 5.399550031317772891, -1.324225279485572893, -28.54570968858208246 ) ) ;
#26514 = EDGE_LOOP ( 'NONE', ( #23071, #4753, #62996, #89526 ) ) ;
#26515 = CARTESIAN_POINT ( 'NONE',  ( 25.13018594592114852, 5.151325109778972511, -8.770570395071676018 ) ) ;
#26516 = CARTESIAN_POINT ( 'NONE',  ( -121.5228709571500048, -23.47593901973090524, -1.443836447538996204 ) ) ;
#26517 = ORIENTED_EDGE ( 'NONE', *, *, #79662, .T. ) ;
#26518 = AXIS2_PLACEMENT_3D ( 'NONE', #93309, #10086, #48672 ) ;
#26519 = CARTESIAN_POINT ( 'NONE',  ( -30.59820534742401676, -24.75468375855055925, 1.373310540286951209 ) ) ;
#26520 = ORIENTED_EDGE ( 'NONE', *, *, #74519, .T. ) ;
#26521 = CARTESIAN_POINT ( 'NONE',  ( 9.051621769697627329, 6.475225279485570695, -27.04979394446680274 ) ) ;
#26522 = CARTESIAN_POINT ( 'NONE',  ( -12.64432969575899968, 0.3587747205143967943, -26.13179214487285407 ) ) ;
#26523 = CARTESIAN_POINT ( 'NONE',  ( -20.82729772986975547, -4.079710536234080642, 11.49999999999998934 ) ) ;
#26524 = DIRECTION ( 'NONE',  ( -1.000000000000000000, -3.773278334444166432E-23, -8.201307841325785021E-29 ) ) ;
#26525 = CARTESIAN_POINT ( 'NONE',  ( 282.9764569301858046, -6.475225279485573360, 20.79159422840526616 ) ) ;
#26526 = DIRECTION ( 'NONE',  ( 0.000000000000000000, 0.000000000000000000, -1.000000000000000000 ) ) ;
#26527 = DIRECTION ( 'NONE',  ( -0.000000000000000000, 2.173523156925979552E-06, -0.9999999999976378895 ) ) ;
#26529 = CARTESIAN_POINT ( 'NONE',  ( -19.27395093635484713, 2.380100695660296140, 11.49999999999998934 ) ) ;
#26528 = CIRCLE ( 'NONE', #83222, 129.7684398600581517 ) ;
#26530 = DIRECTION ( 'NONE',  ( 0.9940716917543757081, 0.000000000000000000, -0.1087265912856348465 ) ) ;
#26531 = VERTEX_POINT ( 'NONE', #67696 ) ;
#26532 = CARTESIAN_POINT ( 'NONE',  ( -19.52990877098713796, 1.257015143768854815, 11.49999999999999645 ) ) ;
#26533 = CARTESIAN_POINT ( 'NONE',  ( -5.576923076923076650, -6.376774720514418959, 20.44941907051282470 ) ) ;
#26534 = B_SPLINE_CURVE_WITH_KNOTS ( 'NONE', 3,
 ( #10357, #97095, #72273, #50932 ),
 .UNSPECIFIED., .F., .F.,
 ( 4, 4 ),
 ( 0.000000000000000000, 9.999999999998900014E-05 ),
 .UNSPECIFIED. ) ;
#26535 = AXIS2_PLACEMENT_3D ( 'NONE', #72207, #78290, #8798 ) ;
#26536 = EDGE_CURVE ( 'NONE', #71288, #909, #62377, .T. ) ;
#26537 = CARTESIAN_POINT ( 'NONE',  ( -42.55620429048338593, -23.48786465467240347, 11.44779295918255180 ) ) ;
#26538 = VERTEX_POINT ( 'NONE', #59581 ) ;
#26539 = CARTESIAN_POINT ( 'NONE',  ( -97.62287095715005592, -24.33832256526969218, 0.1851278514119914509 ) ) ;
#26540 = CARTESIAN_POINT ( 'NONE',  ( -75.62287095715005592, -25.00158670708909625, 2.256160236439166855 ) ) ;
#26541 = DIRECTION ( 'NONE',  ( -1.000000000000000000, 0.000000000000000000, 0.000000000000000000 ) ) ;
#26542 = CARTESIAN_POINT ( 'NONE',  ( -81.60636161561390622, -25.24813873414510113, 7.020724594378081385 ) ) ;
#26543 = CARTESIAN_POINT ( 'NONE',  ( 19.16472379399037251, -4.548241762842377689, -1.500000000000002220 ) ) ;
#26544 = ORIENTED_EDGE ( 'NONE', *, *, #40250, .F. ) ;
#26545 = EDGE_CURVE ( 'NONE', #46271, #12512, #73305, .T. ) ;
#26546 = CARTESIAN_POINT ( 'NONE',  ( -7.847517764308983956, -10.47139188923011233, 1.273303694910093986 ) ) ;
#26547 = CARTESIAN_POINT ( 'NONE',  ( 2.905029696106983916, -5.876774720514416295, 20.12486936895525957 ) ) ;
#26548 = ADVANCED_FACE ( 'NONE', ( #20989 ), #50970, .F. ) ;
#26549 = CALENDAR_DATE ( 2026, 9, 10 ) ;
#26550 = ORIENTED_EDGE ( 'NONE', *, *, #18400, .F. ) ;
#26551 = CARTESIAN_POINT ( 'NONE',  ( -106.5562042904834357, -24.64965694238575722, 8.947790433994187609 ) ) ;
#26552 = DIRECTION ( 'NONE',  ( -3.773278334453079618E-23, 0.9999999999976377785, 2.173523156925979975E-06 ) ) ;
#26553 = CARTESIAN_POINT ( 'NONE',  ( -69.62287095715007013, -24.50216790748100593, 0.6166512839513600408 ) ) ;
#26554 = CARTESIAN_POINT ( 'NONE',  ( -105.6228709571500417, -24.52323809116984066, 9.355190652339416602 ) ) ;
#26555 = CARTESIAN_POINT ( 'NONE',  ( -81.90208261351192220, -25.29489613318244423, 6.057562805997258160 ) ) ;
#26556 =( REPRESENTATION_RELATIONSHIP ('NONE','NONE', #96270, #37291 ) REPRESENTATION_RELATIONSHIP_WITH_TRANSFORMATION ( #22162 )SHAPE_REPRESENTATION_RELATIONSHIP( ) );
#26557 = B_SPLINE_CURVE_WITH_KNOTS ( 'NONE', 3,
 ( #57392, #17298, #47257, #95428 ),
 .UNSPECIFIED., .F., .F.,
 ( 4, 4 ),
 ( 0.000000000000000000, 9.999999999998897304E-05 ),
 .UNSPECIFIED. ) ;
#26558 = CARTESIAN_POINT ( 'NONE',  ( -8.160000000000000142, -0.1502355682624769706, 6.837492552117866218 ) ) ;
#26559 = DIRECTION ( 'NONE',  ( 0.000000000000000000, 0.000000000000000000, 1.000000000000000000 ) ) ;
#26560 = CARTESIAN_POINT ( 'NONE',  ( 8.914523860536577970, -17.85282776015759154, 11.49999999999998934 ) ) ;
#26561 = EDGE_CURVE ( 'NONE', #35855, #93616, #37034, .T. ) ;
#26562 = AXIS2_PLACEMENT_3D ( 'NONE', #16332, #85342, #14325 ) ;
#26563 = CARTESIAN_POINT ( 'NONE',  ( -75.49128105450554926, -24.92592662359561118, 8.075495903018000021 ) ) ;
#26564 = CARTESIAN_POINT ( 'NONE',  ( -19.70454523906213495, -2.556213046838741842, -1.500000000000002220 ) ) ;
#26565 = ORIENTED_EDGE ( 'NONE', *, *, #63019, .F. ) ;
#26566 = CARTESIAN_POINT ( 'NONE',  ( -120.6228709571500417, -23.48783264082479505, -1.443836473390058384 ) ) ;
#26567 = VECTOR ( 'NONE', #94720, 1000.000000000000000 ) ;
#26568 = CARTESIAN_POINT ( 'NONE',  ( -125.5228709571500900, -24.14321612903116332, -0.2833117244521576872 ) ) ;
#26569 = CARTESIAN_POINT ( 'NONE',  ( 6.660000000000001030, -10.15233964170348457, 0.003711184059992174607 ) ) ;
#26570 = CARTESIAN_POINT ( 'NONE',  ( 6.055070916906798217, -3.316774720512750019, -28.43998667593618990 ) ) ;
#26571 = CARTESIAN_POINT ( 'NONE',  ( -15.88994834598175387, -13.44966708658631838, 11.49999999999999645 ) ) ;
#26572 = CARTESIAN_POINT ( 'NONE',  ( -6.901944873432418248, -6.376774720514410077, 19.15221817653406688 ) ) ;
#26573 = CARTESIAN_POINT ( 'NONE',  ( -50.81585168191263335, -25.19418440451270058, 3.360232408535756665 ) ) ;
#26574 = CARTESIAN_POINT ( 'NONE',  ( 16.54545882101025711, 15.75737887292823558, 11.49999999999999645 ) ) ;
#26575 = ORIENTED_EDGE ( 'NONE', *, *, #72315, .F. ) ;
#26576 = CARTESIAN_POINT ( 'NONE',  ( -103.5228709571500758, -23.48786465467241769, 11.44779295918254114 ) ) ;
#26577 = PLANE ( 'NONE',  #93813 ) ;
#26578 = ORIENTED_EDGE ( 'NONE', *, *, #24909, .F. ) ;
#26579 = CARTESIAN_POINT ( 'NONE',  ( 18.08294815051442583, 9.098846914115775064, -1.500000000000002220 ) ) ;
#26580 = EDGE_CURVE ( 'NONE', #59029, #58206, #82891, .T. ) ;
#26581 = CARTESIAN_POINT ( 'NONE',  ( -80.62287095715005592, -29.50248528299804818, 1.056150453629038477 ) ) ;
#26582 = DIRECTION ( 'NONE',  ( -3.773278334453079030E-23, 0.9999999999976377785, 2.173523156925979128E-06 ) ) ;
#26583 = FACE_OUTER_BOUND ( 'NONE', #33086, .T. ) ;
#26584 = ORIENTED_EDGE ( 'NONE', *, *, #36567, .F. ) ;
#26586 = EDGE_CURVE ( 'NONE', #86771, #95782, #57535, .T. ) ;
#26585 = CARTESIAN_POINT ( 'NONE',  ( -79.48419046236253394, -25.30823799978809419, 5.428935451781088162 ) ) ;
#26587 = CARTESIAN_POINT ( 'NONE',  ( 0.000000000000000000, -1.477225279485574028, -1.352392034746782823 ) ) ;
#26588 = CARTESIAN_POINT ( 'NONE',  ( 19.27460657395150889, -5.330843762518559181, -1.500000000000002220 ) ) ;
#26589 = CARTESIAN_POINT ( 'NONE',  ( -17.93810645791062441, 10.97360191750010827, 11.49999999999999645 ) ) ;
#26590 = LINE ( 'NONE', #11359, #85841 ) ;
#26591 = CARTESIAN_POINT ( 'NONE',  ( -93.52287095715007581, -23.73934037231756733, 11.05740245334328975 ) ) ;
#26592 = CARTESIAN_POINT ( 'NONE',  ( 21.54648482299927181, -4.703075207800759827, -1.500000000000002220 ) ) ;
#26593 = CARTESIAN_POINT ( 'NONE',  ( 6.421796364777552668, 5.356774720514453136, -25.37953985271570900 ) ) ;
#26594 = ADVANCED_FACE ( 'NONE', ( #28618 ), #26628, .F. ) ;
#26595 = CARTESIAN_POINT ( 'NONE',  ( -97.52287095715006160, -29.50248528299804818, 1.056150453629042030 ) ) ;
#26596 = CARTESIAN_POINT ( 'NONE',  ( 33.10875634548599322, 5.965225279485572685, -11.42349945801155719 ) ) ;
#26597 = FACE_OUTER_BOUND ( 'NONE', #83399, .T. ) ;
#26598 = DIRECTION ( 'NONE',  ( 0.000000000000000000, -0.9999999999976377785, -2.173523156925979975E-06 ) ) ;
#26599 = VERTEX_POINT ( 'NONE', #35741 ) ;
#26600 = ORIENTED_EDGE ( 'NONE', *, *, #12403, .T. ) ;
#26601 = CYLINDRICAL_SURFACE ( 'NONE', #1672, 3.060000000000000053 ) ;
#26602 = B_SPLINE_CURVE_WITH_KNOTS ( 'NONE', 3,
 ( #84799, #29510, #5679, #59987 ),
 .UNSPECIFIED., .F., .F.,
 ( 4, 4 ),
 ( 0.000000000000000000, 1.000000000000000000 ),
 .UNSPECIFIED. ) ;
#26603 = CARTESIAN_POINT ( 'NONE',  ( -100.6747599127204040, -25.27404634170540376, 2.849795293083101200 ) ) ;
#26604 = CARTESIAN_POINT ( 'NONE',  ( -27.61845239340658154, -5.965225279485594001, -10.37513603161905351 ) ) ;
#26605 = CARTESIAN_POINT ( 'NONE',  ( -1.764913036440812322, 20.45846032914734280, -1.500000000000002220 ) ) ;
#26606 = VERTEX_POINT ( 'NONE', #66712 ) ;
#26607 = LINE ( 'NONE', #57569, #2442 ) ;
#26608 = CARTESIAN_POINT ( 'NONE',  ( -97.62287095715005592, -23.48786465467241058, 11.44779295918254114 ) ) ;
#26609 = DIRECTION ( 'NONE',  ( -0.000000000000000000, 1.000000000000000000, -0.000000000000000000 ) ) ;
#26610 = CARTESIAN_POINT ( 'NONE',  ( -22.12323335113916301, -3.008119206214963981, -1.500000000000002220 ) ) ;
#26611 = FACE_OUTER_BOUND ( 'NONE', #57325, .T. ) ;
#26612 = CARTESIAN_POINT ( 'NONE',  ( -121.6228709571500559, -23.47596703998600631, 11.44779298504227683 ) ) ;
#26613 = VERTEX_POINT ( 'NONE', #42372 ) ;
#26614 = FACE_OUTER_BOUND ( 'NONE', #76279, .T. ) ;
#26615 = CARTESIAN_POINT ( 'NONE',  ( -51.69888143875354558, -25.26742185460100387, 4.038564875323308989 ) ) ;
#26616 = B_SPLINE_CURVE_WITH_KNOTS ( 'NONE', 3,
 ( #861, #56666, #62783, #49050, #72384, #2879, #70372, #93698, #55164, #10974, #4368, #81487, #20075, #89098, #97699, #88601, #34315, #12463, #27701 ),
 .UNSPECIFIED., .F., .F.,
 ( 4, 1, 1, 1, 1, 1, 1, 1, 1, 1, 1, 1, 1, 1, 1, 1, 4 ),
 ( 0.000000000000000000, 0.07834298519369982394, 0.1505633028794195749, 0.2161510566599787464, 0.2756797924514269305, 0.3287070503654637710, 0.3759044348322068685, 0.4173018977400307916, 0.4526927480535820614, 0.5172652917530110583, 0.5812165680623054831, 0.6453218939728019299, 0.7120244933797625908, 0.7801300447160447460, 0.8502182262116649847, 0.9226485217347383250, 1.000000000000000000 ),
 .UNSPECIFIED. ) ;
#26617 = CARTESIAN_POINT ( 'NONE',  ( -19.85847575633505713, -6.422239212204448044, -1.500000000000002220 ) ) ;
#26618 = ORIENTED_EDGE ( 'NONE', *, *, #31811, .T. ) ;
#26619 = VECTOR ( 'NONE', #49404, 1000.000000000000114 ) ;
#26621 = EDGE_LOOP ( 'NONE', ( #17959, #49485, #57227, #46850 ) ) ;
#26620 = DIRECTION ( 'NONE',  ( -3.773278334444167608E-23, 1.000000000000000000, 0.000000000000000000 ) ) ;
#26622 = ADVANCED_FACE ( 'NONE', ( #19502 ), #11892, .T. ) ;
#26623 = ORIENTED_EDGE ( 'NONE', *, *, #10765, .T. ) ;
#26624 = CARTESIAN_POINT ( 'NONE',  ( -69.03624148920614800, -25.03149190493494203, 6.724186720489000457 ) ) ;
#26625 = CARTESIAN_POINT ( 'NONE',  ( -20.42954818520503935, 5.180689535515515587, -1.500000000000002220 ) ) ;
#26626 = ORIENTED_EDGE ( 'NONE', *, *, #20896, .T. ) ;
#26627 = CARTESIAN_POINT ( 'NONE',  ( -114.6228709571500559, -23.72773821059536559, 11.05748984161097503 ) ) ;
#26628 = CYLINDRICAL_SURFACE ( 'NONE', #10929, 1.500000000000000666 ) ;
#26629 = DIRECTION ( 'NONE',  ( 0.000000000000000000, -2.173523156925979552E-06, 0.9999999999976378895 ) ) ;
#26630 = EDGE_CURVE ( 'NONE', #20641, #50993, #7910, .T. ) ;
#26631 = CARTESIAN_POINT ( 'NONE',  ( -101.8751956322788317, -25.25419332119572857, 6.541289853642102692 ) ) ;
#26632 = DIRECTION ( 'NONE',  ( -0.09824042138329590335, 0.9951627101165078093, 3.519298150595267489E-15 ) ) ;
#26633 = CARTESIAN_POINT ( 'NONE',  ( -20.56447267657262401, 6.860157381912782348, -1.500000000000002220 ) ) ;
#26634 = CARTESIAN_POINT ( 'NONE',  ( -81.45245898465185519, -25.12224243742947749, 6.419336199521627151 ) ) ;
#26636 = ORIENTED_EDGE ( 'NONE', *, *, #57917, .T. ) ;
#26635 = CARTESIAN_POINT ( 'NONE',  ( 16.16129659511371131, 15.28805624652528472, 11.49999999999999645 ) ) ;
#26637 = CARTESIAN_POINT ( 'NONE',  ( -51.48368152949297638, -25.24728876902798902, 5.903371821033232436 ) ) ;
#26638 = DIRECTION ( 'NONE',  ( 0.6451914333552788428, 0.000000000000000000, 0.7640209514960702997 ) ) ;
#26639 = CARTESIAN_POINT ( 'NONE',  ( 28.20688450243577705, 14.82721238576592704, -7.073367244511738150 ) ) ;
#26640 = VERTEX_POINT ( 'NONE', #96623 ) ;
#26641 = VECTOR ( 'NONE', #63311, 1000.000000000000000 ) ;
#26642 = EDGE_CURVE ( 'NONE', #15369, #70394, #96340, .T. ) ;
#26643 = ADVANCED_FACE ( 'NONE', ( #68679 ), #37720, .F. ) ;
#26645 = ORIENTED_EDGE ( 'NONE', *, *, #49793, .T. ) ;
#26644 = CARTESIAN_POINT ( 'NONE',  ( 30.09341516180546350, -1.682774720514426114, -11.39311774897855933 ) ) ;
#26646 = ORIENTED_EDGE ( 'NONE', *, *, #89398, .F. ) ;
#26647 = CARTESIAN_POINT ( 'NONE',  ( 31.51256023177338861, -4.716437395117331732, -1.484035900832843868 ) ) ;
#26648 = CARTESIAN_POINT ( 'NONE',  ( -107.5228709571501042, -23.73907113217658704, -1.053371485781485317 ) ) ;
#26649 = CARTESIAN_POINT ( 'NONE',  ( -32.62287095715004881, -23.48783264082477729, -1.443836473390074371 ) ) ;
#26650 = ORIENTED_EDGE ( 'NONE', *, *, #85046, .T. ) ;
#26651 = CARTESIAN_POINT ( 'NONE',  ( -130.5728709571500303, -24.15356421501153861, -0.4487796565293491469 ) ) ;
#26652 = CARTESIAN_POINT ( 'NONE',  ( 4.981011153104904388, 21.88276397462241363, -1.500000000000002220 ) ) ;
#26653 = EDGE_CURVE ( 'NONE', #59687, #35831, #91007, .T. ) ;
#26654 = ORIENTED_EDGE ( 'NONE', *, *, #7158, .T. ) ;
#26655 = CARTESIAN_POINT ( 'NONE',  ( -112.5569623894730569, -23.73791477778912551, 11.05961554403169878 ) ) ;
#26656 = CARTESIAN_POINT ( 'NONE',  ( -94.55792968542381516, -23.73791477778911840, 11.05961554403170588 ) ) ;
#26657 = CARTESIAN_POINT ( 'NONE',  ( 10.22011794243639038, 5.356774720516090937, -27.02313658038265132 ) ) ;
#26658 = DIRECTION ( 'NONE',  ( -3.773278334453079618E-23, 0.9999999999976377785, 2.173523156925979975E-06 ) ) ;
#26659 = CARTESIAN_POINT ( 'NONE',  ( -63.92071404197809414, -24.75179208683297105, 8.640809912072082710 ) ) ;
#26660 = CARTESIAN_POINT ( 'NONE',  ( 3.881049643139886207, -19.21785841795820104, 11.49999999999998934 ) ) ;
#26661 = CARTESIAN_POINT ( 'NONE',  ( -0.02075734969026423599, 5.866774720514426278, -0.08597719988137648983 ) ) ;
#26662 = ORIENTED_EDGE ( 'NONE', *, *, #19687, .T. ) ;
#26663 = VECTOR ( 'NONE', #11310, 1000.000000000000114 ) ;
#26664 = CARTESIAN_POINT ( 'NONE',  ( -17.55493245422511350, -12.44833567967518029, 11.49999999999998934 ) ) ;
#26665 = DIRECTION ( 'NONE',  ( -0.000000000000000000, 1.000000000000000000, -0.000000000000000000 ) ) ;
#26666 = CARTESIAN_POINT ( 'NONE',  ( -114.5228709571500758, -23.72747288104470798, -1.053458166803225238 ) ) ;
#26668 = B_SPLINE_CURVE_WITH_KNOTS ( 'NONE', 3,
 ( #49292, #18322, #48789, #73120 ),
 .UNSPECIFIED., .F., .F.,
 ( 4, 4 ),
 ( 0.9194398632183746756, 0.9204406102591400352 ),
 .UNSPECIFIED. ) ;
#26667 = CARTESIAN_POINT ( 'NONE',  ( -70.52287095715007581, -23.47596703998600631, 11.44779298504228748 ) ) ;
#26669 = DIRECTION ( 'NONE',  ( 0.7512896232465891000, -1.109416176496794925E-16, 0.6599726524652351767 ) ) ;
#26670 = CARTESIAN_POINT ( 'NONE',  ( 0.5590224530292132732, -22.91010021869659852, -1.500000000000002220 ) ) ;
#26671 = EDGE_CURVE ( 'NONE', #13722, #16519, #21480, .T. ) ;
#26672 = EDGE_CURVE ( 'NONE', #69394, #67776, #99107, .T. ) ;
#26673 = COORDINATED_UNIVERSAL_TIME_OFFSET ( 0, 0, .AHEAD. ) ;
#26674 = CARTESIAN_POINT ( 'NONE',  ( -12.65407072091355722, 6.376774720514426953, -26.15404995688569301 ) ) ;
#26675 = DIRECTION ( 'NONE',  ( 0.6451914333552788428, 0.000000000000000000, 0.7640209514960702997 ) ) ;
#26676 = CARTESIAN_POINT ( 'NONE',  ( 1.781536345648733199, 20.00535218256611358, 11.49999999999999645 ) ) ;
#26677 = CARTESIAN_POINT ( 'NONE',  ( -112.6228709571500417, -24.65952944569304961, 1.056160979905702346 ) ) ;
#26678 = FACE_OUTER_BOUND ( 'NONE', #63653, .T. ) ;
#26679 = LINE ( 'NONE', #57144, #66856 ) ;
#26680 = CARTESIAN_POINT ( 'NONE',  ( -102.5228709571500758, -24.64898659630367916, 1.056161002820829697 ) ) ;
#26681 = PLANE ( 'NONE',  #26737 ) ;
#26682 = CARTESIAN_POINT ( 'NONE',  ( -19.84341114293531305, -1.032944114202840824, -1.500000000000002220 ) ) ;
#26683 = ADVANCED_FACE ( 'NONE', ( #83391 ), #60583, .T. ) ;
#26684 = CARTESIAN_POINT ( 'NONE',  ( 5.271800844963591359, 5.356774720514425603, -28.56638892015329034 ) ) ;
#26685 = CARTESIAN_POINT ( 'NONE',  ( -5.084378373094740944, 19.06436389234985285, -1.500000000000002220 ) ) ;
#26686 = CARTESIAN_POINT ( 'NONE',  ( -75.52287095715007581, -23.48786465467241769, 11.44779295918254469 ) ) ;
#26687 = ADVANCED_FACE ( 'NONE', ( #45349 ), #46334, .F. ) ;
#26688 = ADVANCED_FACE ( 'NONE', ( #77265 ), #19941, .T. ) ;
#26689 = CARTESIAN_POINT ( 'NONE',  ( 4.621320343559625066, 12.75000000000004974, 2.100000000000000089 ) ) ;
#26690 = CARTESIAN_POINT ( 'NONE',  ( 3.248328688408994580, -6.376774720514406525, 18.75910638930973917 ) ) ;
#26691 = CARTESIAN_POINT ( 'NONE',  ( -20.25002411749221665, -3.895867502427604379, 11.49999999999999645 ) ) ;
#26692 = VECTOR ( 'NONE', #84326, 1000.000000000000114 ) ;
#26693 = CARTESIAN_POINT ( 'NONE',  ( 6.660000000000001030, 0.000000000000000000, 0.000000000000000000 ) ) ;
#26694 = CARTESIAN_POINT ( 'NONE',  ( -11.11902432501355342, 19.77583997595719367, 11.49999999999999645 ) ) ;
#26695 = VERTEX_POINT ( 'NONE', #80663 ) ;
#26696 = CARTESIAN_POINT ( 'NONE',  ( -115.5562042904833788, -25.00182538069145721, 7.747789668545097541 ) ) ;
#26697 = CARTESIAN_POINT ( 'NONE',  ( -109.6228709571500559, -23.47596703998600631, 11.44779298504227860 ) ) ;
#26698 = CARTESIAN_POINT ( 'NONE',  ( -127.5228709571500616, -24.50321055353805377, 9.387540953477508054 ) ) ;
#26699 = CIRCLE ( 'NONE', #28355, 6.000000000000000888 ) ;
#26700 = CARTESIAN_POINT ( 'NONE',  ( 11.16000000000000014, -10.65233964170348635, 1.628518864987183790 ) ) ;
#26701 = B_SPLINE_CURVE_WITH_KNOTS ( 'NONE', 3,
 ( #32263, #1829, #63234, #61736, #8430, #39878, #39380, #86051, #55623, #70334, #85045, #78428, #24641, #48004, #15034 ),
 .UNSPECIFIED., .F., .F.,
 ( 4, 1, 1, 1, 1, 1, 1, 1, 1, 1, 1, 1, 4 ),
 ( 0.000000000000000000, 0.08415201884431650070, 0.1665323202984589912, 0.2488363311465309202, 0.3312461454872611122, 0.4129571090216161422, 0.4904942776695665474, 0.5661557919819242279, 0.6399873346864671797, 0.7167654882718511589, 0.8021439047100994424, 0.8958332007101933447, 1.000000000000000000 ),
 .UNSPECIFIED. ) ;
#26702 = ORIENTED_EDGE ( 'NONE', *, *, #44166, .T. ) ;
#26703 = CARTESIAN_POINT ( 'NONE',  ( -30.49308942697465952, -23.47593901973084485, -1.443836476861628970 ) ) ;
#26704 = CARTESIAN_POINT ( 'NONE',  ( -22.55118551311790753, 3.560990644294375063, -1.500000000000002220 ) ) ;
#26705 = DIRECTION ( 'NONE',  ( 0.000000000000000000, 0.9999999999976377785, 2.173523156925979128E-06 ) ) ;
#26706 = CARTESIAN_POINT ( 'NONE',  ( 0.000000000000000000, 0.000000000000000000, -9.000000000000000000 ) ) ;
#26707 = CARTESIAN_POINT ( 'NONE',  ( -63.50971770550398077, -23.96169478059713143, 10.65365249895718236 ) ) ;
#26708 = CARTESIAN_POINT ( 'NONE',  ( -21.16806448877717628, 7.570426553894726851, 11.49999999999999645 ) ) ;
#26709 = ORIENTED_EDGE ( 'NONE', *, *, #13333, .T. ) ;
#26710 = CARTESIAN_POINT ( 'NONE',  ( -43.53440695141820527, -24.51314013834316086, 0.6176544820404143987 ) ) ;
#26711 = CARTESIAN_POINT ( 'NONE',  ( -1.948345350117603125, -21.87844622001750139, -1.500000000000002220 ) ) ;
#26712 = CARTESIAN_POINT ( 'NONE',  ( -111.6235230694679785, -24.65952944569305316, 1.056160979905705455 ) ) ;
#26713 = CARTESIAN_POINT ( 'NONE',  ( -29.21998272650427708, -24.79699891632823494, 5.646414127112506343 ) ) ;
#26714 = ORIENTED_EDGE ( 'NONE', *, *, #12893, .T. ) ;
#26715 = PLANE ( 'NONE',  #52416 ) ;
#26716 = CARTESIAN_POINT ( 'NONE',  ( -107.5228709571501184, -24.33927499327856125, 9.819080762295811837 ) ) ;
#26717 = B_SPLINE_CURVE_WITH_KNOTS ( 'NONE', 3,
 ( #32280, #55637, #61251, #85563, #94173, #78945, #70854, #38390, #16045, #40402, #76937, #48019, #71355, #69344, #61750, #39892, #84562, #55134, #63250, #31276, #62245, #7939, #38889, #16541, #30272, #69850, #7435 ),
 .UNSPECIFIED., .F., .F.,
 ( 4, 1, 1, 1, 1, 1, 1, 1, 1, 1, 1, 1, 1, 1, 1, 1, 1, 1, 1, 1, 1, 1, 1, 1, 4 ),
 ( 0.000000000000000000, 0.06859462225874299324, 0.1332460424433017654, 0.1943125864682570259, 0.2512792231169669877, 0.3045134392563472181, 0.3542349066533249102, 0.4004805887739895653, 0.4434107549384915803, 0.4840148686163446845, 0.5232523007732032827, 0.5610423727283604389, 0.5979002393643996216, 0.6335184888561951055, 0.6683143511696515437, 0.7024956712863811292, 0.7366853535134582076, 0.7702931693607886210, 0.8034372550192486750, 0.8359129516660284143, 0.8684602457892908189, 0.9008465382431825041, 0.9334665246307077835, 0.9662575752981232835, 1.000000000000000000 ),
 .UNSPECIFIED. ) ;
#26718 = ORIENTED_EDGE ( 'NONE', *, *, #12649, .T. ) ;
#26719 = CARTESIAN_POINT ( 'NONE',  ( -45.52287095715004028, -24.62226745350437795, 0.9660975649728088532 ) ) ;
#26720 = CARTESIAN_POINT ( 'NONE',  ( 1.819314030819549233, -20.42850443921780013, -1.500000000000002220 ) ) ;
#26721 = EDGE_LOOP ( 'NONE', ( #37694, #24465, #99700, #7996 ) ) ;
#26723 = ORIENTED_EDGE ( 'NONE', *, *, #95826, .F. ) ;
#26722 = B_SPLINE_CURVE_WITH_KNOTS ( 'NONE', 3,
 ( #50985, #11908, #42386, #42875, #73805, #19015, #74308, #4800 ),
 .UNSPECIFIED., .F., .F.,
 ( 4, 2, 2, 4 ),
 ( -0.001224873891641433451, -0.0002244903592271139166, 0.0007758931731872056176, 0.002776660238015840349 ),
 .UNSPECIFIED. ) ;
#26724 = ORIENTED_EDGE ( 'NONE', *, *, #64133, .F. ) ;
#26725 = CARTESIAN_POINT ( 'NONE',  ( -80.54756436351547677, -25.13342022318803615, 7.100032767599389061 ) ) ;
#26726 = CARTESIAN_POINT ( 'NONE',  ( 19.36532470938277228, 12.59445105952145738, -1.500000000000002220 ) ) ;
#26727 = CARTESIAN_POINT ( 'NONE',  ( -104.5928576678435746, -23.96169478059713853, 10.65365249895717525 ) ) ;
#26728 = CARTESIAN_POINT ( 'NONE',  ( 18.91379238805564356, 7.493326543281090935, -1.500000000000002220 ) ) ;
#26729 = ORIENTED_EDGE ( 'NONE', *, *, #73851, .F. ) ;
#26730 = CARTESIAN_POINT ( 'NONE',  ( -0.02075734969026423599, -0.3587747205144213303, -0.08597719988137648983 ) ) ;
#26731 = CARTESIAN_POINT ( 'NONE',  ( -50.78270459440467732, -25.12977507029983926, 2.884057882057353694 ) ) ;
#26732 = CARTESIAN_POINT ( 'NONE',  ( -105.5874393031439809, -24.73486907724918282, 1.287355809206962576 ) ) ;
#26733 = LINE ( 'NONE', #11009, #94977 ) ;
#26734 = ORIENTED_EDGE ( 'NONE', *, *, #3097, .T. ) ;
#26735 = CARTESIAN_POINT ( 'NONE',  ( -29.10059600771309007, -24.76881121394164964, 3.504325771330080386 ) ) ;
#26736 = CARTESIAN_POINT ( 'NONE',  ( -8.978253834636468866, -6.376774720514426953, 21.48128695274316158 ) ) ;
#26737 = AXIS2_PLACEMENT_3D ( 'NONE', #81471, #11945, #35299 ) ;
#26738 = ORIENTED_EDGE ( 'NONE', *, *, #22256, .F. ) ;
#26739 = CARTESIAN_POINT ( 'NONE',  ( -20.13249939377427111, -5.111880259578561514, 11.49999999999998934 ) ) ;
#26740 = ORIENTED_EDGE ( 'NONE', *, *, #91809, .T. ) ;
#26742 = ORIENTED_EDGE ( 'NONE', *, *, #7350, .F. ) ;
#26741 = CARTESIAN_POINT ( 'NONE',  ( 10.34999999999999254, -4.939065598916630706E-16, 2.100000000000000977 ) ) ;
#26743 = EDGE_CURVE ( 'NONE', #37899, #69965, #11643, .T. ) ;
#26744 = CARTESIAN_POINT ( 'NONE',  ( -77.52287095715006160, -24.33832256527049154, 0.1851278514138615938 ) ) ;
#26745 = CARTESIAN_POINT ( 'NONE',  ( -102.6228709571500985, -24.33832256526968862, 0.1851278514119935603 ) ) ;
#26746 = ORIENTED_EDGE ( 'NONE', *, *, #70402, .F. ) ;
#26747 = VERTEX_POINT ( 'NONE', #18264 ) ;
#26748 = LINE ( 'NONE', #74901, #93253 ) ;
#26749 = CARTESIAN_POINT ( 'NONE',  ( 22.02124265030973760, -4.543225279485573864, 17.35402280011862786 ) ) ;
#26750 = CARTESIAN_POINT ( 'NONE',  ( -43.49938052968830959, -24.15620529776627734, 10.23563542870661003 ) ) ;
#26752 = ORIENTED_EDGE ( 'NONE', *, *, #36471, .T. ) ;
#26751 = CARTESIAN_POINT ( 'NONE',  ( -19.65368394218270254, -10.04821906498216499, 11.49999999999999645 ) ) ;
#26753 = CARTESIAN_POINT ( 'NONE',  ( -47.62287095715005592, -24.35013146730204170, 9.818937971375113705 ) ) ;
#26754 = CARTESIAN_POINT ( 'NONE',  ( 21.16457415087624128, -7.944649954575952577, 11.49999999999998934 ) ) ;
#26755 = ADVANCED_FACE ( 'NONE', ( #65469 ), #96888, .T. ) ;
#26756 = EDGE_CURVE ( 'NONE', #63436, #8729, #27381, .T. ) ;
#26757 = EDGE_CURVE ( 'NONE', #89963, #52986, #18754, .T. ) ;
#26759 = ORIENTED_EDGE ( 'NONE', *, *, #10032, .T. ) ;
#26758 = DIRECTION ( 'NONE',  ( 0.7640209514960704107, 0.000000000000000000, -0.6451914333552789538 ) ) ;
#26760 = ORIENTED_EDGE ( 'NONE', *, *, #24268, .T. ) ;
#26761 = EDGE_CURVE ( 'NONE', #34988, #66705, #95885, .T. ) ;
#26762 = CARTESIAN_POINT ( 'NONE',  ( 33.13288845015618023, -0.3587747205144265483, -0.1650522222209214185 ) ) ;
#26763 = VECTOR ( 'NONE', #27947, 1000.000000000000114 ) ;
#26764 = CARTESIAN_POINT ( 'NONE',  ( -36.55620429048339304, -24.64965694238575011, 8.947790433994200043 ) ) ;
#26765 = VERTEX_POINT ( 'NONE', #19745 ) ;
#26766 = CARTESIAN_POINT ( 'NONE',  ( 9.297385241821217505, 19.04214385377821017, 11.49999999999998934 ) ) ;
#26767 = FACE_OUTER_BOUND ( 'NONE', #68148, .T. ) ;
#26768 = FACE_OUTER_BOUND ( 'NONE', #73322, .T. ) ;
#26769 = CARTESIAN_POINT ( 'NONE',  ( -22.27612280437926273, 0.2766752662994830247, -1.500000000000002220 ) ) ;
#26770 = DIRECTION ( 'NONE',  ( 0.000000000000000000, -0.9999999999976377785, -2.173523156925979975E-06 ) ) ;
#26771 = ADVANCED_FACE ( 'NONE', ( #41616 ), #71751, .T. ) ;
#26772 = CIRCLE ( 'NONE', #44664, 251.4258649670780699 ) ;
#26773 = VERTEX_POINT ( 'NONE', #88788 ) ;
#26774 = CARTESIAN_POINT ( 'NONE',  ( -110.5895376238167387, -23.47596703998600631, 11.44779298504227683 ) ) ;
#26775 = DIRECTION ( 'NONE',  ( 1.000000000000000000, 0.000000000000000000, 0.000000000000000000 ) ) ;
#26776 = VECTOR ( 'NONE', #76240, 1000.000000000000114 ) ;
#26777 = CARTESIAN_POINT ( 'NONE',  ( -36.58084380204805086, -24.51419770103156637, 9.386484678747175181 ) ) ;
#26778 = CARTESIAN_POINT ( 'NONE',  ( 25.61870917940689196, -6.376774720514426953, 28.79814474876424768 ) ) ;
#26779 = EDGE_CURVE ( 'NONE', #99833, #80512, #32168, .T. ) ;
#26780 = CARTESIAN_POINT ( 'NONE',  ( 13.27039818535887505, -14.28956163997708906, -1.500000000000002220 ) ) ;
#26781 = CARTESIAN_POINT ( 'NONE',  ( 19.99082695160776169, -7.785253749782737209, -1.500000000000002220 ) ) ;
#26782 = CARTESIAN_POINT ( 'NONE',  ( -26.25707451207771470, -24.57999642328221768, 2.297367441281741751 ) ) ;
#26783 = LINE ( 'NONE', #41513, #92421 ) ;
#26784 = DIRECTION ( 'NONE',  ( 3.773278334444166432E-23, -1.000000000000000000, 0.000000000000000000 ) ) ;
#26785 = CARTESIAN_POINT ( 'NONE',  ( -19.53289989604362376, -11.71160353944097920, -1.500000000000002220 ) ) ;
#26786 = ADVANCED_FACE ( 'NONE', ( #4552 ), #21740, .F. ) ;
#26787 = CARTESIAN_POINT ( 'NONE',  ( 139.5443831022366226, -6.474179415928253967, 23.70558727230170959 ) ) ;
#26788 = CARTESIAN_POINT ( 'NONE',  ( -25.92875734969026524, -3.316774720514426456, -0.08597719988137648983 ) ) ;
#26789 = LINE ( 'NONE', #81580, #94594 ) ;
#26790 = CARTESIAN_POINT ( 'NONE',  ( -10.02925392579303576, -17.20239368982820238, 11.49999999999999645 ) ) ;
#26791 = DIRECTION ( 'NONE',  ( -1.000000000000000000, -0.000000000000000000, -0.000000000000000000 ) ) ;
#26792 = DIRECTION ( 'NONE',  ( -3.773278334453080206E-23, 0.9999999999976377785, 2.173523156925979975E-06 ) ) ;
#26793 = CARTESIAN_POINT ( 'NONE',  ( -76.55620429048340725, -23.47596703998600276, 11.44779298504227683 ) ) ;
#26794 = VERTEX_POINT ( 'NONE', #98369 ) ;
#26795 = CARTESIAN_POINT ( 'NONE',  ( -103.6228709571500701, -23.48783264082478794, -1.443836473390062158 ) ) ;
#26796 = DIRECTION ( 'NONE',  ( -1.889676989081488347E-15, 0.000000000000000000, -1.000000000000000000 ) ) ;
#26797 = EDGE_CURVE ( 'NONE', #47587, #10358, #67445, .T. ) ;
#26798 = CARTESIAN_POINT ( 'NONE',  ( 12.10466045530642631, 18.00204671274030233, 11.49999999999998934 ) ) ;
#26799 = CARTESIAN_POINT ( 'NONE',  ( -56.59303884526941175, -24.15620529776628445, 10.23563542870660648 ) ) ;
#26800 = CARTESIAN_POINT ( 'NONE',  ( -16.58133674543539371, -10.29093563426468450, -1.500000000000002220 ) ) ;
#26801 = CARTESIAN_POINT ( 'NONE',  ( -0.02075734969026423599, -5.965225279485572685, -0.08597719988137648983 ) ) ;
#26802 = ADVANCED_FACE ( 'NONE', ( #59835 ), #20249, .T. ) ;
#26803 = ORIENTED_EDGE ( 'NONE', *, *, #81296, .T. ) ;
#26804 = CALENDAR_DATE ( 2026, 9, 10 ) ;
#26805 = B_SPLINE_CURVE_WITH_KNOTS ( 'NONE', 3,
 ( #81692, #12164, #82180, #13159 ),
 .UNSPECIFIED., .F., .F.,
 ( 4, 4 ),
 ( 0.000000000000000000, 0.0001000000000000028644 ),
 .UNSPECIFIED. ) ;
#26806 = CIRCLE ( 'NONE', #70614, 0.8160000000000007248 ) ;
#26807 = DIRECTION ( 'NONE',  ( 0.2009441437208800141, 0.000000000000000000, -0.9796027006415827243 ) ) ;
#26808 = CARTESIAN_POINT ( 'NONE',  ( 19.60162835767302880, 5.811842276320244416, 11.49999999999999645 ) ) ;
#26809 = CARTESIAN_POINT ( 'NONE',  ( -40.62287095715005592, -29.50250786944525672, 11.44777988621624232 ) ) ;
#26810 = CARTESIAN_POINT ( 'NONE',  ( -22.05275734969026047, -0.3587747205144262708, 30.51402280011862089 ) ) ;
#26811 = EDGE_LOOP ( 'NONE', ( #7452, #2271, #5125, #8868, #87171, #7506, #43271, #64473, #41672, #31721, #90235, #16611, #2815, #47293, #62717, #36356 ) ) ;
#26812 = CARTESIAN_POINT ( 'NONE',  ( 9.950000000000006395, 0.000000000000000000, 18.35000000000000142 ) ) ;
#26813 = CARTESIAN_POINT ( 'NONE',  ( -39.46304919600096639, -25.28892577674529463, 4.009749604779731413 ) ) ;
#26814 = DIRECTION ( 'NONE',  ( 0.000000000000000000, 0.000000000000000000, 1.000000000000000000 ) ) ;
#26815 = CARTESIAN_POINT ( 'NONE',  ( -109.5521161159935275, -24.34968618360934300, 0.1864209137778879422 ) ) ;
#26816 = ORIENTED_EDGE ( 'NONE', *, *, #75566, .T. ) ;
#26817 = CARTESIAN_POINT ( 'NONE',  ( -79.73149462243459595, -25.14083923594767356, 2.947789366383930965 ) ) ;
#26818 = CARTESIAN_POINT ( 'NONE',  ( -5.713817535623205046, 22.21719745612757535, 11.49999999999999645 ) ) ;
#26819 = CARTESIAN_POINT ( 'NONE',  ( 21.04450177026006230, 8.645109164175620364, 11.49999999999998934 ) ) ;
#26820 = CARTESIAN_POINT ( 'NONE',  ( -71.04002682610065733, -25.08030589124952314, 7.384199749201091123 ) ) ;
#26821 = CARTESIAN_POINT ( 'NONE',  ( -40.52287095715005449, -24.62226745350442059, 0.9660975649729506287 ) ) ;
#26822 = CARTESIAN_POINT ( 'NONE',  ( -90.60545780893913559, -23.48783264082477018, -1.443836473390091912 ) ) ;
#26823 = DIRECTION ( 'NONE',  ( 1.000000000000000000, 0.000000000000000000, 0.000000000000000000 ) ) ;
#26824 = DIRECTION ( 'NONE',  ( -3.773278334444166432E-23, 1.000000000000000000, 0.000000000000000000 ) ) ;
#26825 = AXIS2_PLACEMENT_3D ( 'NONE', #95183, #95684, #57635 ) ;
#26826 = CARTESIAN_POINT ( 'NONE',  ( -9.708950231915746798, -19.59419465507263070, -1.500000000000002220 ) ) ;
#26827 = CARTESIAN_POINT ( 'NONE',  ( -74.52287095715011844, -24.33832256527049509, 0.1851278514138617326 ) ) ;
#26828 = AXIS2_PLACEMENT_3D ( 'NONE', #52424, #61037, #45801 ) ;
#26829 = B_SPLINE_CURVE_WITH_KNOTS ( 'NONE', 3,
 ( #81286, #20366, #98991, #97506 ),
 .UNSPECIFIED., .F., .F.,
 ( 4, 4 ),
 ( 0.000000000000000000, 9.999999999998897304E-05 ),
 .UNSPECIFIED. ) ;
#26830 = CARTESIAN_POINT ( 'NONE',  ( -103.5895376238167103, -24.66019654487199730, 8.947790411086115725 ) ) ;
#26831 = CARTESIAN_POINT ( 'NONE',  ( -120.6228709571500275, -23.84047902841603062, -0.8780736468305480047 ) ) ;
#26832 = CARTESIAN_POINT ( 'NONE',  ( 8.971512145086499856, -0.9999999999999991118, 3.746884140868835367 ) ) ;
#26833 = ORIENTED_EDGE ( 'NONE', *, *, #99800, .F. ) ;
#26834 = CARTESIAN_POINT ( 'NONE',  ( -10.82153711268468932, 17.32902648900640230, -1.500000000000002220 ) ) ;
#26835 = ORIENTED_EDGE ( 'NONE', *, *, #30956, .T. ) ;
#26836 = AXIS2_PLACEMENT_3D ( 'NONE', #77666, #15273, #68079 ) ;
#26837 = ORIENTED_EDGE ( 'NONE', *, *, #30640, .T. ) ;
#26838 = ORIENTED_EDGE ( 'NONE', *, *, #46477, .F. ) ;
#26839 = ORIENTED_EDGE ( 'NONE', *, *, #26163, .F. ) ;
#26840 = CARTESIAN_POINT ( 'NONE',  ( -19.18584950847915493, -12.73052202388904952, 11.49999999999998934 ) ) ;
#26841 = CARTESIAN_POINT ( 'NONE',  ( 17.91726403014145319, -0.5000000000000000000, -1.691563534834430227 ) ) ;
#26842 = CARTESIAN_POINT ( 'NONE',  ( -11.96439459519798554, -16.23097265130270728, -1.500000000000002220 ) ) ;
#26843 = ORIENTED_EDGE ( 'NONE', *, *, #87587, .T. ) ;
#26844 = FACE_OUTER_BOUND ( 'NONE', #84619, .T. ) ;
#26845 = CARTESIAN_POINT ( 'NONE',  ( 0.000000000000000000, -4.056774720514426669, 0.000000000000000000 ) ) ;
#26846 = AXIS2_PLACEMENT_3D ( 'NONE', #84746, #17, #8632 ) ;
#26847 = CARTESIAN_POINT ( 'NONE',  ( -85.62287095715005592, -29.50250786944525672, 11.44777988621623344 ) ) ;
#26848 = FACE_OUTER_BOUND ( 'NONE', #36321, .T. ) ;
#26850 = ORIENTED_EDGE ( 'NONE', *, *, #17701, .T. ) ;
#26849 = CARTESIAN_POINT ( 'NONE',  ( -21.18999663186871274, 2.814949255606389311, 11.49999999999999645 ) ) ;
#26851 = CARTESIAN_POINT ( 'NONE',  ( -111.9545715455114987, -29.50249917535260380, 7.447779886225679213 ) ) ;
#26852 = ORIENTED_EDGE ( 'NONE', *, *, #81984, .F. ) ;
#26853 = CARTESIAN_POINT ( 'NONE',  ( 10.43072250204971851, -19.66636941823637841, 11.49999999999998934 ) ) ;
#26854 = CARTESIAN_POINT ( 'NONE',  ( 0.1934390699377774303, 20.68474938276070318, -1.500000000000002220 ) ) ;
#26855 = ORIENTED_EDGE ( 'NONE', *, *, #4094, .F. ) ;
#26856 = CARTESIAN_POINT ( 'NONE',  ( 2.903846153846159517, -5.876774720514415407, 19.99999999999999289 ) ) ;
#26857 = ORIENTED_EDGE ( 'NONE', *, *, #70660, .F. ) ;
#26858 = ADVANCED_FACE ( 'NONE', ( #13133 ), #90272, .F. ) ;
#26859 = CARTESIAN_POINT ( 'NONE',  ( -56.52287095715005449, -23.47593901973090169, -1.443836447538996870 ) ) ;
#26860 = VERTEX_POINT ( 'NONE', #83650 ) ;
#26862 = EDGE_CURVE ( 'NONE', #91978, #61677, #5036, .T. ) ;
#26861 = CARTESIAN_POINT ( 'NONE',  ( 8.720681858489903959, -3.316774720514428232, -28.09278397295777197 ) ) ;
#26863 = CARTESIAN_POINT ( 'NONE',  ( -4.092705237139750984, -20.55955383578756113, -1.500000000000002220 ) ) ;
#26864 = CARTESIAN_POINT ( 'NONE',  ( -21.08706934527708654, 5.832127334627817739, 11.49999999999999645 ) ) ;
#26865 = EDGE_CURVE ( 'NONE', #22696, #73872, #59864, .T. ) ;
#26866 = CARTESIAN_POINT ( 'NONE',  ( -73.49608911756305929, -24.66019654487200441, 8.947790411086119278 ) ) ;
#26867 = CARTESIAN_POINT ( 'NONE',  ( -22.13300264024875119, -4.194623038110560032, 11.49999999999998934 ) ) ;
#26868 = EDGE_CURVE ( 'NONE', #36206, #65103, #20747, .T. ) ;
#26869 = CARTESIAN_POINT ( 'NONE',  ( 2.438461900574103502, 20.79476225230834174, 11.49999999999998934 ) ) ;
#26870 = CARTESIAN_POINT ( 'NONE',  ( -38.49809217028499830, -24.15543982623907127, -0.2315651400026569606 ) ) ;
#26871 = DIRECTION ( 'NONE',  ( -3.773278334453079030E-23, 0.9999999999976377785, 2.173523156925979128E-06 ) ) ;
#26872 = DIRECTION ( 'NONE',  ( 0.000000000000000000, 0.000000000000000000, -1.000000000000000000 ) ) ;
#26873 = CARTESIAN_POINT ( 'NONE',  ( -91.58953762381672448, -24.64965694238407323, 8.947790433994651238 ) ) ;
#26874 = ORIENTED_EDGE ( 'NONE', *, *, #54881, .T. ) ;
#26875 = CIRCLE ( 'NONE', #13891, 18.35000000000000142 ) ;
#26876 = ORIENTED_EDGE ( 'NONE', *, *, #34681, .F. ) ;
#26877 = VERTEX_POINT ( 'NONE', #28873 ) ;
#26878 = CARTESIAN_POINT ( 'NONE',  ( -52.49090493470863095, -24.51314013834315375, 0.6176544820404114011 ) ) ;
#26879 = ORIENTED_EDGE ( 'NONE', *, *, #67009, .T. ) ;
#26880 = CARTESIAN_POINT ( 'NONE',  ( -21.25412285906045895, 3.082840150875858054, -1.500000000000002220 ) ) ;
#26881 = VERTEX_POINT ( 'NONE', #21245 ) ;
#26882 = CARTESIAN_POINT ( 'NONE',  ( 0.06697178475903577122, -5.876774720514410077, 19.29815762497054976 ) ) ;
#26883 = CARTESIAN_POINT ( 'NONE',  ( 21.06685942672242362, 1.161445541649065882, -1.500000000000002220 ) ) ;
#26884 = CARTESIAN_POINT ( 'NONE',  ( -39.52287095715006870, -24.64965694238406613, 8.947790433994205372 ) ) ;
#26885 = CARTESIAN_POINT ( 'NONE',  ( 3.398286024651508530, -6.376774720514429617, 21.76255057507181334 ) ) ;
#26886 = CARTESIAN_POINT ( 'NONE',  ( -87.62287095715005592, -24.51283580621365132, 0.6167428607019791453 ) ) ;
#26887 = LINE ( 'NONE', #50234, #39344 ) ;
#26888 = CARTESIAN_POINT ( 'NONE',  ( -51.58953762381672448, -23.48786465467241413, 11.44779295918254824 ) ) ;
#26889 = CARTESIAN_POINT ( 'NONE',  ( 7.103389721457689099, 20.86620700561973862, -1.500000000000002220 ) ) ;
#26890 = ORIENTED_EDGE ( 'NONE', *, *, #81394, .T. ) ;
#26891 = CARTESIAN_POINT ( 'NONE',  ( -65.51285700265663081, -23.85049219812685806, 10.88485053497527311 ) ) ;
#26892 = CARTESIAN_POINT ( 'NONE',  ( -111.6228709571500559, -23.73934037231757799, 11.05740245334328087 ) ) ;
#26893 = CARTESIAN_POINT ( 'NONE',  ( 25.83488407601164383, -2.682774720514426559, -11.31196583263649735 ) ) ;
#26895 = B_SPLINE_CURVE_WITH_KNOTS ( 'NONE', 3,
 ( #49999, #47987, #72832, #11419, #80429 ),
 .UNSPECIFIED., .F., .F.,
 ( 4, 1, 4 ),
 ( 0.005748367439507872691, 0.007020066368101311738, 0.008291765296694749918 ),
 .UNSPECIFIED. ) ;
#26894 = CARTESIAN_POINT ( 'NONE',  ( -62.56627033263149684, -23.48786465467241058, 11.44779295918255002 ) ) ;
#26896 = CARTESIAN_POINT ( 'NONE',  ( -80.88924702628075636, -25.29868576439400840, 4.592921234843194256 ) ) ;
#26897 = DIRECTION ( 'NONE',  ( -4.472869286569340140E-16, -1.000000000000000000, 7.102795889480464408E-16 ) ) ;
#26898 = CARTESIAN_POINT ( 'NONE',  ( 17.14628872753620215, 12.71262973326862245, -1.500000000000002220 ) ) ;
#26899 = DIRECTION ( 'NONE',  ( 0.000000000000000000, -2.173523156925980399E-06, 0.9999999999976378895 ) ) ;
#26900 = CARTESIAN_POINT ( 'NONE',  ( -113.5228709571500616, -24.64965694238408034, 8.947790433994192938 ) ) ;
#26901 = CARTESIAN_POINT ( 'NONE',  ( -70.55620429048339304, -24.99156044556202616, 7.747789690856175859 ) ) ;
#26902 = CARTESIAN_POINT ( 'NONE',  ( -81.31047933837676567, -25.18365442479677796, 6.723090361430874573 ) ) ;
#26903 = CARTESIAN_POINT ( 'NONE',  ( 22.41689761077644860, -2.907977976681301424, -1.500000000000002220 ) ) ;
#26904 = AXIS2_PLACEMENT_3D ( 'NONE', #94203, #86098, #16576 ) ;
#26905 = CARTESIAN_POINT ( 'NONE',  ( -33.22287095715006444, -23.47596703998600276, 11.44779298504227683 ) ) ;
#26906 = EDGE_LOOP ( 'NONE', ( #45601, #49593, #774, #1971 ) ) ;
#26907 = AXIS2_PLACEMENT_3D ( 'NONE', #25504, #17896, #48858 ) ;
#26908 = CARTESIAN_POINT ( 'NONE',  ( 4.595037417369686850, -5.876774720514419847, 20.70846556543617467 ) ) ;
#26909 = CARTESIAN_POINT ( 'NONE',  ( -3.826923076923078426, -6.376774720514408301, 19.19230769230769695 ) ) ;
#26910 = CARTESIAN_POINT ( 'NONE',  ( 2.412641546452875208, 19.58572291230954221, 11.49999999999999645 ) ) ;
#26911 = CARTESIAN_POINT ( 'NONE',  ( 27.53860345374771867, -4.772774720514425972, -9.482392034746242260 ) ) ;
#26912 = VECTOR ( 'NONE', #19422, 1000.000000000000114 ) ;
#26913 = CARTESIAN_POINT ( 'NONE',  ( 7.749999999999998224, 24.84999999999999787, 2.100000000000000089 ) ) ;
#26914 = VERTEX_POINT ( 'NONE', #35497 ) ;
#26915 = AXIS2_PLACEMENT_3D ( 'NONE', #66990, #91793, #7065 ) ;
#26916 = CARTESIAN_POINT ( 'NONE',  ( -5.891025641025639636, -6.376774720514420736, 20.75510817307693046 ) ) ;
#26917 = CARTESIAN_POINT ( 'NONE',  ( -110.6228709571500559, -23.47593901973091235, -1.443836447538999312 ) ) ;
#26918 = CARTESIAN_POINT ( 'NONE',  ( -101.1189062734182755, -25.12268525518375739, 6.916461178196335879 ) ) ;
#26919 = CARTESIAN_POINT ( 'NONE',  ( -21.01067979154616694, 5.129389437380057259, 11.49999999999998934 ) ) ;
#26920 = DIRECTION ( 'NONE',  ( 0.000000000000000000, 0.000000000000000000, 1.000000000000000000 ) ) ;
#26922 = CARTESIAN_POINT ( 'NONE',  ( -16.26263985875334228, -10.51264992557365829, -1.500000000000002220 ) ) ;
#26921 = AXIS2_PLACEMENT_3D ( 'NONE', #83970, #67773, #75851 ) ;
#26923 = SHAPE_REPRESENTATION ( 'Plastic Part 2', ( #37391 ), #61811 ) ;
#26924 = CARTESIAN_POINT ( 'NONE',  ( -10.40290173325841216, -5.356774720514425603, 27.45402280011861862 ) ) ;
#26925 = CARTESIAN_POINT ( 'NONE',  ( -81.81116923543841324, -25.20690049807753041, 6.627235307510320972 ) ) ;
#26926 = ADVANCED_FACE ( 'NONE', ( #45112 ), #88814, .T. ) ;
#26927 = CARTESIAN_POINT ( 'NONE',  ( 9.697495225759652726, 17.24774500829319734, -1.500000000000002220 ) ) ;
#26928 = ORIENTED_EDGE ( 'NONE', *, *, #5510, .T. ) ;
#26929 = CARTESIAN_POINT ( 'NONE',  ( -0.6865706486018943178, -20.24796467851281179, 11.49999999999999645 ) ) ;
#26930 = CARTESIAN_POINT ( 'NONE',  ( 11.22265027772288093, 3.316774720514091612, -28.06709888818796017 ) ) ;
#26931 = ADVANCED_FACE ( 'NONE', ( #78022 ), #61336, .F. ) ;
#26932 = ORIENTED_EDGE ( 'NONE', *, *, #88943, .T. ) ;
#26933 = CARTESIAN_POINT ( 'NONE',  ( -37.52287095715007581, -23.96177878511307924, 10.65340807706330573 ) ) ;
#26934 = CARTESIAN_POINT ( 'NONE',  ( -20.27875734969026311, -6.143225279485574397, 24.00402280011862288 ) ) ;
#26935 = CARTESIAN_POINT ( 'NONE',  ( -31.62287095715005236, -23.48786465467240347, 11.44779295918255180 ) ) ;
#26936 = CARTESIAN_POINT ( 'NONE',  ( 8.499999999999989342, 18.74999999999999645, 2.100000000000000089 ) ) ;
#26937 = LINE ( 'NONE', #88847, #83505 ) ;
#26938 = CARTESIAN_POINT ( 'NONE',  ( 19.70663390988245922, 3.666079223618853966, -1.500000000000002220 ) ) ;
#26939 = CARTESIAN_POINT ( 'NONE',  ( -51.58953762381672448, -23.47596703998600276, 11.44779298504227505 ) ) ;
#26940 = ORIENTED_EDGE ( 'NONE', *, *, #30972, .T. ) ;
#26941 = CIRCLE ( 'NONE', #12364, 0.2999999999999981570 ) ;
#26942 = CARTESIAN_POINT ( 'NONE',  ( -50.34997525821440689, -25.31297217320124204, 4.735128272951183881 ) ) ;
#26943 = CARTESIAN_POINT ( 'NONE',  ( -35.53216495579373202, -24.63355581998385091, 0.9682620441944008727 ) ) ;
#26944 = CARTESIAN_POINT ( 'NONE',  ( -79.76418533285618651, -25.30522694008003270, 5.133764971034367797 ) ) ;
#26945 = DIRECTION ( 'NONE',  ( 0.000000000000000000, 1.000000000000000000, 4.336808689942019708E-16 ) ) ;
#26946 = CARTESIAN_POINT ( 'NONE',  ( -73.64404266222578599, -23.73766607897670511, -1.055555164236457344 ) ) ;
#26947 = CARTESIAN_POINT ( 'NONE',  ( 15.01911467442486625, 4.015204461132062974, -28.37592028203548011 ) ) ;
#26948 = CARTESIAN_POINT ( 'NONE',  ( 22.81105451610979173, -500000.0000000000582, -20.71691820600746681 ) ) ;
#26949 = VERTEX_POINT ( 'NONE', #32370 ) ;
#26950 = CARTESIAN_POINT ( 'NONE',  ( 15.76184642470745700, 12.85868457875834103, -1.500000000000002220 ) ) ;
#26951 = ORIENTED_EDGE ( 'NONE', *, *, #61948, .T. ) ;
#26952 = CARTESIAN_POINT ( 'NONE',  ( -22.92702450682246251, 0.3551139841105944162, -1.500000000000002220 ) ) ;
#26953 = CARTESIAN_POINT ( 'NONE',  ( 31.60706529141451426, 6.376774720514427841, 26.12024523944107557 ) ) ;
#26954 = ORIENTED_EDGE ( 'NONE', *, *, #32989, .F. ) ;
#26955 = CARTESIAN_POINT ( 'NONE',  ( 6.660000000000001030, -10.77121780415746599, 1.154761385154455366 ) ) ;
#26956 = AXIS2_PLACEMENT_3D ( 'NONE', #83566, #35422, #29288 ) ;
#26957 = CARTESIAN_POINT ( 'NONE',  ( -49.74873825466967503, -25.12215384875874591, 6.941713980050353783 ) ) ;
#26958 = LINE ( 'NONE', #57932, #65903 ) ;
#26959 = CARTESIAN_POINT ( 'NONE',  ( 0.06830352742921809439, -21.21198074455918814, 11.49999999999999645 ) ) ;
#26960 = CARTESIAN_POINT ( 'NONE',  ( -21.14055147415990277, -6.693858341896442354, 11.49999999999998934 ) ) ;
#26961 = CARTESIAN_POINT ( 'NONE',  ( -7.762539992054180438, 19.06225842855939234, -1.500000000000002220 ) ) ;
#26962 = VECTOR ( 'NONE', #91439, 1000.000000000000000 ) ;
#26963 = VERTEX_POINT ( 'NONE', #23747 ) ;
#26964 = CARTESIAN_POINT ( 'NONE',  ( -104.5228709571500758, -29.50250243563736774, 8.947779886222138046 ) ) ;
#26965 = VERTEX_POINT ( 'NONE', #70944 ) ;
#26966 = CARTESIAN_POINT ( 'NONE',  ( -54.56747232805444270, -23.48783264082476663, -1.443836473390098130 ) ) ;
#26967 = CARTESIAN_POINT ( 'NONE',  ( -126.6228709571500559, -23.73934037231758509, 11.05740245334328264 ) ) ;
#26968 = ORIENTED_EDGE ( 'NONE', *, *, #23039, .F. ) ;
#26969 = VECTOR ( 'NONE', #31700, 1000.000000000000114 ) ;
#26971 = ORIENTED_EDGE ( 'NONE', *, *, #51179, .T. ) ;
#26970 = EDGE_CURVE ( 'NONE', #25591, #22543, #31368, .T. ) ;
#26972 = CIRCLE ( 'NONE', #96653, 2.499999999999993339 ) ;
#26973 = ORIENTED_EDGE ( 'NONE', *, *, #70660, .T. ) ;
#26974 = CARTESIAN_POINT ( 'NONE',  ( -27.96875734969026084, -6.143225279485574397, 23.50402280011861933 ) ) ;
#26975 = FACE_OUTER_BOUND ( 'NONE', #25644, .T. ) ;
#26976 = CARTESIAN_POINT ( 'NONE',  ( 5.557675543255346184, -6.376774720514415407, 20.10561748372801461 ) ) ;
#26977 = CARTESIAN_POINT ( 'NONE',  ( -20.31193019649481357, 4.361987795224258946, -1.500000000000002220 ) ) ;
#26978 = CARTESIAN_POINT ( 'NONE',  ( -20.31635052000798325, -7.690577546848336610, 11.49999999999999645 ) ) ;
#26979 = ORIENTED_EDGE ( 'NONE', *, *, #59066, .F. ) ;
#26980 = ADVANCED_FACE ( 'NONE', ( #418 ), #39488, .T. ) ;
#26981 = LINE ( 'NONE', #56950, #19065 ) ;
#26982 = CARTESIAN_POINT ( 'NONE',  ( -115.5889431145695028, -24.63355581998384736, 0.9682620441943983192 ) ) ;
#26983 = CARTESIAN_POINT ( 'NONE',  ( 20.99545381566289137, 7.807860396396394620, 11.49999999999998934 ) ) ;
#26984 = AXIS2_PLACEMENT_3D ( 'NONE', #99781, #75458, #5958 ) ;
#26985 = B_SPLINE_CURVE_WITH_KNOTS ( 'NONE', 3,
 ( #77236, #93469, #7743, #38689, #76245, #69655 ),
 .UNSPECIFIED., .F., .F.,
 ( 4, 2, 4 ),
 ( 1.570755371634150632E-05, 0.001396183895866089488, 0.002776660238015837747 ),
 .UNSPECIFIED. ) ;
#26986 = EDGE_CURVE ( 'NONE', #77983, #56862, #90041, .T. ) ;
#26987 = B_SPLINE_CURVE_WITH_KNOTS ( 'NONE', 3,
 ( #11952, #89584, #42923, #80971, #34802, #20064 ),
 .UNSPECIFIED., .F., .F.,
 ( 4, 2, 4 ),
 ( 0.000000000000000000, 0.001380901958385389412, 0.002761803916770778824 ),
 .UNSPECIFIED. ) ;
#26988 = CARTESIAN_POINT ( 'NONE',  ( -99.52287095715006160, -29.50250243563736774, 8.947779886222138046 ) ) ;
#26989 = CARTESIAN_POINT ( 'NONE',  ( -61.58953762381672448, -24.64965694238574656, 8.947790433994201820 ) ) ;
#26990 = VERTEX_POINT ( 'NONE', #86155 ) ;
#26991 = CARTESIAN_POINT ( 'NONE',  ( -31.62287095715005236, -23.48786465467240347, 11.44779295918255180 ) ) ;
#26992 = CARTESIAN_POINT ( 'NONE',  ( 12.17747153392518733, -4.565036639100802596, -27.62487831441275787 ) ) ;
#26993 = EDGE_CURVE ( 'NONE', #55188, #86370, #85179, .T. ) ;
#26994 = ORIENTED_EDGE ( 'NONE', *, *, #77524, .F. ) ;
#26995 = EDGE_CURVE ( 'NONE', #16519, #87155, #31876, .T. ) ;
#26996 = EDGE_LOOP ( 'NONE', ( #65253, #94118, #29447, #39360 ) ) ;
#26997 = FACE_OUTER_BOUND ( 'NONE', #26116, .T. ) ;
#26998 = VERTEX_POINT ( 'NONE', #7529 ) ;
#26999 = CARTESIAN_POINT ( 'NONE',  ( -21.08860491664495029, 2.407354197416772035, -1.500000000000002220 ) ) ;
#27000 = EDGE_LOOP ( 'NONE', ( #58706, #69823, #86141, #89642 ) ) ;
#27001 = CARTESIAN_POINT ( 'NONE',  ( -68.62287095715005592, -24.65952944569304606, 1.056160979905698794 ) ) ;
#27002 = CARTESIAN_POINT ( 'NONE',  ( 4.919149715316761373, 21.27959583485438344, -1.500000000000002220 ) ) ;
#27003 = CARTESIAN_POINT ( 'NONE',  ( -103.5477529696951819, -24.66019654487200086, 8.947790411086115725 ) ) ;
#27004 = CARTESIAN_POINT ( 'NONE',  ( -21.72567761722203628, 6.514095075961352954, -1.500000000000002220 ) ) ;
#27005 = CARTESIAN_POINT ( 'NONE',  ( -125.5228709571500616, -25.00182538069146077, 7.747789668545104647 ) ) ;
#27006 = CARTESIAN_POINT ( 'NONE',  ( -24.90875734969025501, -5.965225279485572685, 26.43402280011862615 ) ) ;
#27007 = CARTESIAN_POINT ( 'NONE',  ( -20.59625928752216240, -7.366027188055905839, -1.500000000000002220 ) ) ;
#27008 = CARTESIAN_POINT ( 'NONE',  ( -55.52287095715006870, -25.00182538069145011, 7.747789668545106423 ) ) ;
#27009 = VERTEX_POINT ( 'NONE', #23240 ) ;
#27010 = EDGE_CURVE ( 'NONE', #51976, #44200, #97411, .T. ) ;
#27011 = CARTESIAN_POINT ( 'NONE',  ( -65.62287095715002749, -23.85196035786901092, -0.8779234886474904798 ) ) ;
#27012 = DIRECTION ( 'NONE',  ( -1.000000000000000000, -3.773278334444167608E-23, -8.201307833595939069E-29 ) ) ;
#27013 = AXIS2_PLACEMENT_3D ( 'NONE', #40463, #71412, #25222 ) ;
#27014 = EDGE_LOOP ( 'NONE', ( #15758, #45682, #59802, #56323 ) ) ;
#27015 = CARTESIAN_POINT ( 'NONE',  ( -30.60882031961203253, -24.47943607710057634, 0.5667427426393205625 ) ) ;
#27016 = ORIENTED_EDGE ( 'NONE', *, *, #61772, .T. ) ;
#27017 = CARTESIAN_POINT ( 'NONE',  ( 30.53060340732036337, -5.329285123471891872, 3.289350009555732868 ) ) ;
#27018 = AXIS2_PLACEMENT_3D ( 'NONE', #49996, #11416, #80425 ) ;
#27019 = CARTESIAN_POINT ( 'NONE',  ( -0.06470660251384131867, -22.21232218138523606, 0.8294870405985470541 ) ) ;
#27020 = CARTESIAN_POINT ( 'NONE',  ( -0.06837171988653999166, -21.26218376953697486, 11.49999999999998934 ) ) ;
#27021 = CARTESIAN_POINT ( 'NONE',  ( -7.641025641025641413, -5.876774720514418071, 20.36458333333334636 ) ) ;
#27022 = CARTESIAN_POINT ( 'NONE',  ( -26.09929425038925999, -24.75186500840231218, 4.716438697959393522 ) ) ;
#27023 = DIRECTION ( 'NONE',  ( 0.000000000000000000, 2.173523156925980399E-06, -0.9999999999976378895 ) ) ;
#27024 = CARTESIAN_POINT ( 'NONE',  ( -31.24388727629348494, -29.50248678627064081, 1.747779886239157809 ) ) ;
#27025 = CARTESIAN_POINT ( 'NONE',  ( -117.6281512103715272, -23.73791477778912551, 11.05961554403169878 ) ) ;
#27026 = ORIENTED_EDGE ( 'NONE', *, *, #30299, .T. ) ;
#27027 = CARTESIAN_POINT ( 'NONE',  ( 19.26631176993168282, 3.279242639417544236, 11.49999999999999645 ) ) ;
#27028 = CARTESIAN_POINT ( 'NONE',  ( -5.382328594919684406, -6.376774720514413630, 19.61227901093090864 ) ) ;
#27029 = CARTESIAN_POINT ( 'NONE',  ( -55.62287095715004881, -23.48783264082478084, -1.443836473390068820 ) ) ;
#27030 = EDGE_CURVE ( 'NONE', #17929, #67306, #48892, .T. ) ;
#27031 = ORIENTED_EDGE ( 'NONE', *, *, #62408, .T. ) ;
#27032 = CARTESIAN_POINT ( 'NONE',  ( 3.825380556292953482, -5.876774720514426953, 21.83927723428477208 ) ) ;
#27033 = CARTESIAN_POINT ( 'NONE',  ( -100.4498239493576648, -25.03284467579916495, 7.563174216508126158 ) ) ;
#27034 = AXIS2_PLACEMENT_3D ( 'NONE', #32529, #55888, #95432 ) ;
#27035 = DIRECTION ( 'NONE',  ( 0.000000000000000000, 1.000000000000000000, 0.000000000000000000 ) ) ;
#27036 = ADVANCED_FACE ( 'NONE', ( #54224 ), #47608, .F. ) ;
#27037 = CARTESIAN_POINT ( 'NONE',  ( -32.07722060962682775, -29.50250091417111520, 8.247779886223803203 ) ) ;
#27038 = CARTESIAN_POINT ( 'NONE',  ( -5.193715590271882121, 18.98282465337476665, 11.49999999999998934 ) ) ;
#27039 = EDGE_LOOP ( 'NONE', ( #28585, #19912, #65806, #20231 ) ) ;
#27040 = DIRECTION ( 'NONE',  ( -3.773278334453079618E-23, 0.9999999999976377785, 2.173523156925979975E-06 ) ) ;
#27041 = CARTESIAN_POINT ( 'NONE',  ( -42.62287095715004881, -24.66019654487199020, 8.947790411086135265 ) ) ;
#27042 = B_SPLINE_CURVE_WITH_KNOTS ( 'NONE', 3,
 ( #97627, #59088, #82403, #43855, #41870, #19007, #20995, #29610, #5780, #37726, #15377, #68686, #84400, #91506, #14880, #36243 ),
 .UNSPECIFIED., .F., .F.,
 ( 4, 2, 2, 2, 2, 2, 2, 4 ),
 ( 0.000000000000000000, 0.0003118279254866530067, 0.0006236558509733060134, 0.0009354837764599591285, 0.001247311701946612027, 0.001870967552919916305, 0.002182795478406559988, 0.002494623403893203670 ),
 .UNSPECIFIED. ) ;
#27043 = AXIS2_PLACEMENT_3D ( 'NONE', #55676, #7977, #48052 ) ;
#27044 = APPROVAL_DATE_TIME ( #20909, #90973 ) ;
#27045 = ADVANCED_FACE ( 'NONE', ( #77530 ), #61835, .T. ) ;
#27046 = ORIENTED_EDGE ( 'NONE', *, *, #41009, .T. ) ;
#27047 = PLANE ( 'NONE',  #75910 ) ;
#27048 = DIRECTION ( 'NONE',  ( 0.6599726524652350657, 0.000000000000000000, -0.7512896232465892110 ) ) ;
#27049 = DIRECTION ( 'NONE',  ( 1.000000000000000000, 3.773278334444166432E-23, 8.201307841325785021E-29 ) ) ;
#27050 = CARTESIAN_POINT ( 'NONE',  ( -105.6228709571500559, -23.48786465467241769, 11.44779295918253759 ) ) ;
#27051 = DIRECTION ( 'NONE',  ( 0.000000000000000000, 0.9999999999976377785, 2.173523156925979975E-06 ) ) ;
#27052 = VECTOR ( 'NONE', #15499, 1000.000000000000114 ) ;
#27053 = AXIS2_PLACEMENT_3D ( 'NONE', #73676, #59962, #50847 ) ;
#27054 = DIRECTION ( 'NONE',  ( -1.000000000000000000, -3.773278334444167608E-23, -8.201307833595939069E-29 ) ) ;
#27055 = CARTESIAN_POINT ( 'NONE',  ( -50.62287095715006302, -24.91544648472619272, 1.928969306349232804 ) ) ;
#27056 = CARTESIAN_POINT ( 'NONE',  ( 13.89251353435424363, -14.32104260081073832, -1.500000000000002220 ) ) ;
#27057 = EDGE_CURVE ( 'NONE', #65344, #29538, #15091, .T. ) ;
#27058 = CARTESIAN_POINT ( 'NONE',  ( -0.01312681704450994330, -22.88006303776501582, 7.008493951326582483 ) ) ;
#27059 = CARTESIAN_POINT ( 'NONE',  ( -4.768723929037996356, 19.30091236029735668, -1.500000000000002220 ) ) ;
#27060 = VERTEX_POINT ( 'NONE', #38978 ) ;
#27061 = AXIS2_PLACEMENT_3D ( 'NONE', #26525, #1691, #57490 ) ;
#27062 = CARTESIAN_POINT ( 'NONE',  ( 20.13489193910630703, -2.682774720514426559, -22.92085183005112370 ) ) ;
#27063 = CARTESIAN_POINT ( 'NONE',  ( -72.52287095715007581, -24.64898659630367916, 1.056161002820824368 ) ) ;
#27064 = CARTESIAN_POINT ( 'NONE',  ( 10.86431179149619908, -3.316774720514763075, -28.05678185015766246 ) ) ;
#27065 = CARTESIAN_POINT ( 'NONE',  ( -20.46667790307254009, -3.548193229090686796, 11.49999999999999645 ) ) ;
#27066 = CARTESIAN_POINT ( 'NONE',  ( -7.617563585130437076, -6.376774720514411854, 19.95084900476494383 ) ) ;
#27067 = B_SPLINE_CURVE_WITH_KNOTS ( 'NONE', 3,
 ( #74877, #97233, #82497, #82007 ),
 .UNSPECIFIED., .F., .F.,
 ( 4, 4 ),
 ( 0.1906361285931100769, 0.1996425598652254996 ),
 .UNSPECIFIED. ) ;
#27068 = CC_DESIGN_DATE_AND_TIME_ASSIGNMENT ( #10959, #49036, ( #19911 ) ) ;
#27069 = CARTESIAN_POINT ( 'NONE',  ( -92.52287095715006160, -23.47596703998600631, 11.44779298504228393 ) ) ;
#27070 = CARTESIAN_POINT ( 'NONE',  ( -22.57016884136470125, -3.422276288085174478, 11.49999999999999645 ) ) ;
#27071 = ORIENTED_EDGE ( 'NONE', *, *, #66812, .T. ) ;
#27072 = CARTESIAN_POINT ( 'NONE',  ( -64.62287095715011276, -24.34917612406838572, 0.1852690917426601802 ) ) ;
#27073 = FACE_OUTER_BOUND ( 'NONE', #23977, .T. ) ;
#27074 = ORIENTED_EDGE ( 'NONE', *, *, #45870, .T. ) ;
#27075 = CARTESIAN_POINT ( 'NONE',  ( 9.769481717609929561, -17.74358427669893956, 11.49999999999998934 ) ) ;
#27076 = DIRECTION ( 'NONE',  ( -0.000000000000000000, -0.000000000000000000, 1.000000000000000000 ) ) ;
#27077 = CARTESIAN_POINT ( 'NONE',  ( 3.176458874063926352, 5.965225279485592225, -28.85257003503889095 ) ) ;
#27078 = VECTOR ( 'NONE', #55334, 1000.000000000000000 ) ;
#27079 = FACE_OUTER_BOUND ( 'NONE', #90034, .T. ) ;
#27080 = ORIENTED_EDGE ( 'NONE', *, *, #58250, .T. ) ;
#27081 = CARTESIAN_POINT ( 'NONE',  ( -79.44990853704386780, -25.30595284857920291, 5.490744999806991267 ) ) ;
#27082 = CARTESIAN_POINT ( 'NONE',  ( -46.52287095715006160, -23.72773821059536914, 11.05748984161097326 ) ) ;
#27083 = CARTESIAN_POINT ( 'NONE',  ( 20.02521558760690112, -0.9251608499524575091, -1.500000000000002220 ) ) ;
#27084 = CARTESIAN_POINT ( 'NONE',  ( 18.99863377428308198, 9.053671573812124507, 11.49999999999999645 ) ) ;
#27085 = VECTOR ( 'NONE', #35520, 1000.000000000000000 ) ;
#27086 = CARTESIAN_POINT ( 'NONE',  ( -54.62287095715004881, -23.73934037231756022, 11.05740245334329508 ) ) ;
#27087 = DIRECTION ( 'NONE',  ( 0.000000000000000000, 0.000000000000000000, -1.000000000000000000 ) ) ;
#27088 = CARTESIAN_POINT ( 'NONE',  ( 21.39010012190943755, 5.354582491813655309, -1.500000000000002220 ) ) ;
#27089 = CARTESIAN_POINT ( 'NONE',  ( -39.78092788824959314, -25.31589286589048982, 4.883081598822826663 ) ) ;
#27090 = CARTESIAN_POINT ( 'NONE',  ( -60.52287095715006160, -24.99132157543083821, 2.256160258750667502 ) ) ;
#27091 = DIRECTION ( 'NONE',  ( -0.000000000000000000, 1.000000000000000000, -0.000000000000000000 ) ) ;
#27092 = CARTESIAN_POINT ( 'NONE',  ( -90.25937923781920347, -25.27880950044345454, 5.947789066509451494 ) ) ;
#27093 = CARTESIAN_POINT ( 'NONE',  ( -31.62287095715005236, -23.73907113216990439, -1.053371485793236362 ) ) ;
#27094 = ORIENTED_EDGE ( 'NONE', *, *, #69201, .F. ) ;
#27095 = VERTEX_POINT ( 'NONE', #26762 ) ;
#27096 = ADVANCED_FACE ( 'NONE', ( #57725 ), #71448, .F. ) ;
#27097 = DIRECTION ( 'NONE',  ( 3.773278334444167608E-23, -1.000000000000000000, 0.000000000000000000 ) ) ;
#27098 = CARTESIAN_POINT ( 'NONE',  ( -89.55620429048339304, -23.48786465467241058, 11.44779295918253936 ) ) ;
#27099 = LINE ( 'NONE', #65686, #45510 ) ;
#27100 = CARTESIAN_POINT ( 'NONE',  ( -1.452656003914881477, -20.50939586048694352, -1.500000000000002220 ) ) ;
#27101 = ORIENTED_EDGE ( 'NONE', *, *, #97455, .T. ) ;
#27102 = DIRECTION ( 'NONE',  ( -0.000000000000000000, 1.000000000000000000, -0.000000000000000000 ) ) ;
#27103 = DIRECTION ( 'NONE',  ( 0.000000000000000000, -1.000000000000000000, 0.000000000000000000 ) ) ;
#27104 = CARTESIAN_POINT ( 'NONE',  ( -80.43221577628075636, -25.31553502933635968, 4.967019755914117596 ) ) ;
#27105 = CARTESIAN_POINT ( 'NONE',  ( -21.16112330106665240, 7.131417522999676351, 11.49999999999998934 ) ) ;
#27106 = VECTOR ( 'NONE', #56366, 1000.000000000000114 ) ;
#27107 = DIRECTION ( 'NONE',  ( -0.000000000000000000, -1.000000000000000000, -0.000000000000000000 ) ) ;
#27108 = CARTESIAN_POINT ( 'NONE',  ( -124.6228709571500559, -23.48783264082479505, -1.443836473390058828 ) ) ;
#27109 = ORIENTED_EDGE ( 'NONE', *, *, #24340, .T. ) ;
#27110 = CARTESIAN_POINT ( 'NONE',  ( -32.50560601784287229, -24.86181184613565165, 1.747789954104514987 ) ) ;
#27111 = CARTESIAN_POINT ( 'NONE',  ( -91.62287095715005592, -23.48786465467241769, 11.44779295918254114 ) ) ;
#27112 = EDGE_CURVE ( 'NONE', #2990, #18856, #22275, .T. ) ;
#27113 = CARTESIAN_POINT ( 'NONE',  ( 20.25184064777635484, 4.944226511633750043, -1.500000000000002220 ) ) ;
#27114 = EDGE_CURVE ( 'NONE', #46643, #31571, #17144, .T. ) ;
#27115 = ORIENTED_EDGE ( 'NONE', *, *, #7663, .T. ) ;
#27117 = ORIENTED_EDGE ( 'NONE', *, *, #49399, .T. ) ;
#27116 = CARTESIAN_POINT ( 'NONE',  ( 14.61581676223891613, -3.582999323269832725, -27.35847991879931485 ) ) ;
#27118 = VECTOR ( 'NONE', #84851, 1000.000000000000000 ) ;
#27120 = ORIENTED_EDGE ( 'NONE', *, *, #95271, .F. ) ;
#27119 = PERSON ( 'NAUO-PER10', 'UNSPECIFIED', 'UNSPECIFIED', ('UNSPECIFIED'), ('UNSPECIFIED'), ('UNSPECIFIED') ) ;
#27121 = CARTESIAN_POINT ( 'NONE',  ( -120.6228709571500417, -29.50247984919015209, -1.443849546365046699 ) ) ;
#27122 = CARTESIAN_POINT ( 'NONE',  ( -16.00611555608923098, 13.71732778110762219, -1.500000000000002220 ) ) ;
#27123 = ORIENTED_EDGE ( 'NONE', *, *, #91036, .T. ) ;
#27124 = CARTESIAN_POINT ( 'NONE',  ( -27.13414387080440093, -5.965225279485594001, -10.21530720150730254 ) ) ;
#27125 = CARTESIAN_POINT ( 'NONE',  ( -48.87380231474225667, -25.25252557466923520, 6.137092008254006359 ) ) ;
#27126 = CARTESIAN_POINT ( 'NONE',  ( -120.5173578655454918, -24.73531770709095312, 8.716586749053508498 ) ) ;
#27127 = AXIS2_PLACEMENT_3D ( 'NONE', #38984, #37989, #15145 ) ;
#27128 = CARTESIAN_POINT ( 'NONE',  ( -76.59214368814321006, -24.15620529776628089, 10.23563542870660470 ) ) ;
#27129 = B_SPLINE_CURVE_WITH_KNOTS ( 'NONE', 3,
 ( #40769, #9307, #96552, #32652, #71730, #34168 ),
 .UNSPECIFIED., .F., .F.,
 ( 4, 2, 4 ),
 ( 6.384118678618878472E-06, 0.001386860460828378888, 0.002767336802978138856 ),
 .UNSPECIFIED. ) ;
#27130 = CARTESIAN_POINT ( 'NONE',  ( -118.6228709571500559, -24.64965695001469115, 8.947790433994175174 ) ) ;
#27131 = CARTESIAN_POINT ( 'NONE',  ( 21.66353188042378974, 1.267531592894010739, -1.500000000000002220 ) ) ;
#27132 = CARTESIAN_POINT ( 'NONE',  ( -80.52846833935618065, -25.24759804693422893, 7.100555191934691202 ) ) ;
#27134 = ORIENTED_EDGE ( 'NONE', *, *, #49541, .F. ) ;
#27133 = CARTESIAN_POINT ( 'NONE',  ( 2.725811458822067657, 22.07344620009914138, 11.49999999999999645 ) ) ;
#27135 = ADVANCED_FACE ( 'NONE', ( #27268 ), #81047, .F. ) ;
#27136 = LINE ( 'NONE', #58099, #4860 ) ;
#27137 = CARTESIAN_POINT ( 'NONE',  ( 15.32675665358028283, 3.579156900695799060, -27.14457288197743878 ) ) ;
#27138 = DIRECTION ( 'NONE',  ( -3.773278334453079030E-23, 0.9999999999976377785, 2.173523156925979128E-06 ) ) ;
#27139 = EDGE_LOOP ( 'NONE', ( #18181, #28513, #35946, #34150 ) ) ;
#27141 = ORIENTED_EDGE ( 'NONE', *, *, #27342, .T. ) ;
#27140 = DIRECTION ( 'NONE',  ( -3.773278334453079618E-23, 0.9999999999976377785, 2.173523156925979975E-06 ) ) ;
#27142 = ORIENTED_EDGE ( 'NONE', *, *, #75566, .F. ) ;
#27143 = CARTESIAN_POINT ( 'NONE',  ( -95.55620429048339304, -24.99156044556202261, 7.747789690856174083 ) ) ;
#27144 = B_SPLINE_CURVE_WITH_KNOTS ( 'NONE', 3,
 ( #53607, #7400, #57606, #48991 ),
 .UNSPECIFIED., .F., .F.,
 ( 4, 4 ),
 ( 0.2689542867207789789, 0.2699550337615441720 ),
 .UNSPECIFIED. ) ;
#27145 = CARTESIAN_POINT ( 'NONE',  ( -49.22466177438518287, -25.30474062507557065, 4.482496648232663361 ) ) ;
#27146 = CARTESIAN_POINT ( 'NONE',  ( -28.98875734969026041, 5.965225279485572685, 15.62202280011862321 ) ) ;
#27147 = CARTESIAN_POINT ( 'NONE',  ( -105.5228709571501184, -24.83602698348160942, 1.605859176311261294 ) ) ;
#27148 = VERTEX_POINT ( 'NONE', #32880 ) ;
#27150 =( BOUNDED_SURFACE ( )  B_SPLINE_SURFACE ( 3, 2, ( 
 ( #77717, #1121, #32058 ),
 ( #93955, #55920, #85340 ),
 ( #24444, #86841, #17337 ),
 ( #69633, #79230, #9729 ),
 ( #2135, #33070, #92947 ),
 ( #80747, #81240, #88358 ),
 ( #11230, #42207, #82233 ),
 ( #3135, #73139, #74132 ),
 ( #49816, #3630, #81740 ),
 ( #2629, #65547, #64549 ),
 ( #19823, #34579, #96464 ),
 ( #65049, #4124, #89356 ),
 ( #50304, #41186, #50801 ),
 ( #41699, #95462, #72143 ),
 ( #95966, #19335, #12215 ),
 ( #33571, #26953, #4625 ) ),
 .UNSPECIFIED., .F., .F., .T. ) 
 B_SPLINE_SURFACE_WITH_KNOTS ( ( 4, 2, 2, 2, 2, 2, 2, 4 ),
 ( 3, 3 ),
 ( 5.963111948670274387E-19, 0.0002402527847056124086, 0.0004805055694112242209, 0.0007207583541168360603, 0.0009610111388224478997, 0.001201263923528059739, 0.001441516708233671470, 0.001922022277644895149 ),
 ( 0.000000000000000000, 1.000000000000000000 ),
 .UNSPECIFIED. ) 
 GEOMETRIC_REPRESENTATION_ITEM ( )  RATIONAL_B_SPLINE_SURFACE ( (
 ( 1.000000000000000000, 0.6532382444175202085, 1.000000000000000000),
 ( 1.000000000000000000, 0.6532394276814369460, 1.000000000000000000),
 ( 1.000000000000000000, 0.6536213453767286685, 1.000000000000000000),
 ( 1.000000000000000000, 0.6551141999105375424, 1.000000000000000000),
 ( 1.000000000000000000, 0.6562426621441458385, 1.000000000000000000),
 ( 1.000000000000000000, 0.6591574828660696772, 1.000000000000000000),
 ( 1.000000000000000000, 0.6609310395923536641, 1.000000000000000000),
 ( 1.000000000000000000, 0.6650742797341039347, 1.000000000000000000),
 ( 1.000000000000000000, 0.6674600455424170020, 1.000000000000000000),
 ( 1.000000000000000000, 0.6725980719960679144, 1.000000000000000000),
 ( 1.000000000000000000, 0.6753708636379929242, 1.000000000000000000),
 ( 1.000000000000000000, 0.6813027919944147914, 1.000000000000000000),
 ( 1.000000000000000000, 0.6844015431888567091, 1.000000000000000000),
 ( 1.000000000000000000, 0.6938890553659712301, 1.000000000000000000),
 ( 1.000000000000000000, 0.7006220437376852184, 1.000000000000000000),
 ( 1.000000000000000000, 0.7071067811865475727, 1.000000000000000000) ) ) 
 REPRESENTATION_ITEM ( '' )  SURFACE ( )  );
#27149 = CARTESIAN_POINT ( 'NONE',  ( -130.5728709571500872, -25.30388856787854479, 6.584556770830782391 ) ) ;
#27151 = CARTESIAN_POINT ( 'NONE',  ( -22.46026885398333661, -0.8929446408661095846, -1.500000000000002220 ) ) ;
#27152 = ORIENTED_EDGE ( 'NONE', *, *, #1607, .T. ) ;
#27153 = CARTESIAN_POINT ( 'NONE',  ( -81.52287095715007581, -23.73934037231757088, 11.05740245334329153 ) ) ;
#27154 = CARTESIAN_POINT ( 'NONE',  ( -101.5089391001824310, -24.66019654487200086, 8.947790411086115725 ) ) ;
#27155 = CARTESIAN_POINT ( 'NONE',  ( 9.131215498121711960, 5.356774720514425603, -25.00673578072587588 ) ) ;
#27156 = VECTOR ( 'NONE', #63346, 1000.000000000000000 ) ;
#27157 = CARTESIAN_POINT ( 'NONE',  ( -125.5228709571500616, -24.83602698348235904, 1.605859176313918946 ) ) ;
#27158 = CARTESIAN_POINT ( 'NONE',  ( -130.5728709571501156, -25.30558673197061736, 5.002395802403323266 ) ) ;
#27159 = ADVANCED_FACE ( 'NONE', ( #42505 ), #11037, .T. ) ;
#27160 = CARTESIAN_POINT ( 'NONE',  ( -7.889300446747370188, -17.95381117360125955, -1.500000000000002220 ) ) ;
#27161 = B_SPLINE_SURFACE_WITH_KNOTS ( 'NONE', 3, 3, ( 
 ( #62871, #84674, #91777, #22260 ),
 ( #99879, #53242, #85175, #68461 ),
 ( #15160, #100378, #440, #76056 ),
 ( #29891, #77550, #46127, #16162 ),
 ( #22759, #77053, #31393, #76546 ),
 ( #85682, #30891, #93787, #83674 ),
 ( #46632, #47130, #24283, #7054 ) ),
 .UNSPECIFIED., .F., .F., .F.,
 ( 4, 3, 4 ),
 ( 4, 4 ),
 ( 0.0004766839783820474058, 0.1029713700210894145, 0.2054660560637967814 ),
 ( 0.6796668928939724186, 0.6809932145055455077 ),
 .UNSPECIFIED. ) ;
#27162 = DIRECTION ( 'NONE',  ( 0.000000000000000000, 0.000000000000000000, 1.000000000000000000 ) ) ;
#27163 = ORIENTED_EDGE ( 'NONE', *, *, #77713, .F. ) ;
#27164 = CARTESIAN_POINT ( 'NONE',  ( -14.25192491085926072, -16.12266454619898326, 11.49999999999998934 ) ) ;
#27165 = AXIS2_PLACEMENT_3D ( 'NONE', #95927, #39635, #26423 ) ;
#27166 = CARTESIAN_POINT ( 'NONE',  ( 5.949073730962466833, -5.965225279485572685, -27.94053387008862188 ) ) ;
#27167 = CARTESIAN_POINT ( 'NONE',  ( -71.30457154551153565, -25.25639407517100565, 6.209207384461286061 ) ) ;
#27168 = CARTESIAN_POINT ( 'NONE',  ( -69.52287095715009002, -23.48783264082477018, -1.443836473390092801 ) ) ;
#27169 = DIRECTION ( 'NONE',  ( -0.1311553622875919756, -6.845827386180409975E-16, -0.9913618264504692190 ) ) ;
#27170 = CARTESIAN_POINT ( 'NONE',  ( 3.929728083993185184, -22.62717521373229701, -1.500000000000002220 ) ) ;
#27171 = EDGE_CURVE ( 'NONE', #37175, #66086, #48110, .T. ) ;
#27172 = PERSON_AND_ORGANIZATION_ROLE ( 'classification_officer' ) ;
#27173 = DIRECTION ( 'NONE',  ( -0.000000000000000000, -0.000000000000000000, -1.000000000000000000 ) ) ;
#27174 = CARTESIAN_POINT ( 'NONE',  ( -49.59336093443951654, -24.15543982623906771, -0.2315651400026657036 ) ) ;
#27175 = CARTESIAN_POINT ( 'NONE',  ( 19.99232773509726258, 2.034096180923423702, 11.49999999999999645 ) ) ;
#27176 = DIRECTION ( 'NONE',  ( 0.000000000000000000, 0.000000000000000000, 1.000000000000000000 ) ) ;
#27177 = LINE ( 'NONE', #41915, #76013 ) ;
#27178 = PRODUCT ( 'Spool_Varsay\X2\0131\X0\lan', 'Spool_Varsay\X2\0131\X0\lan', '', ( #85309 ) ) ;
#27179 = PLANE ( 'NONE',  #5265 ) ;
#27180 = CARTESIAN_POINT ( 'NONE',  ( -65.62287095715008434, -24.82558206586145033, 1.605769216559450152 ) ) ;
#27181 = DIRECTION ( 'NONE',  ( -0.000000000000000000, -1.000000000000000000, -0.000000000000000000 ) ) ;
#27182 = CARTESIAN_POINT ( 'NONE',  ( 7.713363164125232707, -18.29545692620113684, -1.500000000000002220 ) ) ;
#27183 = B_SPLINE_CURVE_WITH_KNOTS ( 'NONE', 3,
 ( #39809, #92588, #54058, #70266, #93586, #47434 ),
 .UNSPECIFIED., .F., .F.,
 ( 4, 2, 4 ),
 ( 0.000000000000000000, 0.001380901958385389412, 0.002761803916770778824 ),
 .UNSPECIFIED. ) ;
#27184 = DIRECTION ( 'NONE',  ( 0.000000000000000000, 0.9999999999976377785, 2.173523156925979975E-06 ) ) ;
#27185 = CARTESIAN_POINT ( 'NONE',  ( 8.221391366598689743, 17.94232518691122635, -1.500000000000002220 ) ) ;
#27186 = AXIS2_PLACEMENT_3D ( 'NONE', #87301, #34527, #42653 ) ;
#27187 = CARTESIAN_POINT ( 'NONE',  ( 15.94332860179735256, -4.994534053089958014, -27.96060887785571580 ) ) ;
#27188 = CONTEXT_DEPENDENT_SHAPE_REPRESENTATION ( #20027, #43408 ) ;
#27189 = FACE_OUTER_BOUND ( 'NONE', #16083, .T. ) ;
#27190 = CARTESIAN_POINT ( 'NONE',  ( -5.366453405989236813, 0.000000000000000000, 0.000000000000000000 ) ) ;
#27191 = CARTESIAN_POINT ( 'NONE',  ( -7.658335995763069448, 19.15843701367676388, 11.49999999999999645 ) ) ;
#27192 = EDGE_CURVE ( 'NONE', #94148, #93421, #1933, .T. ) ;
#27193 = VECTOR ( 'NONE', #5755, 1000.000000000000000 ) ;
#27194 = DIRECTION ( 'NONE',  ( -1.000000000000000000, 0.000000000000000000, 0.000000000000000000 ) ) ;
#27195 = ADVANCED_FACE ( 'NONE', ( #96769 ), #56233, .F. ) ;
#27196 = CARTESIAN_POINT ( 'NONE',  ( 22.15051849217804403, -4.756829024181505439, 11.49999999999999645 ) ) ;
#27197 = ORIENTED_EDGE ( 'NONE', *, *, #96739, .F. ) ;
#27198 = CARTESIAN_POINT ( 'NONE',  ( -102.5228709571500758, -24.65952944569305316, 1.056160979905702346 ) ) ;
#27199 = CARTESIAN_POINT ( 'NONE',  ( -56.52287095715007581, -24.34917612406836795, 0.1852690917426530193 ) ) ;
#27200 = VECTOR ( 'NONE', #74080, 1000.000000000000227 ) ;
#27201 = CARTESIAN_POINT ( 'NONE',  ( 10.34999999999999254, -2.091390571243891402E-15, 0.000000000000000000 ) ) ;
#27202 = CARTESIAN_POINT ( 'NONE',  ( -56.52287095715008292, -24.66019654487199375, 8.947790411086122830 ) ) ;
#27203 = ADVANCED_FACE ( 'NONE', ( #80044 ), #3444, .T. ) ;
#27204 = ORIENTED_EDGE ( 'NONE', *, *, #56098, .F. ) ;
#27205 = VERTEX_POINT ( 'NONE', #41492 ) ;
#27206 = DIRECTION ( 'NONE',  ( -0.9496245541219264785, 6.845827386180410961E-16, -0.3133898629642195011 ) ) ;
#27207 = CARTESIAN_POINT ( 'NONE',  ( -22.32109313027335062, -5.015931025267754251, -1.500000000000002220 ) ) ;
#27208 = CARTESIAN_POINT ( 'NONE',  ( 21.97688922017995239, 4.772774720514425972, -18.55878510778117985 ) ) ;
#27209 = CARTESIAN_POINT ( 'NONE',  ( -21.57561264457377348, 0.06291308125064201673, -1.500000000000002220 ) ) ;
#27210 = CARTESIAN_POINT ( 'NONE',  ( -113.5528490827367847, -24.35071581493543746, 9.817618358456018157 ) ) ;
#27211 = DIRECTION ( 'NONE',  ( 0.000000000000000000, 1.000000000000000000, 0.000000000000000000 ) ) ;
#27212 = CARTESIAN_POINT ( 'NONE',  ( -6.671648801611133273, 21.52854475820963032, 11.49999999999999645 ) ) ;
#27213 = ORIENTED_EDGE ( 'NONE', *, *, #34931, .F. ) ;
#27214 = CARTESIAN_POINT ( 'NONE',  ( -43.49940552739553112, -24.15543982623906771, -0.2315651400026568496 ) ) ;
#27215 = CARTESIAN_POINT ( 'NONE',  ( 3.092608977599853315, -21.74436839971096802, 11.49999999999998934 ) ) ;
#27216 = DIRECTION ( 'NONE',  ( -3.773278334444167608E-23, 1.000000000000000000, 0.000000000000000000 ) ) ;
#27217 = CARTESIAN_POINT ( 'NONE',  ( -29.05583327267715532, -25.21724757842646625, 6.516962117439502933 ) ) ;
#27218 = ORIENTED_EDGE ( 'NONE', *, *, #17484, .F. ) ;
#27219 = B_SPLINE_CURVE_WITH_KNOTS ( 'NONE', 3,
 ( #35542, #21285, #88830, #28913, #11196, #50266 ),
 .UNSPECIFIED., .F., .F.,
 ( 4, 2, 4 ),
 ( 6.391158118963033910E-06, 0.001387004593080781809, 0.002767618028042600261 ),
 .UNSPECIFIED. ) ;
#27220 = LINE ( 'NONE', #96718, #68638 ) ;
#27221 = CARTESIAN_POINT ( 'NONE',  ( -0.4909855769230799249, -5.876774720514410077, 19.14743589743590491 ) ) ;
#27222 = ORIENTED_EDGE ( 'NONE', *, *, #92041, .T. ) ;
#27223 = DIRECTION ( 'NONE',  ( 0.000000000000000000, 1.000000000000000000, 0.000000000000000000 ) ) ;
#27224 = CARTESIAN_POINT ( 'NONE',  ( -19.23287947355762384, -7.152392467615741545, -1.500000000000002220 ) ) ;
#27225 = ORIENTED_EDGE ( 'NONE', *, *, #19553, .T. ) ;
#27226 = ORIENTED_EDGE ( 'NONE', *, *, #22851, .F. ) ;
#27227 = ORIENTED_EDGE ( 'NONE', *, *, #75784, .T. ) ;
#27228 = EDGE_CURVE ( 'NONE', #72403, #91284, #65357, .T. ) ;
#27229 = CARTESIAN_POINT ( 'NONE',  ( -60.62287095715004881, -25.00158670708908915, 2.256160236439166855 ) ) ;
#27230 = CARTESIAN_POINT ( 'NONE',  ( -4.621320343559624177, 12.75000000000004974, 0.000000000000000000 ) ) ;
#27231 = CARTESIAN_POINT ( 'NONE',  ( -50.38191529551148307, -25.12049752546737835, 2.832404795212222659 ) ) ;
#27232 = CARTESIAN_POINT ( 'NONE',  ( -14.54385459823299875, 14.27422344363935025, -1.500000000000002220 ) ) ;
#27233 = ORIENTED_EDGE ( 'NONE', *, *, #89908, .F. ) ;
#27234 = VECTOR ( 'NONE', #52593, 1000.000000000000227 ) ;
#27235 = CARTESIAN_POINT ( 'NONE',  ( -1.001577508147789342, -5.876774720514412742, 19.87297243748311004 ) ) ;
#27236 = CARTESIAN_POINT ( 'NONE',  ( -92.52287095715006160, -23.48786465467241769, 11.44779295918254292 ) ) ;
#27237 = DIRECTION ( 'NONE',  ( 3.773278334444166432E-23, -1.000000000000000000, 0.000000000000000000 ) ) ;
#27238 = CARTESIAN_POINT ( 'NONE',  ( -71.43409008949743111, -25.25855267881839339, 7.038380820086293177 ) ) ;
#27239 = VERTEX_POINT ( 'NONE', #19137 ) ;
#27240 = CARTESIAN_POINT ( 'NONE',  ( -76.62287095715007013, -23.47593901973091235, -1.443836447539004642 ) ) ;
#27241 = CARTESIAN_POINT ( 'NONE',  ( -94.58953762381672448, -23.47593901973091235, -1.443836447539002865 ) ) ;
#27242 = VERTEX_POINT ( 'NONE', #95274 ) ;
#27243 = CARTESIAN_POINT ( 'NONE',  ( -15.22196369898608737, 14.14466773073655581, 11.49999999999998934 ) ) ;
#27244 = EDGE_CURVE ( 'NONE', #94756, #94339, #86654, .T. ) ;
#27245 = EDGE_LOOP ( 'NONE', ( #86011, #78841, #80765, #60264 ) ) ;
#27247 = VERTEX_POINT ( 'NONE', #33875 ) ;
#27246 = DIRECTION ( 'NONE',  ( 0.000000000000000000, -2.173523156925980399E-06, 0.9999999999976378895 ) ) ;
#27248 = B_SPLINE_SURFACE_WITH_KNOTS ( 'NONE', 3, 3, ( 
 ( #23313, #55799, #7600, #53790 ),
 ( #39052, #54297, #47679, #39558 ),
 ( #31946, #85225, #7101, #61407 ),
 ( #46172, #78594, #23822, #38554 ),
 ( #46677, #70000, #489, #31440 ),
 ( #47178, #78096, #8610, #62917 ),
 ( #93838, #24325, #55298, #9102 ) ),
 .UNSPECIFIED., .F., .F., .F.,
 ( 4, 3, 4 ),
 ( 4, 4 ),
 ( 0.7945040050992236980, 0.8970133687736494554, 0.9995227324480751019 ),
 ( 0.01949895220031790111, 0.02052067876555380838 ),
 .UNSPECIFIED. ) ;
#27249 = EDGE_CURVE ( 'NONE', #16063, #79151, #61119, .T. ) ;
#27250 = CARTESIAN_POINT ( 'NONE',  ( -41.56944306088920627, -23.48786465467240347, 11.44779295918255002 ) ) ;
#27251 = DIRECTION ( 'NONE',  ( 0.000000000000000000, 1.000000000000000000, 0.000000000000000000 ) ) ;
#27252 = ORIENTED_EDGE ( 'NONE', *, *, #84031, .F. ) ;
#27253 = VERTEX_POINT ( 'NONE', #34874 ) ;
#27254 = CARTESIAN_POINT ( 'NONE',  ( -112.5562042904833930, -23.48783264082478794, -1.443836473390060604 ) ) ;
#27255 = LINE ( 'NONE', #95260, #41627 ) ;
#27256 = LINE ( 'NONE', #97257, #37172 ) ;
#27257 = CARTESIAN_POINT ( 'NONE',  ( -70.90175588921343319, -25.24515073813446264, 5.458926565674500964 ) ) ;
#27259 = ORIENTED_EDGE ( 'NONE', *, *, #26043, .T. ) ;
#27258 = CARTESIAN_POINT ( 'NONE',  ( 21.87352179494074633, -3.179377960941109915, 11.49999999999999645 ) ) ;
#27260 = EDGE_CURVE ( 'NONE', #87003, #93974, #46549, .T. ) ;
#27261 = CARTESIAN_POINT ( 'NONE',  ( -103.6235449539058919, -24.65952944569304606, 1.056160979905703234 ) ) ;
#27262 = CARTESIAN_POINT ( 'NONE',  ( 22.48748499206561746, 2.281147167042596013, -1.500000000000002220 ) ) ;
#27263 = AXIS2_PLACEMENT_3D ( 'NONE', #51013, #12433, #75325 ) ;
#27264 = ADVANCED_FACE ( 'NONE', ( #40992 ), #57235, .T. ) ;
#27266 = ORIENTED_EDGE ( 'NONE', *, *, #93289, .F. ) ;
#27265 = CARTESIAN_POINT ( 'NONE',  ( -115.5510435398882692, -24.83644354573579349, 8.397322867130096569 ) ) ;
#27267 = EDGE_LOOP ( 'NONE', ( #45591, #86405, #6703, #1138 ) ) ;
#27268 = FACE_OUTER_BOUND ( 'NONE', #79473, .T. ) ;
#27269 = VECTOR ( 'NONE', #3042, 1000.000000000000114 ) ;
#27270 = CARTESIAN_POINT ( 'NONE',  ( -57.53372114876139420, -24.66019654487198665, 8.947790411086121054 ) ) ;
#27271 = EDGE_LOOP ( 'NONE', ( #52954, #73238, #82425, #17900, #75639, #27074, #48978, #85519, #33763, #2651, #19104, #76250 ) ) ;
#27272 = CARTESIAN_POINT ( 'NONE',  ( 3.105769797727405024, 20.95935918496786599, -1.500000000000002220 ) ) ;
#27273 = CIRCLE ( 'NONE', #67767, 18.50000000000000000 ) ;
#27274 = CARTESIAN_POINT ( 'NONE',  ( -7.326845193947049140, -6.376774720514417183, 20.33046051580616265 ) ) ;
#27275 = CARTESIAN_POINT ( 'NONE',  ( -41.86233165767207964, -25.29049933140881734, 4.390697414263186715 ) ) ;
#27276 = CARTESIAN_POINT ( 'NONE',  ( 21.63714550250683644, -5.416328558471028565, -1.500000000000002220 ) ) ;
#27277 = DIRECTION ( 'NONE',  ( -0.9888510809027409865, -4.164321980682959710E-15, -0.1489078231574183231 ) ) ;
#27278 = ORIENTED_EDGE ( 'NONE', *, *, #24894, .F. ) ;
#27279 = CARTESIAN_POINT ( 'NONE',  ( -5.063563723219555612, -6.376774720514408301, 19.46509473978807847 ) ) ;
#27280 = DIRECTION ( 'NONE',  ( 0.000000000000000000, -1.000000000000000000, 0.000000000000000000 ) ) ;
#27281 = FACE_OUTER_BOUND ( 'NONE', #36213, .T. ) ;
#27282 = DIRECTION ( 'NONE',  ( 0.000000000000000000, 0.000000000000000000, -1.000000000000000000 ) ) ;
#27283 = EDGE_CURVE ( 'NONE', #17533, #93024, #43496, .T. ) ;
#27284 = CARTESIAN_POINT ( 'NONE',  ( -19.34354882100874562, 2.624169249526263403, 11.49999999999998934 ) ) ;
#27285 = CARTESIAN_POINT ( 'NONE',  ( -13.24026558610970916, 16.85365899302435722, -1.500000000000002220 ) ) ;
#27286 = CARTESIAN_POINT ( 'NONE',  ( -27.70544111104076990, -24.92774666352100965, 1.628749181268301927 ) ) ;
#27287 = CARTESIAN_POINT ( 'NONE',  ( -111.5228709571500616, -29.50250243563736774, 8.947779886222136270 ) ) ;
#27288 = CARTESIAN_POINT ( 'NONE',  ( -77.50833635574721825, -24.15543982623907482, -0.2315651400026658147 ) ) ;
#27289 = CARTESIAN_POINT ( 'NONE',  ( -22.57016884136470125, -3.422276288085174478, -1.500000000000002220 ) ) ;
#27290 = EDGE_CURVE ( 'NONE', #45491, #67032, #51404, .T. ) ;
#27291 = CARTESIAN_POINT ( 'NONE',  ( -102.6311358316829825, -23.96119346886881729, -0.6495511937831878191 ) ) ;
#27292 = LINE ( 'NONE', #34404, #5439 ) ;
#27293 = CARTESIAN_POINT ( 'NONE',  ( -16.79965634883036074, 10.71410036745690597, 11.49999999999999645 ) ) ;
#27294 = CARTESIAN_POINT ( 'NONE',  ( -104.6305873691463404, -23.96119346886880663, -0.6495511937832033622 ) ) ;
#27295 = CARTESIAN_POINT ( 'NONE',  ( -39.53917220841552194, -24.35071581493542681, 9.817618358456035921 ) ) ;
#27296 = CARTESIAN_POINT ( 'NONE',  ( -48.50071888450607105, -24.15543982623907482, -0.2315651400026527418 ) ) ;
#27297 = VERTEX_POINT ( 'NONE', #98755 ) ;
#27298 = LINE ( 'NONE', #57273, #96335 ) ;
#27299 = CARTESIAN_POINT ( 'NONE',  ( -31.23333084502592882, -24.87219037988794312, 1.747789950295619787 ) ) ;
#27300 = CARTESIAN_POINT ( 'NONE',  ( 20.80172415560569021, 6.174449132348904357, 11.49999999999998934 ) ) ;
#27301 = CARTESIAN_POINT ( 'NONE',  ( -56.51485917416104598, -23.73791477778911840, 11.05961554403170766 ) ) ;
#27302 = CARTESIAN_POINT ( 'NONE',  ( 18.95637782189878706, 4.751392969308117387, -1.500000000000002220 ) ) ;
#27303 = CARTESIAN_POINT ( 'NONE',  ( -93.52287095715007581, -23.73907113216989018, -1.053371485793250129 ) ) ;
#27304 = PERSON_AND_ORGANIZATION ( #70597, #27821 ) ;
#27305 = LINE ( 'NONE', #96318, #25650 ) ;
#27306 = CARTESIAN_POINT ( 'NONE',  ( -15.55180764702766716, 13.24544322234432414, 11.49999999999999645 ) ) ;
#27307 = CARTESIAN_POINT ( 'NONE',  ( -49.44071097719352537, -25.28921703305024948, 5.643882662217386326 ) ) ;
#27308 = CARTESIAN_POINT ( 'NONE',  ( -63.62287095715004881, -23.47593901973091235, -1.443836447539007972 ) ) ;
#27309 = EDGE_CURVE ( 'NONE', #50554, #93259, #89161, .T. ) ;
#27310 = ORIENTED_EDGE ( 'NONE', *, *, #33415, .F. ) ;
#27311 = CARTESIAN_POINT ( 'NONE',  ( -123.6228709571500559, -29.50248528299804818, 1.056150453629045360 ) ) ;
#27312 = CARTESIAN_POINT ( 'NONE',  ( -102.6228709571500417, -23.48786465467241769, 11.44779295918253936 ) ) ;
#27313 = CARTESIAN_POINT ( 'NONE',  ( 31.33322533232960083, -4.132774720514427180, -3.827970713771306155 ) ) ;
#27314 = DIRECTION ( 'NONE',  ( -0.000000000000000000, 1.000000000000000000, -0.000000000000000000 ) ) ;
#27315 = VERTEX_POINT ( 'NONE', #74431 ) ;
#27316 = EDGE_CURVE ( 'NONE', #98627, #97595, #44994, .T. ) ;
#27317 = LINE ( 'NONE', #67386, #88482 ) ;
#27318 = ADVANCED_FACE ( 'NONE', ( #29246 ), #5915, .F. ) ;
#27319 = VECTOR ( 'NONE', #14564, 1000.000000000000000 ) ;
#27320 = ADVANCED_FACE ( 'NONE', ( #21130 ), #67834, .T. ) ;
#27321 = CARTESIAN_POINT ( 'NONE',  ( -9.967090755842360039, -20.75144515299163217, 11.49999999999999645 ) ) ;
#27322 = CARTESIAN_POINT ( 'NONE',  ( -13.85039312988123150, 18.09399583546626289, -1.500000000000002220 ) ) ;
#27323 = CARTESIAN_POINT ( 'NONE',  ( 4.115044103975469270, -6.376774720514427841, 21.79213183355573946 ) ) ;
#27324 = CARTESIAN_POINT ( 'NONE',  ( -26.33488822642538452, -29.50249716773871356, 6.524111834107554131 ) ) ;
#27325 = CARTESIAN_POINT ( 'NONE',  ( 1.999999999999998224, 0.000000000000000000, 18.50000000000000000 ) ) ;
#27326 = EDGE_CURVE ( 'NONE', #18521, #55686, #75411, .T. ) ;
#27327 = CARTESIAN_POINT ( 'NONE',  ( -78.52287095715006160, -23.48786465467241769, 11.44779295918254469 ) ) ;
#27328 = CARTESIAN_POINT ( 'NONE',  ( -89.52287095715004739, -24.51283580621451819, 0.6167428607046001598 ) ) ;
#27329 = CARTESIAN_POINT ( 'NONE',  ( -3.281320334969873631, 21.64054093270537393, 11.49999999999998934 ) ) ;
#27330 = FACE_OUTER_BOUND ( 'NONE', #5249, .T. ) ;
#27331 = DIRECTION ( 'NONE',  ( -0.4771587602595988020, -0.8788171126619706008, -0.000000000000000000 ) ) ;
#27332 = DIRECTION ( 'NONE',  ( 1.000000000000000000, 3.773278334444166432E-23, 8.201307841325785021E-29 ) ) ;
#27333 = CARTESIAN_POINT ( 'NONE',  ( 26.74698519091204574, 4.772774720514425972, -10.98683230472873973 ) ) ;
#27334 = ORIENTED_EDGE ( 'NONE', *, *, #69193, .T. ) ;
#27335 = VECTOR ( 'NONE', #17581, 1000.000000000000000 ) ;
#27336 = CARTESIAN_POINT ( 'NONE',  ( -1.067026067711715154, -20.38227831319515460, -1.500000000000002220 ) ) ;
#27337 = VERTEX_POINT ( 'NONE', #83528 ) ;
#27338 = ORIENTED_EDGE ( 'NONE', *, *, #84341, .T. ) ;
#27339 = EDGE_LOOP ( 'NONE', ( #52430, #90503 ) ) ;
#27340 = EDGE_LOOP ( 'NONE', ( #94138, #36568, #72656, #55050 ) ) ;
#27341 = EDGE_CURVE ( 'NONE', #93999, #49156, #87713, .T. ) ;
#27342 = EDGE_CURVE ( 'NONE', #5107, #59954, #12575, .T. ) ;
#27343 = CARTESIAN_POINT ( 'NONE',  ( -11.53412672884717871, -19.92380006517282709, 11.49999999999998934 ) ) ;
#27344 = FACE_OUTER_BOUND ( 'NONE', #96840, .T. ) ;
#27345 = CARTESIAN_POINT ( 'NONE',  ( 14.76687977769557847, -13.71354340032049457, -1.500000000000002220 ) ) ;
#27346 = EDGE_LOOP ( 'NONE', ( #10523, #36151, #47606, #28857 ) ) ;
#27347 = CARTESIAN_POINT ( 'NONE',  ( -97.62287095715007013, -24.34917612406837861, 0.1852690917426668693 ) ) ;
#27348 = FACE_OUTER_BOUND ( 'NONE', #80694, .T. ) ;
#27349 = CARTESIAN_POINT ( 'NONE',  ( -101.5228709571500900, -23.96177878511308634, 10.65340807706329507 ) ) ;
#27350 = CARTESIAN_POINT ( 'NONE',  ( 8.971512145086503409, -1.028487854913504140, -5.500000000000000000 ) ) ;
#27352 = VERTEX_POINT ( 'NONE', #20635 ) ;
#27351 = CARTESIAN_POINT ( 'NONE',  ( 15.73328655151706101, -14.44092690703295467, 11.49999999999999645 ) ) ;
#27353 = DIRECTION ( 'NONE',  ( 0.6837766319725330222, 0.000000000000000000, -0.7296913851542302654 ) ) ;
#27354 = VERTEX_POINT ( 'NONE', #97270 ) ;
#27355 = CARTESIAN_POINT ( 'NONE',  ( 19.22371909900314435, 11.20011194808016342, 11.49999999999998934 ) ) ;
#27356 = CARTESIAN_POINT ( 'NONE',  ( 20.01179378540625819, 5.277757631783551950, 11.49999999999998934 ) ) ;
#27357 = EDGE_CURVE ( 'NONE', #92089, #17028, #5397, .T. ) ;
#27358 = VERTEX_POINT ( 'NONE', #43983 ) ;
#27359 = DIRECTION ( 'NONE',  ( -3.773278334453079030E-23, 0.9999999999976377785, 2.173523156925979128E-06 ) ) ;
#27360 = ORIENTED_EDGE ( 'NONE', *, *, #14388, .F. ) ;
#27361 = DIRECTION ( 'NONE',  ( 0.9888510809027408754, -5.365801633547220192E-16, 0.1489078231574191280 ) ) ;
#27362 = EDGE_LOOP ( 'NONE', ( #96479, #81026, #92102, #10092 ) ) ;
#27363 = CARTESIAN_POINT ( 'NONE',  ( -50.32469610480872291, -25.10935127440189163, 2.834264403437368962 ) ) ;
#27364 = CARTESIAN_POINT ( 'NONE',  ( -18.84683179826791743, -9.195131953753229226, -1.500000000000002220 ) ) ;
#27365 = CARTESIAN_POINT ( 'NONE',  ( 15.10893391618534665, -15.86458014800626692, 11.49999999999999645 ) ) ;
#27366 = B_SPLINE_CURVE_WITH_KNOTS ( 'NONE', 3,
 ( #36436, #14087, #44556, #37443, #75482, #82608 ),
 .UNSPECIFIED., .F., .F.,
 ( 4, 2, 4 ),
 ( 1.570887131794176733E-05, 0.001396322306279757170, 0.002776935741241572803 ),
 .UNSPECIFIED. ) ;
#27367 = EDGE_CURVE ( 'NONE', #36345, #64249, #19105, .T. ) ;
#27368 = CARTESIAN_POINT ( 'NONE',  ( -26.56775203954515874, -24.89279871775309516, 6.997625193822926803 ) ) ;
#27369 = CARTESIAN_POINT ( 'NONE',  ( -17.96456891314058879, -13.58578184957126034, -1.500000000000002220 ) ) ;
#27370 = CARTESIAN_POINT ( 'NONE',  ( 10.03794737889396771, 18.37758748099471973, -1.500000000000002220 ) ) ;
#27371 = ADVANCED_FACE ( 'NONE', ( #61717 ), #15512, .T. ) ;
#27372 = CARTESIAN_POINT ( 'NONE',  ( -110.5228709571500474, -24.82558206586148231, 1.605769216559631563 ) ) ;
#27373 = CARTESIAN_POINT ( 'NONE',  ( 6.404294203292168142, -5.876774720514415407, 20.09052689972686423 ) ) ;
#27374 = B_SPLINE_CURVE_WITH_KNOTS ( 'NONE', 3,
 ( #2968, #97300, #95796, #57266 ),
 .UNSPECIFIED., .F., .F.,
 ( 4, 4 ),
 ( 2.775557561562891043E-17, 9.999999999998898659E-05 ),
 .UNSPECIFIED. ) ;
#27375 = CARTESIAN_POINT ( 'NONE',  ( -119.6235012026005080, -24.66019654487200441, 8.947790411086108620 ) ) ;
#27376 = FACE_OUTER_BOUND ( 'NONE', #79373, .T. ) ;
#27377 = ORIENTED_EDGE ( 'NONE', *, *, #91809, .F. ) ;
#27378 = EDGE_CURVE ( 'NONE', #35739, #45794, #71897, .T. ) ;
#27379 = VERTEX_POINT ( 'NONE', #30241 ) ;
#27380 = EDGE_LOOP ( 'NONE', ( #63194, #99552, #83488, #83244 ) ) ;
#27381 = LINE ( 'NONE', #25877, #69307 ) ;
#27382 = VERTEX_POINT ( 'NONE', #92141 ) ;
#27383 = CARTESIAN_POINT ( 'NONE',  ( -8.943896628894790979, 19.53434260886740503, -1.500000000000002220 ) ) ;
#27384 = EDGE_CURVE ( 'NONE', #12369, #41069, #77972, .T. ) ;
#27385 = CARTESIAN_POINT ( 'NONE',  ( 0.3085469314987323020, -6.376774720514413630, 19.52341893546493523 ) ) ;
#27386 = ORIENTED_EDGE ( 'NONE', *, *, #18442, .F. ) ;
#27387 = CARTESIAN_POINT ( 'NONE',  ( 20.77832821955112408, -3.674247523096572099, 11.49999999999998934 ) ) ;
#27388 = LINE ( 'NONE', #4053, #12558 ) ;
#27389 = DIRECTION ( 'NONE',  ( 0.000000000000000000, 0.000000000000000000, 1.000000000000000000 ) ) ;
#27391 = CARTESIAN_POINT ( 'NONE',  ( 29.80070917940689412, 5.965225279485572685, 27.39560796525321607 ) ) ;
#27390 = VECTOR ( 'NONE', #3764, 1000.000000000000114 ) ;
#27392 = CARTESIAN_POINT ( 'NONE',  ( -80.35919894935767616, -25.29534345321060940, 4.505481338261425606 ) ) ;
#27393 = CARTESIAN_POINT ( 'NONE',  ( 0.000000000000000000, -1.477225279485574028, -1.352392034746782823 ) ) ;
#27394 = CARTESIAN_POINT ( 'NONE',  ( -21.88945651911318535, 3.243594245096953710, -1.500000000000002220 ) ) ;
#27395 = VERTEX_POINT ( 'NONE', #45492 ) ;
#27396 = CARTESIAN_POINT ( 'NONE',  ( -81.50565816229075722, -24.35071581493543036, 9.817618358456037697 ) ) ;
#27397 = CARTESIAN_POINT ( 'NONE',  ( -111.6228709571500559, -29.50250786944525672, 11.44777988621622988 ) ) ;
#27398 = CARTESIAN_POINT ( 'NONE',  ( -40.89894032811586300, -25.27956060308583730, 5.492539715312949156 ) ) ;
#27399 = VECTOR ( 'NONE', #78877, 1000.000000000000000 ) ;
#27400 = CARTESIAN_POINT ( 'NONE',  ( -62.54857352048542651, -24.15620529776627734, 10.23563542870660825 ) ) ;
#27402 = DIRECTION ( 'NONE',  ( 1.000000000000000000, 0.000000000000000000, 0.000000000000000000 ) ) ;
#27401 = AXIS2_PLACEMENT_3D ( 'NONE', #66399, #4972, #21184 ) ;
#27403 = CARTESIAN_POINT ( 'NONE',  ( -15.06583839362908961, -15.15408912208086534, -1.500000000000002220 ) ) ;
#27404 = CARTESIAN_POINT ( 'NONE',  ( -69.00578779554861342, -25.20549243710579290, 6.637794156083747232 ) ) ;
#27405 = CARTESIAN_POINT ( 'NONE',  ( -50.91839352580279865, -25.25978491487771649, 3.590542621692356384 ) ) ;
#27406 = CARTESIAN_POINT ( 'NONE',  ( -64.50990493018097993, -23.96169478059713498, 10.65365249895718058 ) ) ;
#27407 = CARTESIAN_POINT ( 'NONE',  ( 32.84232313084847732, -4.840274619473232676, -11.71291885348859196 ) ) ;
#27408 = CARTESIAN_POINT ( 'NONE',  ( 22.38532167473930556, -2.757513164441831144, -1.500000000000002220 ) ) ;
#27410 = CARTESIAN_POINT ( 'NONE',  ( 3.176458874063931681, -0.3587747205143967943, -28.85257003503889806 ) ) ;
#27409 = B_SPLINE_CURVE_WITH_KNOTS ( 'NONE', 3,
 ( #23136, #62743, #69838, #93657, #8930, #78932 ),
 .UNSPECIFIED., .F., .F.,
 ( 4, 2, 4 ),
 ( 6.391158118958420121E-06, 0.001387004593080778557, 0.002767618028042598960 ),
 .UNSPECIFIED. ) ;
#27411 = ORIENTED_EDGE ( 'NONE', *, *, #25017, .T. ) ;
#27412 = PLANE ( 'NONE',  #27186 ) ;
#27413 = CARTESIAN_POINT ( 'NONE',  ( -79.50500068773956741, -24.34968618360933945, 0.1864209137778814473 ) ) ;
#27414 = CARTESIAN_POINT ( 'NONE',  ( 19.48663422773152121, -3.193742178437300794, 11.49999999999999645 ) ) ;
#27415 = LINE ( 'NONE', #34530, #63407 ) ;
#27416 = AXIS2_PLACEMENT_3D ( 'NONE', #61791, #36935, #67906 ) ;
#27417 = B_SPLINE_CURVE_WITH_KNOTS ( 'NONE', 3,
 ( #77744, #8259, #78749, #79259 ),
 .UNSPECIFIED., .F., .F.,
 ( 4, 4 ),
 ( 0.6309505463409755821, 0.6399569776130914489 ),
 .UNSPECIFIED. ) ;
#27418 = B_SPLINE_CURVE_WITH_KNOTS ( 'NONE', 3,
 ( #82235, #4126, #75120, #12715 ),
 .UNSPECIFIED., .F., .F.,
 ( 4, 4 ),
 ( 0.000000000000000000, 9.999999999998897304E-05 ),
 .UNSPECIFIED. ) ;
#27419 = CARTESIAN_POINT ( 'NONE',  ( -32.07722060962684907, -25.33442522607536418, 4.656390931545514533 ) ) ;
#27420 = VERTEX_POINT ( 'NONE', #86033 ) ;
#27421 = CARTESIAN_POINT ( 'NONE',  ( 0.6000000000000007550, 0.000000000000000000, 0.000000000000000000 ) ) ;
#27422 = CARTESIAN_POINT ( 'NONE',  ( -29.02540380353726590, -25.26026405050802026, 2.175342404154256837 ) ) ;
#27423 = DIRECTION ( 'NONE',  ( 1.000000000000000000, 0.000000000000000000, 0.000000000000000000 ) ) ;
#27424 = CARTESIAN_POINT ( 'NONE',  ( 11.61936018155104833, -18.21891831228114356, 11.49999999999998934 ) ) ;
#27425 = DIRECTION ( 'NONE',  ( -1.000000000000000000, -3.773278334444166432E-23, -8.201307841325785021E-29 ) ) ;
#27426 = CARTESIAN_POINT ( 'NONE',  ( -22.05275734969026047, 5.965225279485572685, 31.02402280011862246 ) ) ;
#27427 = DIRECTION ( 'NONE',  ( 1.000000000000000000, 3.639962309748244178E-15, 0.000000000000000000 ) ) ;
#27428 = FACE_OUTER_BOUND ( 'NONE', #42250, .T. ) ;
#27429 = CARTESIAN_POINT ( 'NONE',  ( 17.16143643543069075, 9.858047367376444825, -1.500000000000002220 ) ) ;
#27430 = ORIENTED_EDGE ( 'NONE', *, *, #66774, .T. ) ;
#27431 = CARTESIAN_POINT ( 'NONE',  ( 5.347689060783223702, 19.56899250667117229, 11.49999999999999645 ) ) ;
#27432 = CARTESIAN_POINT ( 'NONE',  ( -54.62287095715005592, -24.66019654487199020, 8.947790411086135265 ) ) ;
#27433 = AXIS2_PLACEMENT_3D ( 'NONE', #82448, #91555, #36782 ) ;
#27434 = CARTESIAN_POINT ( 'NONE',  ( 6.403846153846157740, -5.876774720514425177, 21.48076923076922995 ) ) ;
#27435 = ADVANCED_FACE ( 'NONE', ( #16014 ), #77405, .T. ) ;
#27436 = ORIENTED_EDGE ( 'NONE', *, *, #97720, .F. ) ;
#27437 = B_SPLINE_SURFACE_WITH_KNOTS ( 'NONE', 3, 3, ( 
 ( #90844, #21315, #89845, #96459 ),
 ( #4118, #5606, #52286, #81734 ),
 ( #11224, #58417, #42202, #5106 ),
 ( #50299, #4620, #73133, #65541 ) ),
 .UNSPECIFIED., .F., .F., .F.,
 ( 4, 4 ),
 ( 4, 4 ),
 ( 0.5133787333263793995, 0.6547335371774368751 ),
 ( 0.7903368604290639254, 0.8131061223386927272 ),
 .UNSPECIFIED. ) ;
#27438 = CARTESIAN_POINT ( 'NONE',  ( -99.52925925567853938, -25.26679311647689730, 4.031539577752753623 ) ) ;
#27439 = CARTESIAN_POINT ( 'NONE',  ( 31.62087157062645204, 4.386438359062696080, 26.73777224682022435 ) ) ;
#27440 = CARTESIAN_POINT ( 'NONE',  ( -71.52287095715010423, -24.66019654487200086, 8.947790411086115725 ) ) ;
#27441 = EDGE_CURVE ( 'NONE', #10045, #80664, #85026, .T. ) ;
#27442 = CARTESIAN_POINT ( 'NONE',  ( -52.52287095715006870, -24.64898659630367916, 1.056161002820821038 ) ) ;
#27443 = ADVANCED_FACE ( 'NONE', ( #39362 ), #22616, .T. ) ;
#27444 = CARTESIAN_POINT ( 'NONE',  ( -24.90875734969025501, 5.965225279485572685, 30.00402280011862288 ) ) ;
#27445 = CARTESIAN_POINT ( 'NONE',  ( 4.692034869050136336, 19.47840706813412126, -1.500000000000002220 ) ) ;
#27446 = EDGE_CURVE ( 'NONE', #67691, #54301, #77903, .T. ) ;
#27447 = DIRECTION ( 'NONE',  ( 0.000000000000000000, 0.000000000000000000, -1.000000000000000000 ) ) ;
#27448 = ORIENTED_EDGE ( 'NONE', *, *, #8647, .F. ) ;
#27449 = EDGE_CURVE ( 'NONE', #71622, #97633, #78414, .T. ) ;
#27450 = EDGE_CURVE ( 'NONE', #54238, #23749, #8911, .T. ) ;
#27451 = LINE ( 'NONE', #35060, #50220 ) ;
#27452 = DIRECTION ( 'NONE',  ( -0.8264557562326033668, -6.845827386180409975E-16, -0.5630016722799281448 ) ) ;
#27453 = DIRECTION ( 'NONE',  ( -0.000000000000000000, 1.000000000000000000, -0.000000000000000000 ) ) ;
#27454 = B_SPLINE_CURVE_WITH_KNOTS ( 'NONE', 3,
 ( #68646, #69133, #38679, #100055, #84855, #7225 ),
 .UNSPECIFIED., .F., .F.,
 ( 4, 2, 4 ),
 ( 0.000000000000000000, 0.001380764517854768869, 0.002761529035709537738 ),
 .UNSPECIFIED. ) ;
#27455 = FACE_OUTER_BOUND ( 'NONE', #75150, .T. ) ;
#27456 = CARTESIAN_POINT ( 'NONE',  ( 14.83405752585473891, 4.881907540128495704, -27.54622755360321307 ) ) ;
#27457 = FACE_OUTER_BOUND ( 'NONE', #56827, .T. ) ;
#27458 = ORIENTED_EDGE ( 'NONE', *, *, #38257, .F. ) ;
#27459 = AXIS2_PLACEMENT_3D ( 'NONE', #5545, #75545, #82174 ) ;
#27460 = CARTESIAN_POINT ( 'NONE',  ( -20.32193514540556123, 0.06534614623005505218, 11.49999999999998934 ) ) ;
#27461 = VERTEX_POINT ( 'NONE', #84035 ) ;
#27462 = EDGE_CURVE ( 'NONE', #76784, #54393, #61064, .T. ) ;
#27463 = CARTESIAN_POINT ( 'NONE',  ( 0.5590224530292132732, -22.91010021869659852, -1.500000000000002220 ) ) ;
#27464 = CARTESIAN_POINT ( 'NONE',  ( -32.56126115692759981, -23.73766607897670866, -1.055555164236441801 ) ) ;
#27465 = EDGE_LOOP ( 'NONE', ( #18863, #46943, #43932, #47062, #24929 ) ) ;
#27466 = CIRCLE ( 'NONE', #19337, 1.529999999999998916 ) ;
#27467 = CARTESIAN_POINT ( 'NONE',  ( -37.62287095715005592, -23.72747288104441665, -1.053458166803663110 ) ) ;
#27468 = CARTESIAN_POINT ( 'NONE',  ( -50.36234373730416536, -25.26264178341608968, 7.100826787533305762 ) ) ;
#27469 = EDGE_CURVE ( 'NONE', #32299, #4321, #57821, .T. ) ;
#27470 = AXIS2_PLACEMENT_3D ( 'NONE', #3750, #89473, #19948 ) ;
#27471 = LINE ( 'NONE', #43685, #22106 ) ;
#27472 = CARTESIAN_POINT ( 'NONE',  ( -20.81765089029956783, 3.879123387127271005, 11.49999999999999645 ) ) ;
#27473 = CARTESIAN_POINT ( 'NONE',  ( -12.03526013704878039, -18.61824004984164560, -1.500000000000002220 ) ) ;
#27474 = CARTESIAN_POINT ( 'NONE',  ( 19.36870410414886479, 7.000668502413378569, 11.49999999999998934 ) ) ;
#27476 = ORIENTED_EDGE ( 'NONE', *, *, #76444, .T. ) ;
#27475 = VECTOR ( 'NONE', #75165, 1000.000000000000000 ) ;
#27477 = CARTESIAN_POINT ( 'NONE',  ( -41.62876366737128819, -24.51314013834315375, 0.6176544820404115121 ) ) ;
#27478 = EDGE_LOOP ( 'NONE', ( #20746, #75875, #31457, #31770 ) ) ;
#27479 = CARTESIAN_POINT ( 'NONE',  ( 6.627987042499408510, -6.376774720514424288, 21.45334999081212146 ) ) ;
#27480 = CARTESIAN_POINT ( 'NONE',  ( -49.62287095715005592, -24.64898659630528499, 1.056161002820821038 ) ) ;
#27481 = ORIENTED_EDGE ( 'NONE', *, *, #2145, .T. ) ;
#27482 = ORIENTED_EDGE ( 'NONE', *, *, #98325, .F. ) ;
#27483 = ORIENTED_EDGE ( 'NONE', *, *, #91269, .T. ) ;
#27484 = CARTESIAN_POINT ( 'NONE',  ( -77.52287095715006160, -24.66019654487200086, 8.947790411086113949 ) ) ;
#27485 = CARTESIAN_POINT ( 'NONE',  ( -71.62287095715005592, -24.64965695001468404, 8.947790433994184056 ) ) ;
#27486 = CARTESIAN_POINT ( 'NONE',  ( -102.5228709571500758, -24.64965694238407323, 8.947790433994194714 ) ) ;
#27487 = CARTESIAN_POINT ( 'NONE',  ( 5.171613189315443115, 20.13430294385436881, -1.500000000000002220 ) ) ;
#27488 = CARTESIAN_POINT ( 'NONE',  ( 16.47784684176308545, -14.13017478139203220, 11.49999999999999645 ) ) ;
#27489 = ORIENTED_EDGE ( 'NONE', *, *, #27469, .T. ) ;
#27490 = CARTESIAN_POINT ( 'NONE',  ( -8.160000000000000142, -9.652339641703484574, -1.621096496867199033 ) ) ;
#27491 = CARTESIAN_POINT ( 'NONE',  ( -96.52287095715006160, -24.65952944569304606, 1.056160979905702346 ) ) ;
#27492 = CARTESIAN_POINT ( 'NONE',  ( 6.649717926671450563, 21.43536518531312396, 11.49999999999998934 ) ) ;
#27493 = EDGE_CURVE ( 'NONE', #8750, #56847, #59466, .T. ) ;
#27494 = LINE ( 'NONE', #34107, #17367 ) ;
#27495 = CARTESIAN_POINT ( 'NONE',  ( -65.61529522140628501, -23.48783264082477018, -1.443836473390096353 ) ) ;
#27496 = ORIENTED_EDGE ( 'NONE', *, *, #8071, .F. ) ;
#27497 = CARTESIAN_POINT ( 'NONE',  ( -83.62287095715005592, -24.64965695001468404, 8.947790433994182280 ) ) ;
#27498 = CARTESIAN_POINT ( 'NONE',  ( -119.4728709571500502, -25.40674640480649416, 5.000950437805936843 ) ) ;
#27499 = B_SPLINE_CURVE_WITH_KNOTS ( 'NONE', 3,
 ( #81254, #11736, #27969, #97959 ),
 .UNSPECIFIED., .F., .F.,
 ( 4, 4 ),
 ( 0.000000000000000000, 1.000000000000000000 ),
 .UNSPECIFIED. ) ;
#27500 = ORIENTED_EDGE ( 'NONE', *, *, #71911, .F. ) ;
#27501 = ORIENTED_EDGE ( 'NONE', *, *, #43043, .T. ) ;
#27502 = EDGE_CURVE ( 'NONE', #37803, #19978, #44025, .T. ) ;
#27503 = CARTESIAN_POINT ( 'NONE',  ( -69.62287095715004170, -23.96177878511307568, 10.65340807706330395 ) ) ;
#27504 = ORIENTED_EDGE ( 'NONE', *, *, #23937, .F. ) ;
#27505 = B_SPLINE_CURVE_WITH_KNOTS ( 'NONE', 3,
 ( #18695, #96332, #43054, #10096, #65912, #27323, #33433, #89223, #3497, #25321, #64418, #34438, #33938, #42065, #64917, #12081, #10594, #56795, #73496, #95335, #56297, #58284, #25823, #88729, #95830, #19198, #26325 ),
 .UNSPECIFIED., .F., .F.,
 ( 4, 1, 1, 1, 1, 1, 1, 1, 1, 1, 1, 1, 1, 1, 1, 1, 1, 1, 1, 1, 1, 1, 1, 1, 4 ),
 ( 0.000000000000000000, 0.03378714634699089836, 0.06662165772429383404, 0.09928487809597265346, 0.1313611650426506072, 0.1635851875953436008, 0.1961039269870681889, 0.2289022543238170004, 0.2621580559050075143, 0.2959912222583161445, 0.3302178457247997301, 0.3650598258919544037, 0.4009507373401082209, 0.4376203820767376462, 0.4757075294370921026, 0.5153806916250490699, 0.5564135414931649093, 0.5997648298727309424, 0.6464241555840876119, 0.6964314445175666668, 0.7497815178015586612, 0.8065733069755320894, 0.8674355315653994314, 0.9318867532508745555, 1.000000000000000000 ),
 .UNSPECIFIED. ) ;
#27506 = CARTESIAN_POINT ( 'NONE',  ( -12.43717309395686499, -17.31322327496724611, -1.500000000000002220 ) ) ;
#27507 = ORIENTED_EDGE ( 'NONE', *, *, #26580, .T. ) ;
#27508 = CARTESIAN_POINT ( 'NONE',  ( 6.660000000000001030, -10.15233964170348457, -1.303165529866009420 ) ) ;
#27509 = CARTESIAN_POINT ( 'NONE',  ( -6.661741538832703036, 20.79550341630197607, -1.500000000000002220 ) ) ;
#27510 = DIRECTION ( 'NONE',  ( 0.000000000000000000, 0.000000000000000000, 1.000000000000000000 ) ) ;
#27511 = CARTESIAN_POINT ( 'NONE',  ( 7.379361219544559702, 21.46082085352547963, 11.49999999999998934 ) ) ;
#27512 = CARTESIAN_POINT ( 'NONE',  ( -41.39385049892748469, -25.28892541658160553, 3.844044583132800064 ) ) ;
#27513 = DIRECTION ( 'NONE',  ( -1.000000000000000000, -3.773278334444167608E-23, -8.201307833595939069E-29 ) ) ;
#27514 = CARTESIAN_POINT ( 'NONE',  ( -4.809782828112996178, 21.40371668077904488, -1.500000000000002220 ) ) ;
#27515 = CARTESIAN_POINT ( 'NONE',  ( -68.52287095715006160, -29.50248528299804818, 1.056150453629036701 ) ) ;
#27516 = ORIENTED_EDGE ( 'NONE', *, *, #52740, .F. ) ;
#27517 = CARTESIAN_POINT ( 'NONE',  ( -122.5889729151568162, -24.51419770103158413, 9.386484678747169852 ) ) ;
#27518 = CARTESIAN_POINT ( 'NONE',  ( -115.6228709571500701, -25.00158670708909625, 2.256160236439165967 ) ) ;
#27519 = ORIENTED_EDGE ( 'NONE', *, *, #86430, .F. ) ;
#27520 = DIRECTION ( 'NONE',  ( 0.000000000000000000, -1.000000000000000000, 0.000000000000000000 ) ) ;
#27521 = ORIENTED_EDGE ( 'NONE', *, *, #25976, .T. ) ;
#27522 = CARTESIAN_POINT ( 'NONE',  ( -88.52287095715009002, -24.66019654487200441, 8.947790411086119278 ) ) ;
#27523 = CARTESIAN_POINT ( 'NONE',  ( -10.25207789694340299, -22.90580643265542093, 0.5637492489085903502 ) ) ;
#27524 = CARTESIAN_POINT ( 'NONE',  ( -21.26230640008892792, -0.7210608269398429693, 11.49999999999998934 ) ) ;
#27525 = CARTESIAN_POINT ( 'NONE',  ( -55.62287095715006302, -24.63345952396254646, 9.038047939301511846 ) ) ;
#27526 = CARTESIAN_POINT ( 'NONE',  ( -107.6228709571500701, -23.47596703998600631, 11.44779298504227860 ) ) ;
#27527 = AXIS2_PLACEMENT_3D ( 'NONE', #80063, #41508, #72463 ) ;
#27528 = CARTESIAN_POINT ( 'NONE',  ( -85.54116237476874574, -24.83618233451451118, 1.606449574219533272 ) ) ;
#27529 = CARTESIAN_POINT ( 'NONE',  ( -68.51066526543451118, -23.96119346886880663, -0.6495511937832112448 ) ) ;
#27530 = CARTESIAN_POINT ( 'NONE',  ( -39.62287095715006302, -23.73934037231756378, 11.05740245334329863 ) ) ;
#27531 = VERTEX_POINT ( 'NONE', #92639 ) ;
#27532 = CARTESIAN_POINT ( 'NONE',  ( 19.54226456527178257, 0.3027743077981833730, 11.49999999999999645 ) ) ;
#27533 = CARTESIAN_POINT ( 'NONE',  ( -43.22287095715006444, -23.47593901973090169, -1.443836447538997980 ) ) ;
#27534 = CIRCLE ( 'NONE', #40499, 6.594667762285751245 ) ;
#27535 = DIRECTION ( 'NONE',  ( 0.000000000000000000, 1.000000000000000000, -1.084202172485504434E-16 ) ) ;
#27536 = B_SPLINE_CURVE_WITH_KNOTS ( 'NONE', 3,
 ( #44520, #35902, #52627, #66871, #43527, #45525, #83564, #14047 ),
 .UNSPECIFIED., .F., .F.,
 ( 4, 2, 2, 4 ),
 ( 0.000000000000000000, 0.0004967474533590028650, 0.0007451211800385037012, 0.0009934949067180044290 ),
 .UNSPECIFIED. ) ;
#27537 = VERTEX_POINT ( 'NONE', #6909 ) ;
#27538 = CARTESIAN_POINT ( 'NONE',  ( -117.5228709571500758, -23.72773821059536914, 11.05748984161097326 ) ) ;
#27539 = CARTESIAN_POINT ( 'NONE',  ( -99.22760414877923552, -25.31352189248182682, 5.229817175528475026 ) ) ;
#27540 = VECTOR ( 'NONE', #91259, 1000.000000000000000 ) ;
#27541 = LINE ( 'NONE', #6184, #71495 ) ;
#27542 = CARTESIAN_POINT ( 'NONE',  ( -29.49875734969025842, -5.965225279485572685, 15.62202280011862321 ) ) ;
#27543 = CARTESIAN_POINT ( 'NONE',  ( 19.18734209777730015, 4.435579877058994036, -1.500000000000002220 ) ) ;
#27544 = AXIS2_PLACEMENT_3D ( 'NONE', #27598, #19967, #67169 ) ;
#27545 = ORIENTED_EDGE ( 'NONE', *, *, #46132, .F. ) ;
#27546 = AXIS2_PLACEMENT_3D ( 'NONE', #57550, #95593, #19458 ) ;
#27547 = CARTESIAN_POINT ( 'NONE',  ( 33.23241444531825550, -3.542570809989110447, -12.77295888271925328 ) ) ;
#27548 = DIRECTION ( 'NONE',  ( -1.000000000000000000, -3.491481338843133355E-15, -2.352173255807796056E-16 ) ) ;
#27549 = AXIS2_PLACEMENT_3D ( 'NONE', #55237, #47615, #48116 ) ;
#27550 = EDGE_CURVE ( 'NONE', #5356, #3446, #13818, .T. ) ;
#27551 = COORDINATED_UNIVERSAL_TIME_OFFSET ( 0, 0, .AHEAD. ) ;
#27552 = EDGE_LOOP ( 'NONE', ( #30075, #21226, #32384, #2733 ) ) ;
#27553 = CARTESIAN_POINT ( 'NONE',  ( 9.010057473089009505, -0.9200333157601816580, 3.712238059855193839 ) ) ;
#27554 = DIRECTION ( 'NONE',  ( -3.773278334444167608E-23, 1.000000000000000000, 0.000000000000000000 ) ) ;
#27555 = CARTESIAN_POINT ( 'NONE',  ( -55.52200631800427999, -23.48783264082475952, -1.443836473390099462 ) ) ;
#27556 = CARTESIAN_POINT ( 'NONE',  ( -118.5885976234968808, -24.51314013834317151, 0.6176544820404233915 ) ) ;
#27557 = CARTESIAN_POINT ( 'NONE',  ( -28.98875734969026041, -6.376774720514426953, 26.43402280011862615 ) ) ;
#27558 = EDGE_CURVE ( 'NONE', #59306, #36357, #27144, .T. ) ;
#27559 = PLANE ( 'NONE',  #40833 ) ;
#27560 = DIRECTION ( 'NONE',  ( 2.338552693767719605E-15, 0.000000000000000000, 1.000000000000000000 ) ) ;
#27561 = CARTESIAN_POINT ( 'NONE',  ( -12.66726347749767179, -15.43046242340049545, -1.500000000000002220 ) ) ;
#27562 = EDGE_CURVE ( 'NONE', #15222, #23558, #46497, .T. ) ;
#27563 = CARTESIAN_POINT ( 'NONE',  ( -0.04267401778350129321, -22.49755130481472420, 8.628546368132811395 ) ) ;
#27564 = CARTESIAN_POINT ( 'NONE',  ( -8.676013072486071565, -17.92234406281952275, -1.500000000000002220 ) ) ;
#27565 = ORIENTED_EDGE ( 'NONE', *, *, #82644, .T. ) ;
#27566 = CARTESIAN_POINT ( 'NONE',  ( -63.52287095715004739, -23.94994826722563985, -0.6494450866342731388 ) ) ;
#27567 = CARTESIAN_POINT ( 'NONE',  ( 3.825768195983636044, -6.376774720514424288, 21.47884071039599618 ) ) ;
#27568 = EDGE_CURVE ( 'NONE', #42765, #54649, #68297, .T. ) ;
#27569 = ADVANCED_FACE ( 'NONE', ( #87034 ), #24625, .T. ) ;
#27570 = CARTESIAN_POINT ( 'NONE',  ( 10.16119454606818984, -3.316774720514931829, -28.04611093432389524 ) ) ;
#27571 = CARTESIAN_POINT ( 'NONE',  ( -49.62287095715005592, -24.66019654487199020, 8.947790411086135265 ) ) ;
#27572 = CARTESIAN_POINT ( 'NONE',  ( -7.536766146225033047, -5.876774720514411854, 19.63296556618507438 ) ) ;
#27573 = EDGE_CURVE ( 'NONE', #52686, #51486, #47984, .T. ) ;
#27574 = CARTESIAN_POINT ( 'NONE',  ( -10.34999999999999254, 0.9999999999999997780, 1.084202172485504187E-16 ) ) ;
#27575 = ORIENTED_EDGE ( 'NONE', *, *, #993, .F. ) ;
#27576 = CARTESIAN_POINT ( 'NONE',  ( 30.53060340732036337, -5.266063118920828678, 0.9746665865322270417 ) ) ;
#27577 = PLANE ( 'NONE',  #1546 ) ;
#27578 = EDGE_LOOP ( 'NONE', ( #98089, #8917, #48221, #2647 ) ) ;
#27579 = CARTESIAN_POINT ( 'NONE',  ( -13.58233929615340152, 14.99024694321910900, 11.49999999999998934 ) ) ;
#27580 = CARTESIAN_POINT ( 'NONE',  ( -23.59123376470063960, 6.143225279485574397, 23.50402280011862288 ) ) ;
#27581 = CARTESIAN_POINT ( 'NONE',  ( 13.74975846015576586, 5.965225279485572685, -27.72022515045486557 ) ) ;
#27582 = DIRECTION ( 'NONE',  ( 0.000000000000000000, 0.000000000000000000, 1.000000000000000000 ) ) ;
#27583 = B_SPLINE_CURVE_WITH_KNOTS ( 'NONE', 3,
 ( #72234, #18436, #81835, #81338, #10324, #50397, #27055, #11820 ),
 .UNSPECIFIED., .F., .F.,
 ( 4, 2, 2, 4 ),
 ( 0.000000000000000000, 0.002001098010032686687, 0.003001647015049031548, 0.004002196020065376843 ),
 .UNSPECIFIED. ) ;
#27584 = ORIENTED_EDGE ( 'NONE', *, *, #9007, .T. ) ;
#27585 = CARTESIAN_POINT ( 'NONE',  ( -80.15869489321136143, -25.31558262175477481, 4.989020118345524502 ) ) ;
#27586 = CARTESIAN_POINT ( 'NONE',  ( -1.733151984336291695, -5.876774720514407413, 19.29154511076646017 ) ) ;
#27587 = CARTESIAN_POINT ( 'NONE',  ( 4.397486433803790007, -19.56896378179033036, -1.500000000000002220 ) ) ;
#27588 = CARTESIAN_POINT ( 'NONE',  ( -11.62490142266122639, -17.50836435561060256, 11.49999999999999645 ) ) ;
#27589 = DIRECTION ( 'NONE',  ( 0.000000000000000000, 0.000000000000000000, 1.000000000000000000 ) ) ;
#27590 = CARTESIAN_POINT ( 'NONE',  ( -70.54092792707334070, -24.63419186844611986, 9.035850630976923981 ) ) ;
#27591 = CARTESIAN_POINT ( 'NONE',  ( 18.88560736741940005, 11.47387103136259690, -1.500000000000002220 ) ) ;
#27592 = AXIS2_PLACEMENT_3D ( 'NONE', #29217, #97234, #43946 ) ;
#27593 = CARTESIAN_POINT ( 'NONE',  ( -39.48225211724125927, -25.31589192678097433, 4.451013730343944985 ) ) ;
#27594 = CARTESIAN_POINT ( 'NONE',  ( -9.150000000000000355, -5.876774720514426953, -15.69999999999999929 ) ) ;
#27595 = PLANE ( 'NONE',  #76797 ) ;
#27596 = ORIENTED_EDGE ( 'NONE', *, *, #47543, .T. ) ;
#27597 = CARTESIAN_POINT ( 'NONE',  ( -72.51141342689224700, -23.96119346886880663, -0.6495511937832121330 ) ) ;
#27598 = CARTESIAN_POINT ( 'NONE',  ( 31.79364159983995464, 1.682774720514426114, -11.59305536555894278 ) ) ;
#27599 = ORIENTED_EDGE ( 'NONE', *, *, #10825, .T. ) ;
#27600 = B_SPLINE_CURVE_WITH_KNOTS ( 'NONE', 3,
 ( #57891, #41155, #72108, #26426 ),
 .UNSPECIFIED., .F., .F.,
 ( 4, 4 ),
 ( 0.000000000000000000, 1.000000000000000000 ),
 .UNSPECIFIED. ) ;
#27601 = B_SPLINE_CURVE_WITH_KNOTS ( 'NONE', 3,
 ( #52709, #22728, #14128, #98867, #28362, #99854, #29360, #6529, #53718, #30359, #45599, #59323, #45105, #68430, #76519, #90268, #98365, #37480, #76026 ),
 .UNSPECIFIED., .F., .F.,
 ( 4, 1, 1, 1, 1, 1, 1, 1, 1, 1, 1, 1, 1, 1, 1, 1, 4 ),
 ( 0.000000000000000000, 0.06796237149445635839, 0.1332834028675231042, 0.1978352977570558280, 0.2608919865309880515, 0.3233765044831760083, 0.3863500754690888384, 0.4496377310517142845, 0.5147953269783583918, 0.5792399132410295248, 0.6418141777582890839, 0.7013585647860598460, 0.7607267659857199771, 0.8192220679243895631, 0.8787161693846299304, 0.9381473540533086242, 1.000000000000000000 ),
 .UNSPECIFIED. ) ;
#27602 = VERTEX_POINT ( 'NONE', #94647 ) ;
#27603 = CARTESIAN_POINT ( 'NONE',  ( -43.22287095715006444, -23.47596703998600276, 11.44779298504227683 ) ) ;
#27604 = CARTESIAN_POINT ( 'NONE',  ( -125.2228709571500644, -23.47596703998600631, 11.44779298504227860 ) ) ;
#27605 = LINE ( 'NONE', #59056, #69836 ) ;
#27606 = CARTESIAN_POINT ( 'NONE',  ( 1.511266892140219920, 20.53031905857337591, -1.500000000000002220 ) ) ;
#27607 = CARTESIAN_POINT ( 'NONE',  ( -4.138935798035190849, -21.16376344109877294, 11.49999999999999645 ) ) ;
#27608 = ORIENTED_EDGE ( 'NONE', *, *, #8179, .T. ) ;
#27609 = DIRECTION ( 'NONE',  ( -0.000000000000000000, 1.000000000000000000, -0.000000000000000000 ) ) ;
#27610 = LINE ( 'NONE', #36215, #22309 ) ;
#27611 = CARTESIAN_POINT ( 'NONE',  ( -97.58953762381672448, -23.48783264082478794, -1.443836473390061936 ) ) ;
#27612 = CARTESIAN_POINT ( 'NONE',  ( -11.77839732991513166, 18.97803183815481987, 11.49999999999998934 ) ) ;
#27613 = DIRECTION ( 'NONE',  ( -3.773278334453079618E-23, 0.9999999999976377785, 2.173523156925979975E-06 ) ) ;
#27614 = DIRECTION ( 'NONE',  ( 0.000000000000000000, -0.9999999999976377785, -2.173523156925979975E-06 ) ) ;
#27615 = ORIENTED_EDGE ( 'NONE', *, *, #64244, .F. ) ;
#27616 = LINE ( 'NONE', #74767, #17757 ) ;
#27617 = CARTESIAN_POINT ( 'NONE',  ( -96.58953762381672448, -23.48786465467241413, 11.44779295918254114 ) ) ;
#27618 = AXIS2_PLACEMENT_3D ( 'NONE', #88751, #50186, #42583 ) ;
#27619 = CARTESIAN_POINT ( 'NONE',  ( 19.90007246472742608, 6.374896562862660154, -1.500000000000002220 ) ) ;
#27620 = VERTEX_POINT ( 'NONE', #40863 ) ;
#27621 = EDGE_CURVE ( 'NONE', #99954, #2424, #32246, .T. ) ;
#27623 = ORIENTED_EDGE ( 'NONE', *, *, #48393, .F. ) ;
#27622 = CARTESIAN_POINT ( 'NONE',  ( -27.25988310792305214, 0.3587747205144265483, 30.32664379231667695 ) ) ;
#27624 = ORIENTED_EDGE ( 'NONE', *, *, #67495, .T. ) ;
#27625 = AXIS2_PLACEMENT_3D ( 'NONE', #98772, #90672, #53127 ) ;
#27626 = CARTESIAN_POINT ( 'NONE',  ( -100.5075804452173571, -24.73531770709095312, 8.716586749053508498 ) ) ;
#27627 = CARTESIAN_POINT ( 'NONE',  ( -20.44436638909326120, 5.324712401148210539, -1.500000000000002220 ) ) ;
#27628 = EDGE_CURVE ( 'NONE', #21942, #56196, #88048, .T. ) ;
#27629 = ORIENTED_EDGE ( 'NONE', *, *, #89079, .F. ) ;
#27630 = CARTESIAN_POINT ( 'NONE',  ( -28.52287095715005094, -24.34106804586823714, 0.6165375242712651804 ) ) ;
#27631 = DIRECTION ( 'NONE',  ( -0.2488812114211666759, -0.000000000000000000, -0.9685340172660599212 ) ) ;
#27632 = DIRECTION ( 'NONE',  ( -3.773278334453079618E-23, 0.9999999999976377785, 2.173523156925979975E-06 ) ) ;
#27633 = CARTESIAN_POINT ( 'NONE',  ( 10.86264265030973952, 5.965225279485574461, -28.05717073599341305 ) ) ;
#27634 = DIRECTION ( 'NONE',  ( -0.9951627101165076983, -0.09824042138329588947, -3.430045979798635096E-16 ) ) ;
#27635 = CARTESIAN_POINT ( 'NONE',  ( 19.97611268498323511, -8.487024919450899318, -1.500000000000002220 ) ) ;
#27636 = CARTESIAN_POINT ( 'NONE',  ( -80.48900664166535535, -25.24759804928183726, 7.101635288197144291 ) ) ;
#27638 = VERTEX_POINT ( 'NONE', #63729 ) ;
#27637 = CARTESIAN_POINT ( 'NONE',  ( 15.88595335714125589, -15.59144682577495189, 11.49999999999999645 ) ) ;
#27639 = CARTESIAN_POINT ( 'NONE',  ( -77.22287095715009286, -23.47593901973090524, -1.443836447538997980 ) ) ;
#27640 = CARTESIAN_POINT ( 'NONE',  ( 8.971512145086503409, -2.028487854913500144, 6.500000000000000000 ) ) ;
#27641 = CARTESIAN_POINT ( 'NONE',  ( -50.40445135320379677, -25.12298712672050982, 7.101635559041870494 ) ) ;
#27642 = ORIENTED_EDGE ( 'NONE', *, *, #60014, .T. ) ;
#27644 = VERTEX_POINT ( 'NONE', #26137 ) ;
#27643 = DIRECTION ( 'NONE',  ( 0.000000000000000000, 1.000000000000000000, 0.000000000000000000 ) ) ;
#27645 = ORIENTED_EDGE ( 'NONE', *, *, #91243, .F. ) ;
#27646 = CARTESIAN_POINT ( 'NONE',  ( -0.1426030150137701236, -21.20389190742571373, -1.497999999999532594 ) ) ;
#27647 = DIRECTION ( 'NONE',  ( 0.000000000000000000, -2.173523156925979552E-06, 0.9999999999976378895 ) ) ;
#27648 = EDGE_CURVE ( 'NONE', #74181, #94973, #44838, .T. ) ;
#27649 = CARTESIAN_POINT ( 'NONE',  ( 30.56047832681638354, -2.297196155479634516, 24.67598410064775649 ) ) ;
#27650 = CARTESIAN_POINT ( 'NONE',  ( -107.5228709571501042, -23.48783264083360578, -1.443836473376361118 ) ) ;
#27651 = PLANE ( 'NONE',  #70074 ) ;
#27652 = VERTEX_POINT ( 'NONE', #78912 ) ;
#27653 = CARTESIAN_POINT ( 'NONE',  ( 0.06232057257353295493, 19.38168652127415825, 11.49999999999999645 ) ) ;
#27654 = FACE_OUTER_BOUND ( 'NONE', #74310, .T. ) ;
#27655 = CARTESIAN_POINT ( 'NONE',  ( 3.503984654965784706, -22.18958196551723816, -1.500000000000002220 ) ) ;
#27656 = VERTEX_POINT ( 'NONE', #3329 ) ;
#27657 = CARTESIAN_POINT ( 'NONE',  ( 31.79364159983995464, -5.965225279485572685, -11.59305536555894278 ) ) ;
#27658 = CARTESIAN_POINT ( 'NONE',  ( 6.948977015814011615, 5.356774720514426491, -25.20533573604597066 ) ) ;
#27659 = B_SPLINE_CURVE_WITH_KNOTS ( 'NONE', 3,
 ( #62122, #32151, #78318, #14922, #77807, #54010 ),
 .UNSPECIFIED., .F., .F.,
 ( 4, 2, 4 ),
 ( 1.570887131794333942E-05, 0.001396322306279757387, 0.002776935741241571502 ),
 .UNSPECIFIED. ) ;
#27660 = PLANE ( 'NONE',  #6078 ) ;
#27661 = CARTESIAN_POINT ( 'NONE',  ( -97.24679249956406579, -24.75179208683297460, 8.640809912072082710 ) ) ;
#27662 = CARTESIAN_POINT ( 'NONE',  ( 19.39309126630920588, -2.812899550206792831, -1.500000000000002220 ) ) ;
#27663 = CARTESIAN_POINT ( 'NONE',  ( -46.48372047104909655, -24.65952944569304606, 1.056160979905696351 ) ) ;
#27664 = ORIENTED_EDGE ( 'NONE', *, *, #97905, .T. ) ;
#27665 = CARTESIAN_POINT ( 'NONE',  ( -2.508422780830330989, 21.39056295969660582, -1.500000000000002220 ) ) ;
#27666 = LINE ( 'NONE', #33775, #57713 ) ;
#27667 = CARTESIAN_POINT ( 'NONE',  ( -81.37613735670856840, -25.30394805385784807, 5.179459886602215235 ) ) ;
#27668 = CARTESIAN_POINT ( 'NONE',  ( -62.55620429048337883, -24.64965694238574656, 8.947790433994198267 ) ) ;
#27669 = AXIS2_PLACEMENT_3D ( 'NONE', #31731, #62697, #71804 ) ;
#27670 = LINE ( 'NONE', #95678, #45578 ) ;
#27671 = CARTESIAN_POINT ( 'NONE',  ( 22.09143763772896918, 6.410036269187016522, -1.500000000000002220 ) ) ;
#27672 = APPROVAL_STATUS ( 'not_yet_approved' ) ;
#27673 = CARTESIAN_POINT ( 'NONE',  ( -93.62287095715005592, -24.66019654487199730, 8.947790411086124607 ) ) ;
#27674 = CARTESIAN_POINT ( 'NONE',  ( -79.62287095715005592, -24.64898659630528854, 1.056161002820826145 ) ) ;
#27675 = CARTESIAN_POINT ( 'NONE',  ( -17.52916707085001136, 9.785066945116392745, 11.49999999999999645 ) ) ;
#27676 = CARTESIAN_POINT ( 'NONE',  ( -109.6441887128288784, -25.10927429713856540, 2.986266705731216664 ) ) ;
#27677 = CARTESIAN_POINT ( 'NONE',  ( -32.49648798523244153, -24.15620529776627734, 10.23563542870661358 ) ) ;
#27678 = CARTESIAN_POINT ( 'NONE',  ( -4.440151687742864617, -5.876774720514411854, 19.67013632031035897 ) ) ;
#27679 = CARTESIAN_POINT ( 'NONE',  ( -90.62287095715004170, -29.50250786944525672, 11.44777988621623344 ) ) ;
#27680 = CARTESIAN_POINT ( 'NONE',  ( -100.4498239493576648, -25.03284467579916495, 7.563174216508126158 ) ) ;
#27681 = CARTESIAN_POINT ( 'NONE',  ( 6.283368587668265448, -18.83516890145298106, 11.49999999999998934 ) ) ;
#27682 = ADVANCED_FACE ( 'NONE', ( #79416 ), #79918, .T. ) ;
#27683 = CARTESIAN_POINT ( 'NONE',  ( -113.5508063869240658, -24.65952944569304606, 1.056160979905704789 ) ) ;
#27684 = CARTESIAN_POINT ( 'NONE',  ( 11.88433821776028942, -15.71472908967258242, -1.500000000000002220 ) ) ;
#27685 = CARTESIAN_POINT ( 'NONE',  ( -42.53415887033509790, -24.51314013834315375, 0.6176544820404090697 ) ) ;
#27686 = ADVANCED_FACE ( 'NONE', ( #17022 ), #10245, .F. ) ;
#27687 = AXIS2_PLACEMENT_3D ( 'NONE', #93405, #77174, #76667 ) ;
#27688 = EDGE_CURVE ( 'NONE', #71376, #35617, #72322, .T. ) ;
#27689 = AXIS2_PLACEMENT_3D ( 'NONE', #29965, #91364, #77128 ) ;
#27690 = FACE_OUTER_BOUND ( 'NONE', #88412, .T. ) ;
#27691 = CARTESIAN_POINT ( 'NONE',  ( 2.909586618535765723, -6.376774720514411854, 19.75512108203924200 ) ) ;
#27692 = CARTESIAN_POINT ( 'NONE',  ( 18.87225196054570020, 8.368929400942139551, 11.49999999999999645 ) ) ;
#27693 = EDGE_CURVE ( 'NONE', #16980, #63531, #14031, .T. ) ;
#27694 = CARTESIAN_POINT ( 'NONE',  ( -128.5228709571501042, -24.51387760970726504, 9.387446482453400520 ) ) ;
#27695 = CARTESIAN_POINT ( 'NONE',  ( 19.67839991682829748, -11.23141783594569354, 11.49999999999999645 ) ) ;
#27696 = ORIENTED_EDGE ( 'NONE', *, *, #6248, .T. ) ;
#27697 = DIRECTION ( 'NONE',  ( -0.1478094111296165691, 0.9890158633619158257, -0.000000000000000000 ) ) ;
#27698 = CARTESIAN_POINT ( 'NONE',  ( 29.75292639967170771, 5.303223407918566501, 26.69524796275325684 ) ) ;
#27699 = ADVANCED_FACE ( 'NONE', ( #1309 ), #63216, .T. ) ;
#27700 = DIRECTION ( 'NONE',  ( -3.773278334453079618E-23, 0.9999999999976377785, 2.173523156925979975E-06 ) ) ;
#27701 = CARTESIAN_POINT ( 'NONE',  ( -2.188401442307694289, -6.376774720514411854, 19.46153846153846700 ) ) ;
#27702 = EDGE_LOOP ( 'NONE', ( #12373, #87545, #69258, #79578 ) ) ;
#27703 = EDGE_LOOP ( 'NONE', ( #5628, #33746, #40206, #78734 ) ) ;
#27704 = CARTESIAN_POINT ( 'NONE',  ( -49.62287095715005592, -29.50247984919015209, -1.443849546365058689 ) ) ;
#27705 = CARTESIAN_POINT ( 'NONE',  ( -1.055347110731411187, -22.84297022578905612, 11.49999999999998934 ) ) ;
#27706 = DIRECTION ( 'NONE',  ( -1.000000000000000000, 0.000000000000000000, -0.000000000000000000 ) ) ;
#27707 = CARTESIAN_POINT ( 'NONE',  ( 19.98343133220876666, -8.209121646405339590, -1.500000000000002220 ) ) ;
#27708 = CARTESIAN_POINT ( 'NONE',  ( -113.5541376391153960, -24.15620529776628800, 10.23563542870659582 ) ) ;
#27709 = DIRECTION ( 'NONE',  ( 0.000000000000000000, -0.9999999999976377785, -2.173523156925979128E-06 ) ) ;
#27710 = CARTESIAN_POINT ( 'NONE',  ( 19.88857169258762170, 10.62688394266798930, 11.49999999999999645 ) ) ;
#27711 = ORIENTED_EDGE ( 'NONE', *, *, #70987, .F. ) ;
#27712 = CARTESIAN_POINT ( 'NONE',  ( 5.399550031317769339, -5.965225279485594001, -28.54570968858208246 ) ) ;
#27713 = CARTESIAN_POINT ( 'NONE',  ( 21.30657626330824783, 5.479626006175059239, 11.49999999999998934 ) ) ;
#27714 = CARTESIAN_POINT ( 'NONE',  ( -111.5512764650698614, -24.51314013834316796, 0.6176544820404207270 ) ) ;
#27715 = PLANE ( 'NONE',  #31429 ) ;
#27716 = ORIENTED_EDGE ( 'NONE', *, *, #53860, .F. ) ;
#27717 = CARTESIAN_POINT ( 'NONE',  ( -89.62287095715004170, -24.66019654487199020, 8.947790411086128159 ) ) ;
#27718 = DIRECTION ( 'NONE',  ( 1.156482317317878549E-14, 0.000000000000000000, 1.000000000000000000 ) ) ;
#27719 = VERTEX_POINT ( 'NONE', #13394 ) ;
#27720 = DIRECTION ( 'NONE',  ( 0.000000000000000000, 0.000000000000000000, -1.000000000000000000 ) ) ;
#27721 = ORIENTED_EDGE ( 'NONE', *, *, #97384, .T. ) ;
#27722 = ORIENTED_EDGE ( 'NONE', *, *, #69596, .F. ) ;
#27723 = VERTEX_POINT ( 'NONE', #81431 ) ;
#27724 = CARTESIAN_POINT ( 'NONE',  ( 0.000000000000000000, -0.5000000000000000000, 0.000000000000000000 ) ) ;
#27725 = DIRECTION ( 'NONE',  ( -3.773278334453080206E-23, 0.9999999999976377785, 2.173523156925979975E-06 ) ) ;
#27726 = CARTESIAN_POINT ( 'NONE',  ( -57.62367078942418885, -24.65952944569304606, 1.056160979905698571 ) ) ;
#27727 = CARTESIAN_POINT ( 'NONE',  ( 1.124825640313904973, 20.40429917142216354, -1.500000000000002220 ) ) ;
#27728 = ORIENTED_EDGE ( 'NONE', *, *, #13386, .F. ) ;
#27729 = CARTESIAN_POINT ( 'NONE',  ( -1.030996059302438761, -5.876774720514415407, 20.06599527532949878 ) ) ;
#27730 = CARTESIAN_POINT ( 'NONE',  ( -51.15652172324698910, -25.15690241117504655, 3.041046503643967114 ) ) ;
#27731 = EDGE_CURVE ( 'NONE', #78484, #64607, #66727, .T. ) ;
#27732 = CARTESIAN_POINT ( 'NONE',  ( -105.5110145565341924, -24.63355581998386867, 0.9682620441943899925 ) ) ;
#27733 = DIRECTION ( 'NONE',  ( -1.000000000000000000, 1.232047923278981953E-16, 0.000000000000000000 ) ) ;
#27734 = VERTEX_POINT ( 'NONE', #60103 ) ;
#27735 = CARTESIAN_POINT ( 'NONE',  ( -27.75618988833547718, -25.21531659070602771, 2.278559006348844118 ) ) ;
#27736 = CARTESIAN_POINT ( 'NONE',  ( -27.75512851621423138, -24.63646064523983981, 8.250987297651915853 ) ) ;
#27737 = ORIENTED_EDGE ( 'NONE', *, *, #92274, .F. ) ;
#27738 = CARTESIAN_POINT ( 'NONE',  ( -18.43438512255917772, -9.567967903218889347, -1.500000000000002220 ) ) ;
#27740 = EDGE_CURVE ( 'NONE', #78010, #29283, #3817, .T. ) ;
#27739 = ORIENTED_EDGE ( 'NONE', *, *, #91919, .F. ) ;
#27742 = VERTEX_POINT ( 'NONE', #82414 ) ;
#27741 = DIRECTION ( 'NONE',  ( 1.000000000000000000, 3.773278334444166432E-23, 8.201307841325785021E-29 ) ) ;
#27743 = LINE ( 'NONE', #36354, #60044 ) ;
#27744 = CARTESIAN_POINT ( 'NONE',  ( -51.59601236526418688, -25.30186097039144499, 5.321576288067153548 ) ) ;
#27745 = VERTEX_POINT ( 'NONE', #35261 ) ;
#27746 = ORIENTED_EDGE ( 'NONE', *, *, #8933, .F. ) ;
#27747 = CARTESIAN_POINT ( 'NONE',  ( -33.52287095715006870, -23.95044443724991368, 10.65354141964649948 ) ) ;
#27748 = CARTESIAN_POINT ( 'NONE',  ( 5.802984775641024662, -6.376774720514402972, 18.35026041666666430 ) ) ;
#27749 = DIRECTION ( 'NONE',  ( 0.000000000000000000, -1.000000000000000000, 0.000000000000000000 ) ) ;
#27750 = CARTESIAN_POINT ( 'NONE',  ( -43.64074078125805300, -24.15620529776627379, 10.23563542870661180 ) ) ;
#27752 = VERTEX_POINT ( 'NONE', #44370 ) ;
#27751 = CARTESIAN_POINT ( 'NONE',  ( 10.71795340210964120, -19.33932934982082585, 11.49999999999999645 ) ) ;
#27753 = DIRECTION ( 'NONE',  ( -1.000000000000000000, 0.000000000000000000, 0.000000000000000000 ) ) ;
#27754 = CARTESIAN_POINT ( 'NONE',  ( 19.13181028273733375, 12.02906595412573232, -1.500000000000002220 ) ) ;
#27756 = ORIENTED_EDGE ( 'NONE', *, *, #44863, .T. ) ;
#27755 = CARTESIAN_POINT ( 'NONE',  ( -115.5500777739175788, -25.00182538069147142, 7.747789668545041586 ) ) ;
#27757 = VECTOR ( 'NONE', #5066, 1000.000000000000227 ) ;
#27758 = ORIENTED_EDGE ( 'NONE', *, *, #5898, .T. ) ;
#27759 =( GEOMETRIC_REPRESENTATION_CONTEXT ( 3 ) GLOBAL_UNCERTAINTY_ASSIGNED_CONTEXT ( ( #29671 ) ) GLOBAL_UNIT_ASSIGNED_CONTEXT ( ( #46529, #53155, #851 ) ) REPRESENTATION_CONTEXT ( 'NONE', 'WORKASPACE' ) );
#27760 = CARTESIAN_POINT ( 'NONE',  ( -78.52287095715004739, -24.66019654487199375, 8.947790411086119278 ) ) ;
#27761 = CC_DESIGN_PERSON_AND_ORGANIZATION_ASSIGNMENT ( #25663, #34783, ( #47237 ) ) ;
#27762 = CARTESIAN_POINT ( 'NONE',  ( -78.62287095715007013, -23.72773821059535848, 11.05748984161097503 ) ) ;
#27763 = ORIENTED_EDGE ( 'NONE', *, *, #79480, .F. ) ;
#27764 = CARTESIAN_POINT ( 'NONE',  ( -12.03079493616482765, -17.41531974249929249, -1.500000000000002220 ) ) ;
#27765 = DIRECTION ( 'NONE',  ( 0.000000000000000000, 0.000000000000000000, -1.000000000000000000 ) ) ;
#27766 = CARTESIAN_POINT ( 'NONE',  ( -20.27875734969026311, 3.456774720514426136, 22.85402280011862430 ) ) ;
#27767 = CARTESIAN_POINT ( 'NONE',  ( 15.82088602905085750, -15.72875506571707760, -1.500000000000002220 ) ) ;
#27768 = DIRECTION ( 'NONE',  ( 0.7682573101345366862, 0.000000000000000000, -0.6401411605457395515 ) ) ;
#27769 = VERTEX_POINT ( 'NONE', #75295 ) ;
#27770 = LINE ( 'NONE', #59223, #2783 ) ;
#27771 = CARTESIAN_POINT ( 'NONE',  ( -29.52287095715006160, -24.56627961951908645, 8.947790480023282811 ) ) ;
#27772 = EDGE_CURVE ( 'NONE', #60342, #33324, #41515, .T. ) ;
#27773 = PLANE ( 'NONE',  #39787 ) ;
#27774 = CARTESIAN_POINT ( 'NONE',  ( -25.92875734969025814, 6.376774720514426953, 26.43402280011862615 ) ) ;
#27775 = CARTESIAN_POINT ( 'NONE',  ( 14.32981562401322506, -13.22600733894156200, 11.49999999999998934 ) ) ;
#27776 = CARTESIAN_POINT ( 'NONE',  ( 18.57079561221590325, -10.74342183689097574, 11.49999999999998934 ) ) ;
#27777 = CARTESIAN_POINT ( 'NONE',  ( -27.65533724976895869, -24.57999497193509342, 1.629628004430854871 ) ) ;
#27778 = DIRECTION ( 'NONE',  ( 0.000000000000000000, 0.9999999999976377785, 2.173523156925979975E-06 ) ) ;
#27779 = LINE ( 'NONE', #43999, #46018 ) ;
#27780 = CARTESIAN_POINT ( 'NONE',  ( 22.53581206741051446, 3.480912172000575122, -1.500000000000002220 ) ) ;
#27781 = B_SPLINE_CURVE_WITH_KNOTS ( 'NONE', 3,
 ( #82941, #51516, #60635, #44404 ),
 .UNSPECIFIED., .F., .F.,
 ( 4, 4 ),
 ( 1.387778780781445521E-17, 9.999999999997510880E-05 ),
 .UNSPECIFIED. ) ;
#27782 = PERSON_AND_ORGANIZATION ( #70597, #27821 ) ;
#27783 = FACE_OUTER_BOUND ( 'NONE', #50321, .T. ) ;
#27784 = DIRECTION ( 'NONE',  ( -1.000000000000000000, -0.000000000000000000, -0.000000000000000000 ) ) ;
#27785 = CARTESIAN_POINT ( 'NONE',  ( 15.68239283413728735, 12.23493734220040530, 11.49999999999999645 ) ) ;
#27786 = CARTESIAN_POINT ( 'NONE',  ( -104.5222000018547988, -23.48783264082477373, -1.443836473390085695 ) ) ;
#27787 = LINE ( 'NONE', #18670, #81400 ) ;
#27788 = CARTESIAN_POINT ( 'NONE',  ( -98.62287095715005592, -23.47593901973091235, -1.443836447539001089 ) ) ;
#27789 = ADVANCED_FACE ( 'NONE', ( #12895 ), #20020, .T. ) ;
#27790 = VERTEX_POINT ( 'NONE', #36252 ) ;
#27791 = DIRECTION ( 'NONE',  ( -0.000000000000000000, 1.000000000000000000, -0.000000000000000000 ) ) ;
#27792 = LINE ( 'NONE', #88703, #23156 ) ;
#27793 = CARTESIAN_POINT ( 'NONE',  ( 12.82194709444435077, -17.51738216156474337, -1.500000000000002220 ) ) ;
#27794 = CARTESIAN_POINT ( 'NONE',  ( -11.64875734969026233, 5.965225279485572685, 31.02402280011862246 ) ) ;
#27795 = CARTESIAN_POINT ( 'NONE',  ( 0.4223197742854877812, 19.52780805513575402, -1.500000000000002220 ) ) ;
#27796 = CARTESIAN_POINT ( 'NONE',  ( -55.61923469880454718, -23.48786465467241058, 11.44779295918254647 ) ) ;
#27797 = VERTEX_POINT ( 'NONE', #96642 ) ;
#27798 = COORDINATED_UNIVERSAL_TIME_OFFSET ( 0, 0, .AHEAD. ) ;
#27799 = EDGE_CURVE ( 'NONE', #24634, #79371, #75457, .T. ) ;
#27800 = CARTESIAN_POINT ( 'NONE',  ( -81.52287095715006160, -24.64965694238408034, 8.947790433994198267 ) ) ;
#27801 = CARTESIAN_POINT ( 'NONE',  ( 19.09590870110849181, 7.302211495713927469, 11.49999999999999645 ) ) ;
#27802 = CARTESIAN_POINT ( 'NONE',  ( -47.52287095715006870, -23.96177878511308634, 10.65340807706330573 ) ) ;
#27803 = AXIS2_PLACEMENT_3D ( 'NONE', #7436, #59751, #60253 ) ;
#27804 = EDGE_CURVE ( 'NONE', #14758, #48827, #72971, .T. ) ;
#27805 = CARTESIAN_POINT ( 'NONE',  ( -93.52287095715006160, -29.50250243563736774, 8.947779886222139822 ) ) ;
#27806 = VERTEX_POINT ( 'NONE', #90526 ) ;
#27807 = CARTESIAN_POINT ( 'NONE',  ( -55.58953762381673158, -23.48786465467240703, 11.44779295918255180 ) ) ;
#27808 = CARTESIAN_POINT ( 'NONE',  ( -43.52287095715007581, -24.66019654487199375, 8.947790411086128159 ) ) ;
#27809 = LINE ( 'NONE', #60275, #92209 ) ;
#27810 = B_SPLINE_CURVE_WITH_KNOTS ( 'NONE', 3,
 ( #12206, #88349, #42197, #4115, #95956, #27946, #19322, #97454 ),
 .UNSPECIFIED., .F., .F.,
 ( 4, 2, 2, 4 ),
 ( -0.001240666984355833250, -0.0002401179793394929429, 0.0007604310256768473646, 0.002761529035709531232 ),
 .UNSPECIFIED. ) ;
#27811 = EDGE_CURVE ( 'NONE', #67935, #48203, #95958, .T. ) ;
#27812 = FACE_OUTER_BOUND ( 'NONE', #90978, .T. ) ;
#27813 = VERTEX_POINT ( 'NONE', #74312 ) ;
#27814 = CARTESIAN_POINT ( 'NONE',  ( 6.351517594976544778, -6.376774720514417183, 20.09206396488320578 ) ) ;
#27815 = VECTOR ( 'NONE', #55271, 1000.000000000000114 ) ;
#27816 = CARTESIAN_POINT ( 'NONE',  ( -4.971178678486217528, -22.47594730032828281, 11.49999999999999645 ) ) ;
#27817 = CARTESIAN_POINT ( 'NONE',  ( 0.8422786845129024424, 22.77647355728978340, -1.500000000000002220 ) ) ;
#27818 = CARTESIAN_POINT ( 'NONE',  ( 3.671066620544169101, -6.376774720514424288, 21.47597918715562670 ) ) ;
#27819 = CARTESIAN_POINT ( 'NONE',  ( -122.5562042904833930, -24.64898659630528854, 1.056161002820831474 ) ) ;
#27820 = CARTESIAN_POINT ( 'NONE',  ( -49.72668233141190797, -25.22502443621784707, 3.520239836515675513 ) ) ;
#27821 = ORGANIZATION ( 'UNSPECIFIED', 'UNSPECIFIED', '' ) ;
#27822 = CARTESIAN_POINT ( 'NONE',  ( -53.22287095715007865, -23.47593901973090169, -1.443836447538997758 ) ) ;
#27823 = CARTESIAN_POINT ( 'NONE',  ( -44.58953762381671737, -23.48783264082478084, -1.443836473390072150 ) ) ;
#27824 = B_SPLINE_CURVE_WITH_KNOTS ( 'NONE', 3,
 ( #29736, #60704, #91625, #22108, #30734, #53090 ),
 .UNSPECIFIED., .F., .F.,
 ( 4, 2, 4 ),
 ( 1.570887131794176733E-05, 0.001396322306279759555, 0.002776935741241577573 ),
 .UNSPECIFIED. ) ;
#27825 = CARTESIAN_POINT ( 'NONE',  ( -19.20277006422315225, 10.48866939257135833, -1.500000000000002220 ) ) ;
#27826 = CARTESIAN_POINT ( 'NONE',  ( -59.55620429048336462, -24.64965694238574301, 8.947790433994201820 ) ) ;
#27827 = FACE_OUTER_BOUND ( 'NONE', #5951, .T. ) ;
#27828 = CARTESIAN_POINT ( 'NONE',  ( 17.51792015816173986, -5.965225279485572685, 29.01255224319336889 ) ) ;
#27829 = CARTESIAN_POINT ( 'NONE',  ( -96.52287095715006160, -24.64965694238575011, 8.947790433994194714 ) ) ;
#27830 = ORIENTED_EDGE ( 'NONE', *, *, #7617, .T. ) ;
#27831 = CARTESIAN_POINT ( 'NONE',  ( -13.80512455850298714, -15.04058748057734896, -1.500000000000002220 ) ) ;
#27832 = ORIENTED_EDGE ( 'NONE', *, *, #39212, .T. ) ;
#27833 = ORIENTED_EDGE ( 'NONE', *, *, #14986, .F. ) ;
#27834 = EDGE_LOOP ( 'NONE', ( #45339, #1885, #60305, #27204 ) ) ;
#27835 = EDGE_LOOP ( 'NONE', ( #63983, #70759 ) ) ;
#27836 = CARTESIAN_POINT ( 'NONE',  ( 23.03040035405544472, 1.057182387018521963, 11.49999999999998934 ) ) ;
#27837 = CARTESIAN_POINT ( 'NONE',  ( 15.03086228770605004, -5.128928118853483653, -26.95277610321158690 ) ) ;
#27838 = CARTESIAN_POINT ( 'NONE',  ( 18.08294815051442583, 9.098846914115775064, -1.500000000000002220 ) ) ;
#27839 = ORIENTED_EDGE ( 'NONE', *, *, #4372, .F. ) ;
#27840 = DIRECTION ( 'NONE',  ( 0.000000000000000000, -0.9999999999976377785, -2.173523156925979975E-06 ) ) ;
#27841 = CARTESIAN_POINT ( 'NONE',  ( -62.62287095715004881, -29.50250243563736774, 8.947779886222145151 ) ) ;
#27842 = CARTESIAN_POINT ( 'NONE',  ( 22.02124265030973760, 7.743225279485574042, 18.45402280011862217 ) ) ;
#27843 = DIRECTION ( 'NONE',  ( 0.000000000000000000, -1.000000000000000000, 0.000000000000000000 ) ) ;
#27845 = ORIENTED_EDGE ( 'NONE', *, *, #95007, .T. ) ;
#27844 = CARTESIAN_POINT ( 'NONE',  ( 21.32124590881793225, -1.116183810207903804, 11.49999999999999645 ) ) ;
#27846 = CARTESIAN_POINT ( 'NONE',  ( -91.62287095715004170, -29.50247984919015209, -1.443849546365051806 ) ) ;
#27847 = ORIENTED_EDGE ( 'NONE', *, *, #64465, .F. ) ;
#27848 = CARTESIAN_POINT ( 'NONE',  ( -20.07822104958740539, -9.643837532803976487, 11.49999999999998934 ) ) ;
#27849 = CARTESIAN_POINT ( 'NONE',  ( -17.42616458466809704, -11.11377323884725321, 11.49999999999998934 ) ) ;
#27850 = ORIENTED_EDGE ( 'NONE', *, *, #75789, .F. ) ;
#27851 = ADVANCED_FACE ( 'NONE', ( #21009 ), #51478, .F. ) ;
#27852 = AXIS2_PLACEMENT_3D ( 'NONE', #65473, #35501, #58834 ) ;
#27853 = CARTESIAN_POINT ( 'NONE',  ( 3.051095722660301934, -5.876774720514410077, 19.07493897947323092 ) ) ;
#27854 = ORIENTED_EDGE ( 'NONE', *, *, #21970, .T. ) ;
#27855 = PLANE ( 'NONE',  #13713 ) ;
#27856 = VERTEX_POINT ( 'NONE', #5293 ) ;
#27857 = DIRECTION ( 'NONE',  ( -0.000000000000000000, 1.000000000000000000, -0.000000000000000000 ) ) ;
#27858 = CARTESIAN_POINT ( 'NONE',  ( -11.35812032211249090, 17.58211214940072864, -1.500000000000002220 ) ) ;
#27859 = B_SPLINE_CURVE_WITH_KNOTS ( 'NONE', 3,
 ( #51754, #13167, #28905, #52253 ),
 .UNSPECIFIED., .F., .F.,
 ( 4, 4 ),
 ( 0.000000000000000000, 9.999999999998897304E-05 ),
 .UNSPECIFIED. ) ;
#27860 = CARTESIAN_POINT ( 'NONE',  ( -20.57654891367511851, 7.437132321665034240, 11.49999999999999645 ) ) ;
#27861 = CARTESIAN_POINT ( 'NONE',  ( -73.51656078076787537, -23.73791477778911840, 11.05961554403170766 ) ) ;
#27862 = CARTESIAN_POINT ( 'NONE',  ( -21.16606679798846358, 7.723709098063864076, 11.49999999999998934 ) ) ;
#27863 = CARTESIAN_POINT ( 'NONE',  ( 19.44712688777480736, 7.780496645421295376, -1.500000000000002220 ) ) ;
#27864 = CARTESIAN_POINT ( 'NONE',  ( -91.52287095715006160, -23.47593901973090524, -1.443836447538996648 ) ) ;
#27865 = CARTESIAN_POINT ( 'NONE',  ( 6.351517594976544778, -5.876774720514417183, 20.09206396488320578 ) ) ;
#27866 = CARTESIAN_POINT ( 'NONE',  ( -119.5880674028319959, -24.66019654487200441, 8.947790411086108620 ) ) ;
#27867 = CARTESIAN_POINT ( 'NONE',  ( -126.6228709571500843, -24.66019654487200441, 8.947790411086119278 ) ) ;
#27868 = ORIENTED_EDGE ( 'NONE', *, *, #66252, .T. ) ;
#27869 = B_SPLINE_CURVE_WITH_KNOTS ( 'NONE', 3,
 ( #53007, #52500, #82930, #68223 ),
 .UNSPECIFIED., .F., .F.,
 ( 4, 4 ),
 ( 0.8503931694243046513, 0.8593996006964206291 ),
 .UNSPECIFIED. ) ;
#27870 = ORIENTED_EDGE ( 'NONE', *, *, #16116, .F. ) ;
#27871 = EDGE_LOOP ( 'NONE', ( #99688, #68976, #16098, #65823 ) ) ;
#27872 = VECTOR ( 'NONE', #52885, 1000.000000000000227 ) ;
#27873 = CARTESIAN_POINT ( 'NONE',  ( -66.62364616943149542, -24.65952944569304250, 1.056160979905692798 ) ) ;
#27874 = EDGE_CURVE ( 'NONE', #74792, #64635, #77255, .T. ) ;
#27875 = CARTESIAN_POINT ( 'NONE',  ( 11.41860910855227829, 18.14899599152127152, -1.500000000000002220 ) ) ;
#27876 = CARTESIAN_POINT ( 'NONE',  ( 0.03625801282051022839, -5.876774720514410077, 19.27714342948718240 ) ) ;
#27877 = VERTEX_POINT ( 'NONE', #29126 ) ;
#27878 = CARTESIAN_POINT ( 'NONE',  ( 16.98782256641479904, -12.52229676876588371, -1.500000000000002220 ) ) ;
#27879 = CARTESIAN_POINT ( 'NONE',  ( -2.872281323269014752, 4.293056017849825601, 1.999999999999999556 ) ) ;
#27880 = CARTESIAN_POINT ( 'NONE',  ( 2.590395174287518643, -6.376774720514415407, 20.05492615153064762 ) ) ;
#27881 = ADVANCED_FACE ( 'NONE', ( #91025 ), #21498, .T. ) ;
#27882 = CARTESIAN_POINT ( 'NONE',  ( -20.27875734969026311, -6.143225279485574397, 24.00402280011862288 ) ) ;
#27883 = LINE ( 'NONE', #58840, #66969 ) ;
#27884 = CARTESIAN_POINT ( 'NONE',  ( 33.00535138976592719, -3.570691370340881576, -12.97242311383975988 ) ) ;
#27885 = CARTESIAN_POINT ( 'NONE',  ( -18.17467834739497690, 12.62983929299386965, -1.500000000000002220 ) ) ;
#27886 = CARTESIAN_POINT ( 'NONE',  ( -116.5166246991671386, -24.51314013834316086, 0.6176544820404277214 ) ) ;
#27887 = CARTESIAN_POINT ( 'NONE',  ( -109.4424681886586228, -25.30227564393651818, 5.310848485335579738 ) ) ;
#27888 = CARTESIAN_POINT ( 'NONE',  ( 3.509873074917118085, 5.965225279485572685, 29.15869884040363758 ) ) ;
#27889 = EDGE_CURVE ( 'NONE', #72799, #46688, #68105, .T. ) ;
#27890 = EDGE_CURVE ( 'NONE', #47659, #55720, #97221, .T. ) ;
#27891 = LINE ( 'NONE', #51233, #36613 ) ;
#27892 = AXIS2_PLACEMENT_3D ( 'NONE', #21915, #29539, #90945 ) ;
#27894 = EDGE_CURVE ( 'NONE', #5514, #31628, #84411, .T. ) ;
#27893 = APPROVAL_PERSON_ORGANIZATION ( #83941, #68642, #22520 ) ;
#27895 = CARTESIAN_POINT ( 'NONE',  ( 19.36035776617087123, -9.008237321879198234, -1.500000000000002220 ) ) ;
#27896 = CARTESIAN_POINT ( 'NONE',  ( -26.19073949106259391, -24.93562033171584957, 6.009727169100417044 ) ) ;
#27897 = CARTESIAN_POINT ( 'NONE',  ( -90.70924515653385356, -25.26266127311081888, 3.981777872396910389 ) ) ;
#27898 = CARTESIAN_POINT ( 'NONE',  ( -64.60342376047213975, -23.73791477778911840, 11.05961554403170766 ) ) ;
#27899 = CARTESIAN_POINT ( 'NONE',  ( -81.39459688428541995, -25.20426285083167173, 6.569653346528638416 ) ) ;
#27900 = CARTESIAN_POINT ( 'NONE',  ( 11.26306171725914851, -19.60737681494043727, -1.500000000000002220 ) ) ;
#27901 = B_SPLINE_CURVE_WITH_KNOTS ( 'NONE', 3,
 ( #63856, #95279, #70443, #25765, #24260, #33370 ),
 .UNSPECIFIED., .F., .F.,
 ( 4, 2, 4 ),
 ( 1.570755371633856203E-05, 0.001396183895866087319, 0.002776660238015836012 ),
 .UNSPECIFIED. ) ;
#27902 = VERTEX_POINT ( 'NONE', #29624 ) ;
#27904 = LINE ( 'NONE', #76066, #61235 ) ;
#27903 = B_SPLINE_CURVE_WITH_KNOTS ( 'NONE', 3,
 ( #27110, #48957, #11382, #49967 ),
 .UNSPECIFIED., .F., .F.,
 ( 4, 4 ),
 ( 0.000000000000000000, 0.001261718750000008493 ),
 .UNSPECIFIED. ) ;
#27905 = CARTESIAN_POINT ( 'NONE',  ( -79.56369746381113828, -23.48783264082476308, -1.443836473390096575 ) ) ;
#27906 = CARTESIAN_POINT ( 'NONE',  ( 9.261118129494249729, -17.44851725036260248, 11.49999999999999645 ) ) ;
#27907 = CARTESIAN_POINT ( 'NONE',  ( -74.62287095715005592, -23.48783264082478794, -1.443836473390067265 ) ) ;
#27908 = CARTESIAN_POINT ( 'NONE',  ( -47.62287095715004881, -24.64898659630367916, 1.056161002820821038 ) ) ;
#27909 = ADVANCED_FACE ( 'NONE', ( #61599 ), #84904, .T. ) ;
#27910 = VERTEX_POINT ( 'NONE', #8286 ) ;
#27911 = DIRECTION ( 'NONE',  ( -1.000000000000000000, -3.773278334444167608E-23, -8.201307833595939069E-29 ) ) ;
#27912 = CARTESIAN_POINT ( 'NONE',  ( -29.81001385051325414, -24.60094546151839623, 4.645691122018320129 ) ) ;
#27913 = CARTESIAN_POINT ( 'NONE',  ( 2.246611357655420083, -0.1632191352058117717, 0.1632191352058111888 ) ) ;
#27914 = CARTESIAN_POINT ( 'NONE',  ( -21.09935167195790839, -4.734744157926700225, 11.49999999999998934 ) ) ;
#27915 = LINE ( 'NONE', #52753, #51232 ) ;
#27916 = CARTESIAN_POINT ( 'NONE',  ( 2.021814659504407579E-13, -19.30000000000000426, -1.500000000000002220 ) ) ;
#27917 = CARTESIAN_POINT ( 'NONE',  ( -109.6228709571500559, -23.47593901973091235, -1.443836447538999312 ) ) ;
#27918 = DIRECTION ( 'NONE',  ( -3.773278334444167608E-23, 1.000000000000000000, 0.000000000000000000 ) ) ;
#27919 = CARTESIAN_POINT ( 'NONE',  ( -6.431973572030615038, 18.70533856667250916, -1.500000000000002220 ) ) ;
#27920 = ORIENTED_EDGE ( 'NONE', *, *, #14792, .F. ) ;
#27921 = CARTESIAN_POINT ( 'NONE',  ( 15.52975653788041122, 12.98207780544785628, 11.49999999999999645 ) ) ;
#27922 = CARTESIAN_POINT ( 'NONE',  ( -54.52287095715005449, -24.66019654487198665, 8.947790411086121054 ) ) ;
#27923 = B_SPLINE_CURVE_WITH_KNOTS ( 'NONE', 3,
 ( #60887, #77581, #86212, #7585, #91816, #23803 ),
 .UNSPECIFIED., .F., .F.,
 ( 4, 2, 4 ),
 ( 0.000000000000000000, 0.001380901958385387894, 0.002761803916770775788 ),
 .UNSPECIFIED. ) ;
#27924 = EDGE_CURVE ( 'NONE', #85301, #39996, #87518, .T. ) ;
#27926 = AXIS2_PLACEMENT_3D ( 'NONE', #73939, #87159, #48619 ) ;
#27925 = DIRECTION ( 'NONE',  ( 0.000000000000000000, 2.173523156925980399E-06, -0.9999999999976378895 ) ) ;
#27927 = EDGE_CURVE ( 'NONE', #18921, #35831, #46350, .T. ) ;
#27928 = EDGE_LOOP ( 'NONE', ( #89371, #91473, #14177, #20610 ) ) ;
#27929 = CARTESIAN_POINT ( 'NONE',  ( -110.5895376238167103, -24.99132157543166954, 2.256160258750667502 ) ) ;
#27930 = CARTESIAN_POINT ( 'NONE',  ( 12.88745205064172694, -3.316774720517230435, -28.14312002837575477 ) ) ;
#27931 = CARTESIAN_POINT ( 'NONE',  ( -75.58953762381673869, -23.48783264082478084, -1.443836473390065489 ) ) ;
#27932 = PLANE ( 'NONE',  #26283 ) ;
#27933 = CARTESIAN_POINT ( 'NONE',  ( -51.39961447129974204, -25.19579413596467177, 6.633757500754181358 ) ) ;
#27934 = CARTESIAN_POINT ( 'NONE',  ( 3.179702300980958185, 19.78100630842630281, -1.500000000000002220 ) ) ;
#27935 = EDGE_CURVE ( 'NONE', #41575, #98063, #44917, .T. ) ;
#27936 = FACE_OUTER_BOUND ( 'NONE', #67071, .T. ) ;
#27937 = EDGE_LOOP ( 'NONE', ( #15788, #48826, #8215 ) ) ;
#27938 = EDGE_CURVE ( 'NONE', #70560, #78258, #99926, .T. ) ;
#27939 = B_SPLINE_CURVE_WITH_KNOTS ( 'NONE', 3,
 ( #24772, #55754, #77553, #61363 ),
 .UNSPECIFIED., .F., .F.,
 ( 4, 4 ),
 ( 0.000000000000000000, 9.999999999999592548E-05 ),
 .UNSPECIFIED. ) ;
#27940 = EDGE_CURVE ( 'NONE', #48556, #45754, #10059, .T. ) ;
#27941 = CARTESIAN_POINT ( 'NONE',  ( -73.62287095715004170, -23.72773821059535848, 11.05748984161097681 ) ) ;
#27942 = AXIS2_PLACEMENT_3D ( 'NONE', #91176, #36897, #6942 ) ;
#27943 = CARTESIAN_POINT ( 'NONE',  ( -117.5228709571500758, -24.64965694238408034, 8.947790433994191162 ) ) ;
#27944 = CARTESIAN_POINT ( 'NONE',  ( -84.62287095715005592, -23.47593901973091235, -1.443836447539004642 ) ) ;
#27945 = AXIS2_PLACEMENT_3D ( 'NONE', #18203, #63908, #57291 ) ;
#27946 = CARTESIAN_POINT ( 'NONE',  ( -105.5228709571500474, -24.14321612903114200, -0.2833117244521580758 ) ) ;
#27947 = DIRECTION ( 'NONE',  ( -3.773278334453080206E-23, 0.9999999999976377785, 2.173523156925979975E-06 ) ) ;
#27948 = CARTESIAN_POINT ( 'NONE',  ( -24.97666371003640151, -5.965225279485592225, -15.72894043976419098 ) ) ;
#27949 = VERTEX_POINT ( 'NONE', #38230 ) ;
#27950 = CARTESIAN_POINT ( 'NONE',  ( 18.28078834835902455, 8.925752885971231620, -1.500000000000002220 ) ) ;
#27951 = ORIENTED_EDGE ( 'NONE', *, *, #13400, .F. ) ;
#27952 = CARTESIAN_POINT ( 'NONE',  ( 9.743704349311032686, 20.77413290702584092, -1.500000000000002220 ) ) ;
#27953 = CARTESIAN_POINT ( 'NONE',  ( -32.48286750831535841, -24.51314013834315375, 0.6176544820404111791 ) ) ;
#27954 = ORIENTED_EDGE ( 'NONE', *, *, #18529, .F. ) ;
#27955 = CARTESIAN_POINT ( 'NONE',  ( -50.40895856474225667, -25.03284467579915784, 7.563174216508125269 ) ) ;
#27956 = CARTESIAN_POINT ( 'NONE',  ( 1.255616527394258553, 17.95615290467683778, -9.000000000000000000 ) ) ;
#27957 = AXIS2_PLACEMENT_3D ( 'NONE', #27421, #66006, #33528 ) ;
#27958 = DIRECTION ( 'NONE',  ( 0.000000000000000000, 0.000000000000000000, 1.000000000000000000 ) ) ;
#27960 = ORIENTED_EDGE ( 'NONE', *, *, #45465, .F. ) ;
#27959 = CARTESIAN_POINT ( 'NONE',  ( -17.86006801910157193, 11.38285951858322242, 11.49999999999999645 ) ) ;
#27961 = ORGANIZATION ( 'NAUO-ORG3', 'UNSPECIFIED', 'UNSPECIFIED' ) ;
#27962 = VERTEX_POINT ( 'NONE', #62090 ) ;
#27963 = CARTESIAN_POINT ( 'NONE',  ( -2.513997614918375589, -22.02279109229760223, -1.500000000000002220 ) ) ;
#27964 = CARTESIAN_POINT ( 'NONE',  ( 19.85042311639309531, 5.490197614093233369, -1.500000000000002220 ) ) ;
#27965 = ORIENTED_EDGE ( 'NONE', *, *, #2489, .T. ) ;
#27967 = ORIENTED_EDGE ( 'NONE', *, *, #35921, .T. ) ;
#27966 = VECTOR ( 'NONE', #56632, 1000.000000000000114 ) ;
#27968 = LINE ( 'NONE', #66058, #80297 ) ;
#27969 = CARTESIAN_POINT ( 'NONE',  ( -77.58953762381673869, -23.47593901973091235, -1.443836447539004642 ) ) ;
#27970 = EDGE_LOOP ( 'NONE', ( #3260, #93929, #69890, #15993 ) ) ;
#27971 = ORIENTED_EDGE ( 'NONE', *, *, #89655, .T. ) ;
#27972 = ORIENTED_EDGE ( 'NONE', *, *, #85738, .T. ) ;
#27973 = AXIS2_PLACEMENT_3D ( 'NONE', #45220, #60949, #22349 ) ;
#27974 = CARTESIAN_POINT ( 'NONE',  ( -77.52287095715009002, -23.96177878511308990, 10.65340807706329684 ) ) ;
#27976 = CARTESIAN_POINT ( 'NONE',  ( -108.6228709571500417, -24.65952944569305316, 1.056160979905705011 ) ) ;
#27975 = B_SPLINE_CURVE_WITH_KNOTS ( 'NONE', 3,
 ( #3914, #58196, #19113, #43956 ),
 .UNSPECIFIED., .F., .F.,
 ( 4, 4 ),
 ( 0.5902073771187474893, 0.5992138083908630231 ),
 .UNSPECIFIED. ) ;
#27977 = DIRECTION ( 'NONE',  ( -3.773278334453080206E-23, 0.9999999999976377785, 2.173523156925979975E-06 ) ) ;
#27978 = CARTESIAN_POINT ( 'NONE',  ( -15.76495264167062160, -13.51897010167481739, -1.500000000000002220 ) ) ;
#27979 = CARTESIAN_POINT ( 'NONE',  ( 21.56942612084361599, 2.798134137018522427, 11.49999999999999645 ) ) ;
#27980 = VERTEX_POINT ( 'NONE', #23487 ) ;
#27981 = CARTESIAN_POINT ( 'NONE',  ( -40.45829750704998418, -25.18492896333868103, 3.293943116708551777 ) ) ;
#27982 = CARTESIAN_POINT ( 'NONE',  ( -37.58953762381673158, -24.66019654487199375, 8.947790411086137041 ) ) ;
#27983 = DIRECTION ( 'NONE',  ( -3.773278334453079618E-23, 0.9999999999976377785, 2.173523156925979975E-06 ) ) ;
#27984 = CARTESIAN_POINT ( 'NONE',  ( 15.48037617655995923, 16.25473645317415361, -1.500000000000002220 ) ) ;
#27985 = LINE ( 'NONE', #88388, #14101 ) ;
#27986 = CARTESIAN_POINT ( 'NONE',  ( -124.5228709571500332, -23.73934037231757443, 11.05740245334327732 ) ) ;
#27987 = ORIENTED_EDGE ( 'NONE', *, *, #23694, .T. ) ;
#27988 = DIRECTION ( 'NONE',  ( 0.000000000000000000, 2.173523156925979975E-06, -0.9999999999976378895 ) ) ;
#27989 = CARTESIAN_POINT ( 'NONE',  ( -89.67764846858844408, -25.05712135967895549, 7.447789548357304668 ) ) ;
#27990 = B_SPLINE_SURFACE_WITH_KNOTS ( 'NONE', 3, 3, ( 
 ( #22076, #20589, #30195, #82983 ),
 ( #51561, #22565, #99690, #6372 ),
 ( #37332, #76363, #44445, #29706 ),
 ( #91103, #92099, #53060, #52551 ),
 ( #90607, #82490, #83484, #12974 ),
 ( #28716, #44948, #29211, #43939 ),
 ( #74872, #14467, #36329, #59677 ),
 ( #67794, #84488, #13475, #98712 ),
 ( #75372, #45449, #5375, #67287 ),
 ( #6866, #61177, #60179, #21088 ) ),
 .UNSPECIFIED., .F., .F., .F.,
 ( 4, 3, 3, 4 ),
 ( 4, 4 ),
 ( 0.7022005934544807149, 0.7765311282028797280, 0.8508616629512786300, 0.9995227324480764342 ),
 ( 0.3995422158643850974, 0.4007930624188544289 ),
 .UNSPECIFIED. ) ;
#27991 = ORIENTED_EDGE ( 'NONE', *, *, #67338, .F. ) ;
#27992 = ORIENTED_EDGE ( 'NONE', *, *, #55449, .F. ) ;
#27993 = CARTESIAN_POINT ( 'NONE',  ( -87.62287095715004170, -23.47593901973091235, -1.443836447539002865 ) ) ;
#27994 = ORIENTED_EDGE ( 'NONE', *, *, #40262, .F. ) ;
#27995 = VECTOR ( 'NONE', #12902, 1000.000000000000227 ) ;
#27996 = EDGE_CURVE ( 'NONE', #28945, #50965, #63268, .T. ) ;
#27997 = CARTESIAN_POINT ( 'NONE',  ( -18.83571791729191958, -9.990160686573538840, -1.500000000000002220 ) ) ;
#27998 = ORIENTED_EDGE ( 'NONE', *, *, #17714, .F. ) ;
#27999 = CARTESIAN_POINT ( 'NONE',  ( -5.891025641025639636, -5.876774720514419847, 20.75510817307693046 ) ) ;
#28000 = CARTESIAN_POINT ( 'NONE',  ( 13.86046232669119149, 16.88393516940953276, -1.500000000000002220 ) ) ;
#28001 = CARTESIAN_POINT ( 'NONE',  ( -55.55620429048340014, -23.47596703998600276, 11.44779298504227505 ) ) ;
#28002 = CARTESIAN_POINT ( 'NONE',  ( 17.32531159343115945, 14.66459048539768162, -1.500000000000002220 ) ) ;
#28003 = CARTESIAN_POINT ( 'NONE',  ( -40.93315603532715130, -25.18430893389220060, 3.395436753013815423 ) ) ;
#28004 = CARTESIAN_POINT ( 'NONE',  ( -124.5228709571500616, -23.47593901973090524, -1.443836447538996204 ) ) ;
#28005 = CARTESIAN_POINT ( 'NONE',  ( -20.07106029494397248, -8.819774368769808248, -1.500000000000002220 ) ) ;
#28006 = CARTESIAN_POINT ( 'NONE',  ( -109.5228709571500474, -24.66019654487200086, 8.947790411086119278 ) ) ;
#28007 = VERTEX_POINT ( 'NONE', #30118 ) ;
#28008 = CARTESIAN_POINT ( 'NONE',  ( -122.5195445546590918, -24.35071581493544102, 9.817618358456019934 ) ) ;
#28009 = DIRECTION ( 'NONE',  ( -0.000000000000000000, -1.000000000000000000, -0.000000000000000000 ) ) ;
#28010 = AXIS2_PLACEMENT_3D ( 'NONE', #46427, #7860, #23572 ) ;
#28011 = EDGE_CURVE ( 'NONE', #70502, #94742, #61091, .T. ) ;
#28012 = EDGE_CURVE ( 'NONE', #53932, #98229, #49783, .T. ) ;
#28013 = ORIENTED_EDGE ( 'NONE', *, *, #3162, .T. ) ;
#28014 = EDGE_CURVE ( 'NONE', #23237, #11869, #44868, .T. ) ;
#28015 = CARTESIAN_POINT ( 'NONE',  ( -30.61237075433887966, -24.38737281877371643, 9.682478639550817334 ) ) ;
#28016 = CIRCLE ( 'NONE', #55545, 1.249999999999997558 ) ;
#28017 = DIRECTION ( 'NONE',  ( -0.000000000000000000, 1.000000000000000000, -0.000000000000000000 ) ) ;
#28018 = EDGE_CURVE ( 'NONE', #78621, #871, #48109, .T. ) ;
#28019 = CARTESIAN_POINT ( 'NONE',  ( -27.25988310792305214, 0.3587747205144265483, 30.32664379231667695 ) ) ;
#28020 = CARTESIAN_POINT ( 'NONE',  ( 16.87399902462237478, -12.92443306546820736, 11.49999999999998934 ) ) ;
#28021 = CARTESIAN_POINT ( 'NONE',  ( -110.5228709571500616, -29.50250786944525672, 11.44777988621622988 ) ) ;
#28022 = LINE ( 'NONE', #50368, #93449 ) ;
#28023 = CARTESIAN_POINT ( 'NONE',  ( -114.5228709571500616, -23.48783264083396105, -1.443836473375806895 ) ) ;
#28024 = FACE_OUTER_BOUND ( 'NONE', #79225, .T. ) ;
#28025 = DIRECTION ( 'NONE',  ( 0.000000000000000000, 0.000000000000000000, 1.000000000000000000 ) ) ;
#28026 = ORIENTED_EDGE ( 'NONE', *, *, #66322, .T. ) ;
#28027 = CARTESIAN_POINT ( 'NONE',  ( -19.49195742049215241, -1.735909528584683947, 11.49999999999999645 ) ) ;
#28028 = CARTESIAN_POINT ( 'NONE',  ( -78.52287095715006160, -23.73934037231757088, 11.05740245334328975 ) ) ;
#28029 = CARTESIAN_POINT ( 'NONE',  ( -28.16520605572959468, -24.69042538764675143, 8.198497088267734156 ) ) ;
#28030 = EDGE_CURVE ( 'NONE', #7941, #58804, #672, .T. ) ;
#28031 = ORIENTED_EDGE ( 'NONE', *, *, #2432, .F. ) ;
#28032 = CARTESIAN_POINT ( 'NONE',  ( 3.879810481058463711, -6.376774720514427841, 21.83835767234735670 ) ) ;
#28033 = CARTESIAN_POINT ( 'NONE',  ( -44.55620429048338593, -24.65952944569303895, 1.056160979905692576 ) ) ;
#28034 = LINE ( 'NONE', #67112, #61784 ) ;
#28035 = AXIS2_PLACEMENT_3D ( 'NONE', #2722, #26040, #80330 ) ;
#28036 = CARTESIAN_POINT ( 'NONE',  ( -41.62287095715006302, -24.64898659630367561, 1.056161002820819261 ) ) ;
#28038 = EDGE_CURVE ( 'NONE', #6656, #2820, #86251, .T. ) ;
#28037 = CARTESIAN_POINT ( 'NONE',  ( 17.66836560233463516, 8.693963128369697202, 11.49999999999998934 ) ) ;
#28040 = ORIENTED_EDGE ( 'NONE', *, *, #24130, .F. ) ;
#28039 = LOCAL_TIME ( 0, 54, 15.00000000000000000, #93684 ) ;
#28041 = DIRECTION ( 'NONE',  ( -3.773278334453079618E-23, 0.9999999999976377785, 2.173523156925979975E-06 ) ) ;
#28042 = CARTESIAN_POINT ( 'NONE',  ( 30.61643171304413613, -3.316774720514426456, 27.37433008668288181 ) ) ;
#28043 = EDGE_CURVE ( 'NONE', #2872, #62364, #91097, .T. ) ;
#28044 = AXIS2_PLACEMENT_3D ( 'NONE', #26801, #88707, #43532 ) ;
#28045 = COORDINATED_UNIVERSAL_TIME_OFFSET ( 0, 0, .AHEAD. ) ;
#28046 = VERTEX_POINT ( 'NONE', #79793 ) ;
#28047 = DIRECTION ( 'NONE',  ( -3.773278334453079618E-23, 0.9999999999976377785, 2.173523156925979975E-06 ) ) ;
#28048 = DIRECTION ( 'NONE',  ( -0.09721092304694055330, 0.000000000000000000, 0.9952638024365006997 ) ) ;
#28049 = CARTESIAN_POINT ( 'NONE',  ( -47.62840667103132830, -24.51314013834316086, 0.6176544820404172853 ) ) ;
#28050 = CARTESIAN_POINT ( 'NONE',  ( -118.5222382821682174, -23.48783264082477018, -1.443836473390085695 ) ) ;
#28051 = CARTESIAN_POINT ( 'NONE',  ( -49.58953762381672448, -24.64965694238575011, 8.947790433994205372 ) ) ;
#28052 = CARTESIAN_POINT ( 'NONE',  ( -70.32437837831572836, -25.24515042352634708, 5.314180867886988402 ) ) ;
#28053 = VECTOR ( 'NONE', #83660, 1000.000000000000114 ) ;
#28054 = CARTESIAN_POINT ( 'NONE',  ( -85.52287095715004739, -25.00158670708909625, 2.256160236439166411 ) ) ;
#28055 = CARTESIAN_POINT ( 'NONE',  ( 4.608267332293128682, -19.41724391825443874, -1.500000000000002220 ) ) ;
#28056 = LINE ( 'NONE', #36167, #46752 ) ;
#28057 = CARTESIAN_POINT ( 'NONE',  ( -0.08004075721539863353, -22.01380949857533409, 0.03441076822783003392 ) ) ;
#28058 = ORIENTED_EDGE ( 'NONE', *, *, #35675, .T. ) ;
#28059 = CARTESIAN_POINT ( 'NONE',  ( -116.5562042904833788, -23.47596703998600631, 11.44779298504227683 ) ) ;
#28060 = DIRECTION ( 'NONE',  ( 0.1478094111296165969, -0.9890158633619159367, 0.000000000000000000 ) ) ;
#28061 = B_SPLINE_CURVE_WITH_KNOTS ( 'NONE', 3,
 ( #60359, #22253, #36999, #67963, #98890, #29383 ),
 .UNSPECIFIED., .F., .F.,
 ( 4, 2, 4 ),
 ( 0.000000000000000000, 0.001380764517854764315, 0.002761529035709528630 ),
 .UNSPECIFIED. ) ;
#28062 = EDGE_CURVE ( 'NONE', #40153, #26363, #72201, .T. ) ;
#28063 =( NAMED_UNIT ( * ) SI_UNIT ( $, .STERADIAN. ) SOLID_ANGLE_UNIT ( ) );
#28064 = CARTESIAN_POINT ( 'NONE',  ( 12.98941176919429097, -3.316774720517114972, -28.15829778459866262 ) ) ;
#28065 = DIRECTION ( 'NONE',  ( 0.000000000000000000, 0.9999999999976377785, 2.173523156925979975E-06 ) ) ;
#28066 = DIRECTION ( 'NONE',  ( 3.773278334444167608E-23, -1.000000000000000000, 0.000000000000000000 ) ) ;
#28067 = EDGE_CURVE ( 'NONE', #66329, #34477, #9189, .T. ) ;
#28068 = CARTESIAN_POINT ( 'NONE',  ( -26.50076437627408765, -24.83282267876757743, 2.987432207970394327 ) ) ;
#28069 = DIRECTION ( 'NONE',  ( 0.000000000000000000, 1.000000000000000000, 0.000000000000000000 ) ) ;
#28070 = EDGE_LOOP ( 'NONE', ( #9097, #29251, #96618, #46957 ) ) ;
#28071 = B_SPLINE_SURFACE_WITH_KNOTS ( 'NONE', 3, 1, ( 
 ( #76356, #67281 ),
 ( #98199, #81993 ),
 ( #59670, #43446 ),
 ( #90600, #52046 ),
 ( #36820, #21571 ),
 ( #97218, #12477 ),
 ( #74376, #35821 ),
 ( #31186, #39804 ),
 ( #14962, #46923 ),
 ( #7347, #46421 ),
 ( #47427, #22559 ),
 ( #70259, #54050 ),
 ( #24571, #23062 ),
 ( #93082, #55548 ),
 ( #38302, #16964 ),
 ( #63159, #30188 ),
 ( #99684, #31695 ),
 ( #77352, #93578 ),
 ( #7854, #39303 ) ),
 .UNSPECIFIED., .F., .F., .F.,
 ( 4, 1, 1, 1, 1, 1, 1, 1, 1, 1, 1, 1, 1, 1, 1, 1, 4 ),
 ( 2, 2 ),
 ( 0.000000000000000000, 0.06523080374203335530, 0.1284048960032229403, 0.1900670715964798418, 0.2509433657682823560, 0.3115458328521446552, 0.3728628021568331508, 0.4350236738562400229, 0.4990717247070452500, 0.5630910750496653794, 0.6255101063303781794, 0.6866800359296505452, 0.7472825030135124003, 0.8085634952159601596, 0.8707421035159864653, 0.9343409515059127868, 1.000000000000000000 ),
 ( 0.000000000000000000, 1.000000000000000000 ),
 .UNSPECIFIED. ) ;
#28072 = DIRECTION ( 'NONE',  ( -0.000000000000000000, 2.173523156925979552E-06, -0.9999999999976378895 ) ) ;
#28073 = CARTESIAN_POINT ( 'NONE',  ( -127.6242800499748853, -23.96119346886880663, -0.6495511937832001426 ) ) ;
#28074 = ORIENTED_EDGE ( 'NONE', *, *, #9626, .F. ) ;
#28075 = CARTESIAN_POINT ( 'NONE',  ( 16.63042848490962555, -11.55671354112608817, 11.49999999999998934 ) ) ;
#28076 = CARTESIAN_POINT ( 'NONE',  ( -68.93918693012690824, -25.25799956426409665, 6.184868438663939649 ) ) ;
#28077 = DIRECTION ( 'NONE',  ( -1.000000000000000000, -3.773278334444166432E-23, -8.201307841325785021E-29 ) ) ;
#28078 = CIRCLE ( 'NONE', #55615, 0.3000000000000016542 ) ;
#28079 = CARTESIAN_POINT ( 'NONE',  ( 22.65031661608460922, 2.682774720514426559, -20.71116937900381672 ) ) ;
#28080 = ORIENTED_EDGE ( 'NONE', *, *, #63033, .T. ) ;
#28081 = CARTESIAN_POINT ( 'NONE',  ( -78.94968344233984681, -25.29062087922736524, 5.787134492223548143 ) ) ;
#28082 = CARTESIAN_POINT ( 'NONE',  ( -52.52287095715006870, -23.48786465467241058, 11.44779295918255002 ) ) ;
#28083 = CARTESIAN_POINT ( 'NONE',  ( 4.692034869050136336, 19.47840706813412126, -1.500000000000002220 ) ) ;
#28084 = AXIS2_PLACEMENT_3D ( 'NONE', #29294, #92681, #37910 ) ;
#28085 = CARTESIAN_POINT ( 'NONE',  ( 18.24537196375281312, 10.48796402029766739, 11.49999999999999645 ) ) ;
#28086 = FACE_OUTER_BOUND ( 'NONE', #54950, .T. ) ;
#28087 = CARTESIAN_POINT ( 'NONE',  ( -89.81226385320383088, -25.31788500672307052, 4.644766330052804371 ) ) ;
#28088 = CARTESIAN_POINT ( 'NONE',  ( -2.767897998228395551, 21.91458177938747909, -1.500000000000002220 ) ) ;
#28089 = CARTESIAN_POINT ( 'NONE',  ( -40.02212956655154130, -25.27806092693242945, 5.017934196670617020 ) ) ;
#28090 = CARTESIAN_POINT ( 'NONE',  ( -76.55620429048340725, -23.47593901973091235, -1.443836447539004642 ) ) ;
#28091 = CARTESIAN_POINT ( 'NONE',  ( 30.61643171304413613, -3.316774720514426456, 27.37433008668288181 ) ) ;
#28092 = ORIENTED_EDGE ( 'NONE', *, *, #68009, .T. ) ;
#28093 = CARTESIAN_POINT ( 'NONE',  ( -99.17126091090496232, -25.24403727686683396, 3.682577372028675633 ) ) ;
#28094 = CARTESIAN_POINT ( 'NONE',  ( -31.61989000895333746, -23.48783264082477018, -1.443836473390079256 ) ) ;
#28095 = EDGE_LOOP ( 'NONE', ( #54788, #68274, #54726, #59953 ) ) ;
#28096 = VERTEX_POINT ( 'NONE', #72703 ) ;
#28097 = CARTESIAN_POINT ( 'NONE',  ( -80.64675904551151575, -25.20074414427590881, 3.409327697718777195 ) ) ;
#28098 = FACE_OUTER_BOUND ( 'NONE', #89959, .T. ) ;
#28099 = DIRECTION ( 'NONE',  ( 0.000000000000000000, 0.9999999999976377785, 2.173523156925979128E-06 ) ) ;
#28100 = CARTESIAN_POINT ( 'NONE',  ( -14.18348626307465743, -14.89297910716571849, -1.500000000000002220 ) ) ;
#28101 = CARTESIAN_POINT ( 'NONE',  ( -17.67581969798968444, -12.36387604476075097, 11.49999999999999645 ) ) ;
#28102 = ORIENTED_EDGE ( 'NONE', *, *, #29511, .F. ) ;
#28103 = CARTESIAN_POINT ( 'NONE',  ( -91.51836583836262662, -23.73766607897670156, -1.055555164236454235 ) ) ;
#28104 = LINE ( 'NONE', #43336, #17469 ) ;
#28105 = LINE ( 'NONE', #90495, #72331 ) ;
#28106 = CARTESIAN_POINT ( 'NONE',  ( 9.556255610625576935, 20.19728179944524271, -1.500000000000002220 ) ) ;
#28108 = CARTESIAN_POINT ( 'NONE',  ( 29.71896661235086157, -4.666145129001815661, 27.69970538640514235 ) ) ;
#28107 = VECTOR ( 'NONE', #71878, 1000.000000000000000 ) ;
#28109 = CARTESIAN_POINT ( 'NONE',  ( -98.52287095715006160, -24.64898659630368272, 1.056161002820829697 ) ) ;
#28110 = ORIENTED_EDGE ( 'NONE', *, *, #74440, .F. ) ;
#28111 = DIRECTION ( 'NONE',  ( -0.9496245541219264785, -6.845827386180410961E-16, -0.3133898629642195011 ) ) ;
#28112 = CARTESIAN_POINT ( 'NONE',  ( -51.13317816230360791, -25.30518297057644617, 4.892016129566734151 ) ) ;
#28113 = CARTESIAN_POINT ( 'NONE',  ( -0.8937202392249329330, 20.86669477224961256, 11.49999999999998934 ) ) ;
#28114 = EDGE_LOOP ( 'NONE', ( #31372, #90011, #28140, #46556 ) ) ;
#28116 = EDGE_LOOP ( 'NONE', ( #10534, #21229, #25629, #87361 ) ) ;
#28115 = CARTESIAN_POINT ( 'NONE',  ( -92.52287095715006160, -24.65952944569304606, 1.056160979905700570 ) ) ;
#28117 = VERTEX_POINT ( 'NONE', #16389 ) ;
#28118 = AXIS2_PLACEMENT_3D ( 'NONE', #95070, #17439, #41284 ) ;
#28119 = CARTESIAN_POINT ( 'NONE',  ( -100.6266774032520601, -24.73531770709095312, 8.716586749053508498 ) ) ;
#28120 = CARTESIAN_POINT ( 'NONE',  ( 13.25904570721172604, 16.46799385432867169, -1.500000000000002220 ) ) ;
#28121 = ORIENTED_EDGE ( 'NONE', *, *, #92979, .T. ) ;
#28122 = CARTESIAN_POINT ( 'NONE',  ( -91.58953762381672448, -24.66019654487198665, 8.947790411086135265 ) ) ;
#28124 = EDGE_CURVE ( 'NONE', #28719, #85754, #93608, .T. ) ;
#28123 = CARTESIAN_POINT ( 'NONE',  ( -102.6228709571500559, -23.47596703998600631, 11.44779298504227683 ) ) ;
#28125 = CARTESIAN_POINT ( 'NONE',  ( -120.5579446662922862, -23.48786465467241769, 11.44779295918253936 ) ) ;
#28126 = VECTOR ( 'NONE', #45737, 1000.000000000000114 ) ;
#28127 = EDGE_CURVE ( 'NONE', #75293, #87052, #2690, .T. ) ;
#28128 = LINE ( 'NONE', #97624, #51812 ) ;
#28129 = CARTESIAN_POINT ( 'NONE',  ( 7.311104923646705167, -6.376774720514415407, 20.13320233724603980 ) ) ;
#28130 = CARTESIAN_POINT ( 'NONE',  ( -4.706806674773570620, -21.25045708977441450, -1.500000000000002220 ) ) ;
#28131 = CARTESIAN_POINT ( 'NONE',  ( -81.14265914342044539, -25.12224344358931205, 6.882252752011148722 ) ) ;
#28133 = ORIENTED_EDGE ( 'NONE', *, *, #70652, .F. ) ;
#28132 = CARTESIAN_POINT ( 'NONE',  ( 22.30035941410032763, -0.3387204123245128873, 11.49999999999999645 ) ) ;
#28134 = CARTESIAN_POINT ( 'NONE',  ( -45.62287095715005592, -24.52232992886361984, 0.6492154411906032596 ) ) ;
#28135 = CARTESIAN_POINT ( 'NONE',  ( -110.3139465455115271, -25.12049752546738191, 2.832404795212222659 ) ) ;
#28136 = FACE_OUTER_BOUND ( 'NONE', #99481, .T. ) ;
#28137 = ORIENTED_EDGE ( 'NONE', *, *, #17690, .T. ) ;
#28138 = ADVANCED_FACE ( 'NONE', ( #70688 ), #26409, .T. ) ;
#28139 = EDGE_CURVE ( 'NONE', #46936, #47734, #67586, .T. ) ;
#28140 = ORIENTED_EDGE ( 'NONE', *, *, #66541, .F. ) ;
#28141 = ORIENTED_EDGE ( 'NONE', *, *, #40966, .F. ) ;
#28142 = DIRECTION ( 'NONE',  ( 0.000000000000000000, 0.000000000000000000, 1.000000000000000000 ) ) ;
#28143 = FACE_OUTER_BOUND ( 'NONE', #53972, .T. ) ;
#28144 = CARTESIAN_POINT ( 'NONE',  ( 29.73620800866979863, -5.101103159685075106, 27.18593991345460381 ) ) ;
#28145 = LINE ( 'NONE', #44872, #84239 ) ;
#28146 = CARTESIAN_POINT ( 'NONE',  ( -76.52287095715007581, -24.64898659630528854, 1.056161002820826145 ) ) ;
#28147 = ADVANCED_FACE ( 'NONE', ( #17906 ), #48866, .F. ) ;
#28148 = DIRECTION ( 'NONE',  ( -1.000000000000000000, -3.773278334444167608E-23, -8.201307833595939069E-29 ) ) ;
#28149 = ORIENTED_EDGE ( 'NONE', *, *, #37785, .F. ) ;
#28150 = CARTESIAN_POINT ( 'NONE',  ( 17.07123823605233781, 9.195568589125342029, 11.49999999999999645 ) ) ;
#28151 = CARTESIAN_POINT ( 'NONE',  ( -115.5228709571500758, -25.00182538069145721, 7.747789668545101094 ) ) ;
#28152 = VERTEX_POINT ( 'NONE', #35137 ) ;
#28154 = CARTESIAN_POINT ( 'NONE',  ( 3.248328688408994580, -6.376774720514406525, 18.75910638930973917 ) ) ;
#28153 = VECTOR ( 'NONE', #89772, 1000.000000000000000 ) ;
#28155 = CARTESIAN_POINT ( 'NONE',  ( 5.659515148826130826, 3.316774720513238517, -27.47062408975114067 ) ) ;
#28156 = CARTESIAN_POINT ( 'NONE',  ( -111.7814946224345789, -29.50249240399202222, 4.332395270848422797 ) ) ;
#28157 = DIRECTION ( 'NONE',  ( -1.000000000000000000, 0.000000000000000000, 0.000000000000000000 ) ) ;
#28158 = CARTESIAN_POINT ( 'NONE',  ( 13.97609912898263573, 13.72534901313461653, -1.500000000000002220 ) ) ;
#28159 = VECTOR ( 'NONE', #62348, 1000.000000000000114 ) ;
#28160 = LINE ( 'NONE', #83424, #7219 ) ;
#28161 = ORIENTED_EDGE ( 'NONE', *, *, #15046, .T. ) ;
#28162 = CARTESIAN_POINT ( 'NONE',  ( 16.61460563260716583, 13.71664681387569118, 11.49999999999998934 ) ) ;
#28163 = CARTESIAN_POINT ( 'NONE',  ( -33.58056022833496712, -24.51419770103157347, 9.386484678747185839 ) ) ;
#28164 = CARTESIAN_POINT ( 'NONE',  ( -123.6228709571500559, -23.48786465467241769, 11.44779295918253759 ) ) ;
#28165 = CARTESIAN_POINT ( 'NONE',  ( -72.62287095715005592, -24.66019654487199020, 8.947790411086131712 ) ) ;
#28166 = CARTESIAN_POINT ( 'NONE',  ( -100.4326965455115044, -25.27473221600376618, 3.293942921519102729 ) ) ;
#28167 = CARTESIAN_POINT ( 'NONE',  ( 8.869223403490039459, -21.23658630136709391, -1.500000000000002220 ) ) ;
#28168 = APPROVAL_DATE_TIME ( #21036, #488 ) ;
#28169 = DIRECTION ( 'NONE',  ( 1.000000000000000000, -0.000000000000000000, -0.000000000000000000 ) ) ;
#28170 = CARTESIAN_POINT ( 'NONE',  ( -53.58246871847038051, -24.51314013834315730, 0.6176544820404108460 ) ) ;
#28171 = CARTESIAN_POINT ( 'NONE',  ( -20.16912494768211417, -0.3064379698199363733, 11.49999999999999645 ) ) ;
#28172 = DIRECTION ( 'NONE',  ( -0.000000000000000000, 1.000000000000000000, -0.000000000000000000 ) ) ;
#28173 = CARTESIAN_POINT ( 'NONE',  ( 0.8635838190919263857, -3.990505948720460605, -8.999999999999998224 ) ) ;
#28174 = DIRECTION ( 'NONE',  ( 0.7071067811865476838, 0.000000000000000000, -0.7071067811865474617 ) ) ;
#28175 = CARTESIAN_POINT ( 'NONE',  ( 13.86067930680220073, 3.316774720515830666, -28.23766061184437604 ) ) ;
#28176 = CARTESIAN_POINT ( 'NONE',  ( -122.5228709571500616, -23.48786465467241769, 11.44779295918253759 ) ) ;
#28177 = CARTESIAN_POINT ( 'NONE',  ( 15.03354914759215966, -12.96403794047452607, -1.500000000000002220 ) ) ;
#28178 = VECTOR ( 'NONE', #89117, 1000.000000000000114 ) ;
#28179 = CARTESIAN_POINT ( 'NONE',  ( -109.5895376238167387, -24.64898659630368627, 1.056161002820390049 ) ) ;
#28180 = CARTESIAN_POINT ( 'NONE',  ( 14.33573519231038063, 13.56928687979844561, -1.500000000000002220 ) ) ;
#28181 = CARTESIAN_POINT ( 'NONE',  ( -42.58143151915821534, -24.51314013834315375, 0.6176544820404090697 ) ) ;
#28182 = ADVANCED_FACE ( 'NONE', ( #20381 ), #98002, .T. ) ;
#28183 = CARTESIAN_POINT ( 'NONE',  ( -110.5228709571500616, -24.51254535375845123, 9.355368624242252906 ) ) ;
#28184 = DIRECTION ( 'NONE',  ( -0.5656310827093757876, -0.8246584009594636333, -1.161164194647626387E-16 ) ) ;
#28185 = CARTESIAN_POINT ( 'NONE',  ( -15.52656095410427817, -13.64048245868121434, 11.49999999999999645 ) ) ;
#28186 = CARTESIAN_POINT ( 'NONE',  ( 7.107139210497321002, -6.376774720514413630, 19.78447747620696617 ) ) ;
#28187 = EDGE_CURVE ( 'NONE', #26613, #32255, #88923, .T. ) ;
#28188 = DIRECTION ( 'NONE',  ( 0.9888510809027409865, -7.885106708985486076E-16, 0.1489078231574183231 ) ) ;
#28189 = CARTESIAN_POINT ( 'NONE',  ( -12.60694655700363143, 18.86142483545513926, 11.49999999999999645 ) ) ;
#28190 = VERTEX_POINT ( 'NONE', #89416 ) ;
#28191 = CARTESIAN_POINT ( 'NONE',  ( -5.366453405989236813, 0.000000000000000000, 0.000000000000000000 ) ) ;
#28192 = CARTESIAN_POINT ( 'NONE',  ( 30.63935204725980554, 3.888906929512149446, 28.25823861891851507 ) ) ;
#28193 = AXIS2_PLACEMENT_3D ( 'NONE', #14665, #82181, #12667 ) ;
#28194 = CARTESIAN_POINT ( 'NONE',  ( -60.58953762381671737, -23.47593901973091235, -1.443836447539007972 ) ) ;
#28195 = CARTESIAN_POINT ( 'NONE',  ( -36.62287095715005592, -23.48783264082477729, -1.443836473390072372 ) ) ;
#28196 = ORIENTED_EDGE ( 'NONE', *, *, #65545, .F. ) ;
#28197 = ORIENTED_EDGE ( 'NONE', *, *, #53856, .F. ) ;
#28198 = CARTESIAN_POINT ( 'NONE',  ( 0.3906119451836247425, -6.376774720514418959, 20.56083401959467594 ) ) ;
#28199 = CARTESIAN_POINT ( 'NONE',  ( 17.53461989915211916, -14.66684187699354425, 11.49999999999998934 ) ) ;
#28200 = CARTESIAN_POINT ( 'NONE',  ( -29.60196703136402263, -23.88187520205043057, -0.6495508823503304274 ) ) ;
#28201 = CARTESIAN_POINT ( 'NONE',  ( -20.03152041342270806, -8.007337437543776915, -1.500000000000002220 ) ) ;
#28202 = CARTESIAN_POINT ( 'NONE',  ( -113.5892018432855650, -24.35071581493543746, 9.817618358456018157 ) ) ;
#28203 = FACE_OUTER_BOUND ( 'NONE', #24338, .T. ) ;
#28204 = CARTESIAN_POINT ( 'NONE',  ( 22.10748686624256720, -4.471405416651531795, 11.49999999999999645 ) ) ;
#28205 = EDGE_LOOP ( 'NONE', ( #39870, #47853, #66145, #100356, #22104, #10704, #18570, #78026, #93220, #66179 ) ) ;
#28206 = PLANE ( 'NONE',  #62695 ) ;
#28207 = CARTESIAN_POINT ( 'NONE',  ( 19.92286461850947887, -9.344431347164146473, 11.49999999999998934 ) ) ;
#28208 = CARTESIAN_POINT ( 'NONE',  ( -44.60757519715500052, -23.73791477778911130, 11.05961554403170943 ) ) ;
#28209 = CARTESIAN_POINT ( 'NONE',  ( -28.94649234366282187, -25.21724812713350872, 6.769412627959744633 ) ) ;
#28210 = ORIENTED_EDGE ( 'NONE', *, *, #69193, .F. ) ;
#28211 = DIRECTION ( 'NONE',  ( -3.773278334453079618E-23, 0.9999999999976377785, 2.173523156925979975E-06 ) ) ;
#28212 = DIRECTION ( 'NONE',  ( 0.000000000000000000, -0.9999999999976377785, -2.173523156925979128E-06 ) ) ;
#28213 = VERTEX_POINT ( 'NONE', #19393 ) ;
#28214 = CARTESIAN_POINT ( 'NONE',  ( -108.5228709571500758, -23.47593901973090524, -1.443836447538996204 ) ) ;
#28215 = ORIENTED_EDGE ( 'NONE', *, *, #15668, .F. ) ;
#28216 = VERTEX_POINT ( 'NONE', #28506 ) ;
#28217 = DIRECTION ( 'NONE',  ( 1.000000000000000000, 0.000000000000000000, 0.000000000000000000 ) ) ;
#28218 = CARTESIAN_POINT ( 'NONE',  ( -104.5228709571500758, -24.65952944569305316, 1.056160979905702346 ) ) ;
#28219 = DIRECTION ( 'NONE',  ( -0.000000000000000000, 1.000000000000000000, -0.000000000000000000 ) ) ;
#28220 = CARTESIAN_POINT ( 'NONE',  ( 8.094744887094867281, -18.73235182305680624, -1.500000000000002220 ) ) ;
#28221 = AXIS2_PLACEMENT_3D ( 'NONE', #96021, #4178, #97018 ) ;
#28222 = ORIENTED_EDGE ( 'NONE', *, *, #2856, .T. ) ;
#28223 = CARTESIAN_POINT ( 'NONE',  ( 2.246611357655420083, 0.1632191352058117717, -0.1632191352058112166 ) ) ;
#28224 = CARTESIAN_POINT ( 'NONE',  ( -30.56674980027052513, -25.57033040079278052, 6.142048374048878046 ) ) ;
#28225 = ADVANCED_FACE ( 'NONE', ( #73689, #67097, #34636 ), #11019, .T. ) ;
#28226 = DIRECTION ( 'NONE',  ( -0.000000000000000000, -1.000000000000000000, 0.000000000000000000 ) ) ;
#28227 = CARTESIAN_POINT ( 'NONE',  ( -71.60924725748338915, -25.03149666953593666, 6.721928064598928110 ) ) ;
#28228 = EDGE_LOOP ( 'NONE', ( #59698, #41711, #86905, #74896 ) ) ;
#28229 = CARTESIAN_POINT ( 'NONE',  ( -99.92287095715006728, -23.47596703998600631, 11.44779298504227860 ) ) ;
#28231 = VECTOR ( 'NONE', #46300, 1000.000000000000000 ) ;
#28230 = DIRECTION ( 'NONE',  ( -0.000000000000000000, 2.173523156925979552E-06, -0.9999999999976378895 ) ) ;
#28232 = ORIENTED_EDGE ( 'NONE', *, *, #25163, .T. ) ;
#28233 = CARTESIAN_POINT ( 'NONE',  ( -3.686900873480770002, -20.48319827837541141, -1.500000000000002220 ) ) ;
#28234 = ORIENTED_EDGE ( 'NONE', *, *, #99387, .T. ) ;
#28236 = ORIENTED_EDGE ( 'NONE', *, *, #75095, .F. ) ;
#28235 = FACE_OUTER_BOUND ( 'NONE', #54186, .T. ) ;
#28237 = CARTESIAN_POINT ( 'NONE',  ( -28.62287095715004881, -24.49675894734168580, 8.947790415257339092 ) ) ;
#28238 = CARTESIAN_POINT ( 'NONE',  ( -115.5228709571500616, -24.14321612903115977, -0.2833117244521543565 ) ) ;
#28239 = ORIENTED_EDGE ( 'NONE', *, *, #81187, .F. ) ;
#28240 = ORIENTED_EDGE ( 'NONE', *, *, #18792, .F. ) ;
#28241 = DIRECTION ( 'NONE',  ( -1.000000000000000000, -0.000000000000000000, -0.000000000000000000 ) ) ;
#28242 = EDGE_CURVE ( 'NONE', #51651, #44226, #68573, .T. ) ;
#28243 = LINE ( 'NONE', #59204, #98302 ) ;
#28244 = LINE ( 'NONE', #59205, #8059 ) ;
#28245 = CARTESIAN_POINT ( 'NONE',  ( -74.62287095715004170, -23.72747288104469376, -1.053458166803227014 ) ) ;
#28247 = ORIENTED_EDGE ( 'NONE', *, *, #24002, .T. ) ;
#28246 = CARTESIAN_POINT ( 'NONE',  ( -19.88706384024380824, 9.709922325909349894, 11.49999999999999645 ) ) ;
#28248 = CARTESIAN_POINT ( 'NONE',  ( -108.5492820750298790, -24.65952944569305316, 1.056160979905706121 ) ) ;
#28249 = EDGE_CURVE ( 'NONE', #50681, #22596, #6008, .T. ) ;
#28250 = CARTESIAN_POINT ( 'NONE',  ( 3.115699594417459473, -22.39947108414558485, -1.500000000000002220 ) ) ;
#28251 = ADVANCED_FACE ( 'NONE', ( #46739 ), #555, .T. ) ;
#28252 = B_SPLINE_CURVE_WITH_KNOTS ( 'NONE', 3,
 ( #29171, #68243, #100151, #21052, #67756, #23031 ),
 .UNSPECIFIED., .F., .F.,
 ( 4, 2, 4 ),
 ( 6.384118694777179670E-06, 0.001386860460836454026, 0.002767336802978130617 ),
 .UNSPECIFIED. ) ;
#28254 = VERTEX_POINT ( 'NONE', #44742 ) ;
#28253 = CARTESIAN_POINT ( 'NONE',  ( -99.42106458011447501, -25.30551355002305769, 5.055668188524513162 ) ) ;
#28255 = EDGE_CURVE ( 'NONE', #37811, #15171, #36644, .T. ) ;
#28256 = ORIENTED_EDGE ( 'NONE', *, *, #58106, .T. ) ;
#28257 = EDGE_CURVE ( 'NONE', #10246, #58683, #78849, .T. ) ;
#28258 = DIRECTION ( 'NONE',  ( -3.773278334453079618E-23, 0.9999999999976377785, 2.173523156925979975E-06 ) ) ;
#28259 = B_SPLINE_SURFACE_WITH_KNOTS ( 'NONE', 3, 3, ( 
 ( #36336, #12982, #22083, #52559 ),
 ( #6380, #43947, #83493, #59684 ),
 ( #21095, #74879, #99213, #61680 ),
 ( #93097, #78368, #15971, #85995 ),
 ( #40326, #70277, #7868, #99698 ),
 ( #92597, #63174, #8871, #7363 ),
 ( #94100, #16469, #93594, #257 ) ),
 .UNSPECIFIED., .F., .F., .F.,
 ( 4, 3, 4 ),
 ( 4, 4 ),
 ( 0.0004766839783816336743, 0.1029713700210892480, 0.2054660560637968647 ),
 ( 0.9397330492811201141, 0.9411793649393953576 ),
 .UNSPECIFIED. ) ;
#28260 = DIRECTION ( 'NONE',  ( -0.000000000000000000, 1.000000000000000000, -0.000000000000000000 ) ) ;
#28261 = ORIENTED_EDGE ( 'NONE', *, *, #13018, .T. ) ;
#28262 = DIRECTION ( 'NONE',  ( 1.000000000000000000, 0.000000000000000000, 0.000000000000000000 ) ) ;
#28263 = CARTESIAN_POINT ( 'NONE',  ( 20.12748746789148413, 9.599020362109589755, -1.500000000000002220 ) ) ;
#28264 = CARTESIAN_POINT ( 'NONE',  ( -46.62287095715004170, -24.50216790748097395, 0.6166512839513648148 ) ) ;
#28265 = EDGE_CURVE ( 'NONE', #52247, #86024, #5195, .T. ) ;
#28266 = EDGE_LOOP ( 'NONE', ( #25872, #66319, #31969, #58648 ) ) ;
#28267 = DIRECTION ( 'NONE',  ( -3.773278334453080206E-23, 0.9999999999976377785, 2.173523156925979975E-06 ) ) ;
#28268 = DIRECTION ( 'NONE',  ( 0.000000000000000000, -2.173523156925979552E-06, 0.9999999999976378895 ) ) ;
#28269 = DIRECTION ( 'NONE',  ( -0.7512896232465892110, 0.000000000000000000, -0.6599726524652350657 ) ) ;
#28270 = CARTESIAN_POINT ( 'NONE',  ( 33.96422015159436114, 0.3587747205144265483, -7.233236000911337449 ) ) ;
#28271 = CARTESIAN_POINT ( 'NONE',  ( -15.27948257512286645, 12.15582775940324822, -1.500000000000002220 ) ) ;
#28272 = CARTESIAN_POINT ( 'NONE',  ( 20.52986552169224410, -6.224258026782483633, 11.49999999999998934 ) ) ;
#28273 = CARTESIAN_POINT ( 'NONE',  ( -1.292025413547811308, -5.876774720514411854, 19.72913074730690752 ) ) ;
#28274 = CARTESIAN_POINT ( 'NONE',  ( 32.53346577320678534, 1.682774720514426114, -11.93731717363831102 ) ) ;
#28275 = DIRECTION ( 'NONE',  ( 3.773278334444166432E-23, -1.000000000000000000, 0.000000000000000000 ) ) ;
#28277 = AXIS2_PLACEMENT_3D ( 'NONE', #25929, #18321, #49291 ) ;
#28276 = CARTESIAN_POINT ( 'NONE',  ( -21.78311099772515647, -6.823855485095160489, -1.500000000000002220 ) ) ;
#28278 = APPLICATION_PROTOCOL_DEFINITION ( 'international standard', 'config_control_design', 1994, #47893 ) ;
#28279 = DIRECTION ( 'NONE',  ( -3.773278334453079030E-23, 0.9999999999976377785, 2.173523156925979128E-06 ) ) ;
#28280 = PLANE ( 'NONE',  #15213 ) ;
#28281 = CARTESIAN_POINT ( 'NONE',  ( 8.874027960929927517, 17.90919871486395465, 11.49999999999999645 ) ) ;
#28282 = CARTESIAN_POINT ( 'NONE',  ( -50.52287095715006160, -23.48783264082477018, -1.443836473390095021 ) ) ;
#28283 = CARTESIAN_POINT ( 'NONE',  ( -57.62287095715004881, -23.48786465467241058, 11.44779295918254824 ) ) ;
#28284 = CARTESIAN_POINT ( 'NONE',  ( -48.57734287085806102, -24.65952944569304606, 1.056160979905697239 ) ) ;
#28285 = ORIENTED_EDGE ( 'NONE', *, *, #92769, .F. ) ;
#28286 = DIRECTION ( 'NONE',  ( 0.000000000000000000, 0.9999999999976377785, 2.173523156925979128E-06 ) ) ;
#28287 = EDGE_CURVE ( 'NONE', #51004, #51553, #24887, .T. ) ;
#28288 = CARTESIAN_POINT ( 'NONE',  ( 8.160000000000000142, 8.793627758918228565, -2.994553991265763049 ) ) ;
#28289 = TOROIDAL_SURFACE ( 'NONE', #76863, 1.020000000000000018, 3.060000000000000053 ) ;
#28290 = CARTESIAN_POINT ( 'NONE',  ( 9.217229664113554932, 19.63635308506117383, 11.49999999999998934 ) ) ;
#28291 = CARTESIAN_POINT ( 'NONE',  ( -92.62287095715005592, -23.48783264082479150, -1.443836473390063713 ) ) ;
#28292 = CARTESIAN_POINT ( 'NONE',  ( 3.395600993332231532, 19.23619202488179525, -1.500000000000002220 ) ) ;
#28293 = CARTESIAN_POINT ( 'NONE',  ( 30.53060340732035982, -1.477225279485574028, 19.84760796525321780 ) ) ;
#28294 = EDGE_CURVE ( 'NONE', #38212, #71187, #29451, .T. ) ;
#28295 = ORIENTED_EDGE ( 'NONE', *, *, #29753, .T. ) ;
#28296 = CALENDAR_DATE ( 2026, 9, 10 ) ;
#28297 = DIRECTION ( 'NONE',  ( -3.389844910009033029E-15, 1.000000000000000000, 0.000000000000000000 ) ) ;
#28298 = CARTESIAN_POINT ( 'NONE',  ( -52.62287095715006302, -24.65952944569304250, 1.056160979905695685 ) ) ;
#28299 = CARTESIAN_POINT ( 'NONE',  ( 20.14718400222343320, -3.498931157112906476, 11.49999999999999645 ) ) ;
#28300 = DIRECTION ( 'NONE',  ( 0.000000000000000000, -1.478457507934778393E-16, -1.000000000000000000 ) ) ;
#28301 = B_SPLINE_CURVE_WITH_KNOTS ( 'NONE', 3,
 ( #74161, #12241, #96996, #56456, #10260, #87888 ),
 .UNSPECIFIED., .F., .F.,
 ( 4, 2, 4 ),
 ( 6.391158118967745954E-06, 0.001387004593080787013, 0.002767618028042606333 ),
 .UNSPECIFIED. ) ;
#28302 = DIRECTION ( 'NONE',  ( -3.773278334453079618E-23, 0.9999999999976377785, 2.173523156925979975E-06 ) ) ;
#28303 = ORIENTED_EDGE ( 'NONE', *, *, #4320, .T. ) ;
#28304 = EDGE_CURVE ( 'NONE', #43699, #70639, #25897, .T. ) ;
#28305 = CARTESIAN_POINT ( 'NONE',  ( 31.42094490286590514, -4.276934461241891583, -0.4045216949806126339 ) ) ;
#28306 = CARTESIAN_POINT ( 'NONE',  ( -43.62287095715004881, -24.66019654487199020, 8.947790411086135265 ) ) ;
#28307 = CARTESIAN_POINT ( 'NONE',  ( -116.5581118885402958, -23.48786465467241769, 11.44779295918253759 ) ) ;
#28308 = ADVANCED_FACE ( 'NONE', ( #71080 ), #39616, .T. ) ;
#28309 = DIRECTION ( 'NONE',  ( -0.000000000000000000, 2.173523156925979552E-06, -0.9999999999976378895 ) ) ;
#28310 = ORIENTED_EDGE ( 'NONE', *, *, #57484, .T. ) ;
#28311 = DIRECTION ( 'NONE',  ( -0.000000000000000000, 1.000000000000000000, -0.000000000000000000 ) ) ;
#28312 = CARTESIAN_POINT ( 'NONE',  ( -22.55714481399219906, -4.634528848986672500, 11.49999999999999645 ) ) ;
#28313 = CARTESIAN_POINT ( 'NONE',  ( -7.601706241105644857, -21.46296766604531570, 11.49999999999998934 ) ) ;
#28314 = DIRECTION ( 'NONE',  ( 1.000000000000000000, 0.000000000000000000, 0.000000000000000000 ) ) ;
#28315 = PLANE ( 'NONE',  #70635 ) ;
#28316 = CARTESIAN_POINT ( 'NONE',  ( -31.62287095715005236, -29.50250243563736774, 8.947779886222150481 ) ) ;
#28317 = VECTOR ( 'NONE', #20397, 1000.000000000000114 ) ;
#28318 = B_SPLINE_CURVE_WITH_KNOTS ( 'NONE', 3,
 ( #46937, #39314, #70274, #755, #75878, #53568 ),
 .UNSPECIFIED., .F., .F.,
 ( 4, 2, 4 ),
 ( 1.570755371634376281E-05, 0.001396183895866089271, 0.002776660238015834711 ),
 .UNSPECIFIED. ) ;
#28319 = CARTESIAN_POINT ( 'NONE',  ( -90.62287095715004170, -24.99132157543084531, 2.256160258750667502 ) ) ;
#28320 = CARTESIAN_POINT ( 'NONE',  ( -110.5864157058229296, -24.92564183028978775, 1.928384488918251982 ) ) ;
#28321 = CARTESIAN_POINT ( 'NONE',  ( 17.35060923807083810, -13.37414737355047656, -1.500000000000002220 ) ) ;
#28322 = APPROVAL ( #23017, 'UNSPECIFIED' ) ;
#28323 = LINE ( 'NONE', #74982, #17045 ) ;
#28324 = FACE_OUTER_BOUND ( 'NONE', #95964, .T. ) ;
#28325 = CARTESIAN_POINT ( 'NONE',  ( -71.45309080802084623, -25.30256279997297497, 5.292638313163490871 ) ) ;
#28326 = DIRECTION ( 'NONE',  ( -3.773278334453079030E-23, 0.9999999999976377785, 2.173523156925978705E-06 ) ) ;
#28327 = EDGE_LOOP ( 'NONE', ( #44326, #70534, #7393, #24440 ) ) ;
#28328 = CARTESIAN_POINT ( 'NONE',  ( 10.78675619948152864, -17.38023510967517637, -1.500000000000002220 ) ) ;
#28329 = ORIENTED_EDGE ( 'NONE', *, *, #64015, .T. ) ;
#28330 = ORIENTED_EDGE ( 'NONE', *, *, #23504, .F. ) ;
#28331 = ORIENTED_EDGE ( 'NONE', *, *, #90780, .F. ) ;
#28332 = CARTESIAN_POINT ( 'NONE',  ( 13.09964176094197441, 18.96253433080681106, 11.49999999999998934 ) ) ;
#28333 = CARTESIAN_POINT ( 'NONE',  ( -61.49060039123366295, -24.65952944569304606, 1.056160979905699682 ) ) ;
#28334 = CARTESIAN_POINT ( 'NONE',  ( -20.01257119864951051, 2.908879540851186274, -1.500000000000002220 ) ) ;
#28335 = ORIENTED_EDGE ( 'NONE', *, *, #20160, .T. ) ;
#28336 = CARTESIAN_POINT ( 'NONE',  ( -98.62287095715009855, -24.33927499327854704, 9.819080762295815390 ) ) ;
#28337 = CARTESIAN_POINT ( 'NONE',  ( 6.150000000000003908, 1.999999999999998224, 18.24068255301868291 ) ) ;
#28338 = LINE ( 'NONE', #96358, #28483 ) ;
#28339 = CARTESIAN_POINT ( 'NONE',  ( 9.299999999999993605, 12.00000000000002309, 2.100000000000000089 ) ) ;
#28341 = EDGE_LOOP ( 'NONE', ( #90506, #90499, #35944, #99370 ) ) ;
#28340 = CARTESIAN_POINT ( 'NONE',  ( 9.091334071971768793, -19.38302982324925239, 11.49999999999999645 ) ) ;
#28342 = DIRECTION ( 'NONE',  ( -0.000000000000000000, 2.173523156925979552E-06, -0.9999999999976378895 ) ) ;
#28343 = VERTEX_POINT ( 'NONE', #17282 ) ;
#28344 = CARTESIAN_POINT ( 'NONE',  ( -7.755428854246955161, -20.87388092083558888, -1.500000000000002220 ) ) ;
#28345 = CARTESIAN_POINT ( 'NONE',  ( 18.79598114143782084, -8.675585332008726169, -1.500000000000002220 ) ) ;
#28346 = VECTOR ( 'NONE', #5099, 1000.000000000000227 ) ;
#28347 = ORIENTED_EDGE ( 'NONE', *, *, #8107, .F. ) ;
#28348 = DIRECTION ( 'NONE',  ( 0.000000000000000000, -0.000000000000000000, -1.000000000000000000 ) ) ;
#28349 = VERTEX_POINT ( 'NONE', #79175 ) ;
#28350 = DIRECTION ( 'NONE',  ( 0.000000000000000000, 0.000000000000000000, -1.000000000000000000 ) ) ;
#28351 = ORIENTED_EDGE ( 'NONE', *, *, #81227, .T. ) ;
#28352 = CARTESIAN_POINT ( 'NONE',  ( -20.67734376658059858, -3.193854526364364954, -1.500000000000002220 ) ) ;
#28353 = EDGE_CURVE ( 'NONE', #17395, #44756, #74030, .T. ) ;
#28354 = CARTESIAN_POINT ( 'NONE',  ( 12.66425630052701479, 17.85959152241435177, 11.49999999999999645 ) ) ;
#28355 = AXIS2_PLACEMENT_3D ( 'NONE', #32356, #17127, #56718 ) ;
#28356 = CARTESIAN_POINT ( 'NONE',  ( -69.34303308397305443, -29.50249648326654039, 6.209198155459374924 ) ) ;
#28357 = CARTESIAN_POINT ( 'NONE',  ( -11.40494320173684351, 19.43794304404440254, -1.500000000000002220 ) ) ;
#28358 = AXIS2_PLACEMENT_3D ( 'NONE', #55183, #31321, #62291 ) ;
#28359 = CARTESIAN_POINT ( 'NONE',  ( 20.89173079421859214, 1.537965369061287557, 11.49999999999998934 ) ) ;
#28360 = CARTESIAN_POINT ( 'NONE',  ( 6.351517594976544778, -6.376774720514417183, 20.09206396488320578 ) ) ;
#28361 = CARTESIAN_POINT ( 'NONE',  ( -91.52287095715003318, -23.48783264082477018, -1.443836473390089248 ) ) ;
#28362 = CARTESIAN_POINT ( 'NONE',  ( 6.179707021866671646, -6.376774720514426065, 21.45334750074374242 ) ) ;
#28363 = ORIENTED_EDGE ( 'NONE', *, *, #6760, .F. ) ;
#28364 = EDGE_CURVE ( 'NONE', #95809, #76588, #10174, .T. ) ;
#28365 = ORIENTED_EDGE ( 'NONE', *, *, #42967, .T. ) ;
#28366 = ORIENTED_EDGE ( 'NONE', *, *, #21976, .F. ) ;
#28367 = EDGE_CURVE ( 'NONE', #56450, #39922, #80186, .T. ) ;
#28368 = DIRECTION ( 'NONE',  ( 0.000000000000000000, 3.740001113483016365E-15, -1.000000000000000000 ) ) ;
#28369 = CARTESIAN_POINT ( 'NONE',  ( 21.15477495681221143, 3.540436534888726783, -1.500000000000002220 ) ) ;
#28370 = CARTESIAN_POINT ( 'NONE',  ( -86.62287095715005592, -23.48786465467241413, 11.44779295918254469 ) ) ;
#28371 = ORIENTED_EDGE ( 'NONE', *, *, #7092, .T. ) ;
#28372 = CARTESIAN_POINT ( 'NONE',  ( 7.532573551308565207, 19.69859070278346991, -1.500000000000002220 ) ) ;
#28373 = CARTESIAN_POINT ( 'NONE',  ( -92.52287095715006160, -24.64965694238407323, 8.947790433994196491 ) ) ;
#28374 = CARTESIAN_POINT ( 'NONE',  ( -124.6228709571500559, -24.64965695001469115, 8.947790433994175174 ) ) ;
#28375 = CARTESIAN_POINT ( 'NONE',  ( -57.52287095715005449, -24.65952944569304606, 1.056160979905695463 ) ) ;
#28376 = DIRECTION ( 'NONE',  ( 1.000000000000000000, -0.000000000000000000, -0.000000000000000000 ) ) ;
#28377 = CARTESIAN_POINT ( 'NONE',  ( 9.402885806365684829, 0.3587747205144265483, 29.04108526060719342 ) ) ;
#28378 = CARTESIAN_POINT ( 'NONE',  ( -19.88706384024380824, 9.709922325909349894, -1.500000000000002220 ) ) ;
#28379 = DIRECTION ( 'NONE',  ( -1.000000000000000000, -1.387778780781445429E-16, 0.000000000000000000 ) ) ;
#28380 = EDGE_CURVE ( 'NONE', #59937, #75883, #23883, .T. ) ;
#28381 = DIRECTION ( 'NONE',  ( -3.773278334453080206E-23, 0.9999999999976377785, 2.173523156925979975E-06 ) ) ;
#28382 = CARTESIAN_POINT ( 'NONE',  ( -99.52287095715010423, -23.95044443724993144, 10.65354141964649592 ) ) ;
#28383 = CARTESIAN_POINT ( 'NONE',  ( -100.5221652074179701, -23.48783264082477018, -1.443836473390090580 ) ) ;
#28384 = CARTESIAN_POINT ( 'NONE',  ( -19.30698013599780083, -2.078282243779251637, 11.49999999999998934 ) ) ;
#28385 = VECTOR ( 'NONE', #39650, 1000.000000000000000 ) ;
#28386 = CARTESIAN_POINT ( 'NONE',  ( 15.73328655151706101, -14.44092690703295467, 11.49999999999998934 ) ) ;
#28387 = PLANE ( 'NONE',  #46681 ) ;
#28388 = CARTESIAN_POINT ( 'NONE',  ( -48.85723664563188606, -25.20650842489795451, 6.812665538484691474 ) ) ;
#28389 = CARTESIAN_POINT ( 'NONE',  ( -56.62287095715005592, -29.50248528299804818, 1.056150453629034924 ) ) ;
#28390 = DIRECTION ( 'NONE',  ( -1.000000000000000000, -3.773278334444167608E-23, -8.201307833595939069E-29 ) ) ;
#28391 = CARTESIAN_POINT ( 'NONE',  ( -21.91535228782390732, -5.629186751109307885, -1.500000000000002220 ) ) ;
#28392 = ORIENTED_EDGE ( 'NONE', *, *, #84923, .F. ) ;
#28393 = CARTESIAN_POINT ( 'NONE',  ( 13.60020833695035947, 0.000000000000000000, 0.000000000000000000 ) ) ;
#28394 = CARTESIAN_POINT ( 'NONE',  ( -62.62287095715004881, -24.66019654487199020, 8.947790411086131712 ) ) ;
#28395 = CARTESIAN_POINT ( 'NONE',  ( -4.105667982141768313, -19.37954422259287668, 11.49999999999999645 ) ) ;
#28396 = LINE ( 'NONE', #51247, #8328 ) ;
#28397 = DIRECTION ( 'NONE',  ( 0.1875268396392986980, 0.000000000000000000, 0.9822594791677485837 ) ) ;
#28398 = ORIENTED_EDGE ( 'NONE', *, *, #82454, .F. ) ;
#28399 = LINE ( 'NONE', #37021, #96047 ) ;
#28400 = FACE_OUTER_BOUND ( 'NONE', #63018, .T. ) ;
#28401 = CARTESIAN_POINT ( 'NONE',  ( -100.7619115510279926, -25.17353336829146926, 7.069363366734568110 ) ) ;
#28402 = CARTESIAN_POINT ( 'NONE',  ( -18.67883320684159543, -10.89015303950203517, -1.500000000000002220 ) ) ;
#28403 = DIRECTION ( 'NONE',  ( -3.773278334453079030E-23, 0.9999999999976377785, 2.173523156925979128E-06 ) ) ;
#28404 = CARTESIAN_POINT ( 'NONE',  ( -8.550378450311910683, 17.38971893761031851, -1.500000000000002220 ) ) ;
#28405 = CARTESIAN_POINT ( 'NONE',  ( 24.50102500000003758, -9.528487854913448629, 1.500000000000004219 ) ) ;
#28406 = CARTESIAN_POINT ( 'NONE',  ( -94.62287095715005592, -29.50248528299804818, 1.056150453629040253 ) ) ;
#28407 = CARTESIAN_POINT ( 'NONE',  ( -11.05534852661189937, -16.44151763790470966, -1.500000000000002220 ) ) ;
#28408 = EDGE_CURVE ( 'NONE', #26747, #86903, #79063, .T. ) ;
#28409 = ORIENTED_EDGE ( 'NONE', *, *, #41434, .F. ) ;
#28410 = CARTESIAN_POINT ( 'NONE',  ( -12.21837793623082113, -16.16665877782589433, 11.49999999999999645 ) ) ;
#28411 = CARTESIAN_POINT ( 'NONE',  ( -119.5228709571500758, -23.96177878511309345, 10.65340807706329151 ) ) ;
#28412 = CIRCLE ( 'NONE', #60815, 2.349999999999999645 ) ;
#28413 = EDGE_CURVE ( 'NONE', #71294, #38181, #37913, .T. ) ;
#28414 = DIRECTION ( 'NONE',  ( -3.773278334453079030E-23, 0.9999999999976377785, 2.173523156925979128E-06 ) ) ;
#28415 = ORIENTED_EDGE ( 'NONE', *, *, #60045, .T. ) ;
#28416 = FACE_OUTER_BOUND ( 'NONE', #43334, .T. ) ;
#28417 = CARTESIAN_POINT ( 'NONE',  ( -50.52287095715006160, -29.50250786944525672, 11.44777988621624054 ) ) ;
#28418 = CARTESIAN_POINT ( 'NONE',  ( -51.04357394935764347, -29.50249372652338664, 4.940868828539293212 ) ) ;
#28419 = DIRECTION ( 'NONE',  ( -1.000000000000000000, 0.000000000000000000, 0.000000000000000000 ) ) ;
#28420 = DIRECTION ( 'NONE',  ( 1.000000000000000000, 0.000000000000000000, 0.000000000000000000 ) ) ;
#28421 = CARTESIAN_POINT ( 'NONE',  ( -1.723993941171178879, -19.98520929721398431, -1.500000000000002220 ) ) ;
#28422 = B_SPLINE_CURVE_WITH_KNOTS ( 'NONE', 3,
 ( #73273, #27092, #11366, #3767 ),
 .UNSPECIFIED., .F., .F.,
 ( 4, 4 ),
 ( 1.387778780781445521E-17, 0.001341346153846192935 ),
 .UNSPECIFIED. ) ;
#28423 = VECTOR ( 'NONE', #50097, 1000.000000000000000 ) ;
#28424 = CARTESIAN_POINT ( 'NONE',  ( 33.13288845015618023, 0.3587747205144265483, -0.1650522222209214185 ) ) ;
#28425 = EDGE_LOOP ( 'NONE', ( #72700, #74572, #72563, #23425, #50165, #99968, #34722 ) ) ;
#28426 = AXIS2_PLACEMENT_3D ( 'NONE', #8862, #47934, #15963 ) ;
#28427 = CARTESIAN_POINT ( 'NONE',  ( -49.68676680831369197, -25.31297152054679245, 4.434853371053554483 ) ) ;
#28428 = FACE_OUTER_BOUND ( 'NONE', #78639, .T. ) ;
#28429 = DIRECTION ( 'NONE',  ( 1.000000000000000000, -0.000000000000000000, -0.000000000000000000 ) ) ;
#28430 = FACE_OUTER_BOUND ( 'NONE', #94250, .T. ) ;
#28431 = EDGE_CURVE ( 'NONE', #65949, #90027, #23330, .T. ) ;
#28432 = DIRECTION ( 'NONE',  ( 0.000000000000000000, 2.173523156925980399E-06, -0.9999999999976378895 ) ) ;
#28433 = CARTESIAN_POINT ( 'NONE',  ( -10.09097066620046235, 20.03973272787133553, 11.49999999999999645 ) ) ;
#28434 = CARTESIAN_POINT ( 'NONE',  ( -2.899999999999996803, 33.29999999999999716, 0.000000000000000000 ) ) ;
#28435 = VERTEX_POINT ( 'NONE', #47238 ) ;
#28436 = CARTESIAN_POINT ( 'NONE',  ( 10.94010344783756672, -17.16519937159427656, 11.49999999999998934 ) ) ;
#28437 = ORIENTED_EDGE ( 'NONE', *, *, #92617, .F. ) ;
#28438 = CARTESIAN_POINT ( 'NONE',  ( 21.44032754495887261, 8.191337786432022483, 11.49999999999998934 ) ) ;
#28439 = CARTESIAN_POINT ( 'NONE',  ( -61.52287095715006160, -24.64965694238407323, 8.947790433994201820 ) ) ;
#28441 = ORIENTED_EDGE ( 'NONE', *, *, #54167, .F. ) ;
#28440 = EDGE_CURVE ( 'NONE', #47768, #36906, #56301, .T. ) ;
#28442 = CARTESIAN_POINT ( 'NONE',  ( -4.621320343559254695, 11.49999999999999467, 0.000000000000000000 ) ) ;
#28443 = EDGE_CURVE ( 'NONE', #27352, #94885, #39163, .T. ) ;
#28444 = CARTESIAN_POINT ( 'NONE',  ( -67.52287095715007581, -24.50321055353805733, 9.387540953477515160 ) ) ;
#28445 = CARTESIAN_POINT ( 'NONE',  ( 13.91401389203221406, -6.376774720514426953, 158.0376437107427137 ) ) ;
#28447 = ORIENTED_EDGE ( 'NONE', *, *, #58422, .T. ) ;
#28446 = CARTESIAN_POINT ( 'NONE',  ( -21.15187133135857422, -0.9709546189074961253, 11.49999999999999645 ) ) ;
#28448 = VECTOR ( 'NONE', #70744, 1000.000000000000000 ) ;
#28449 = ORIENTED_EDGE ( 'NONE', *, *, #88090, .F. ) ;
#28450 = CARTESIAN_POINT ( 'NONE',  ( -20.56814720681451902, 8.302189128749821734, -1.500000000000002220 ) ) ;
#28451 = CARTESIAN_POINT ( 'NONE',  ( 7.647619880454145758, 19.11525441646967849, 11.49999999999998934 ) ) ;
#28452 = ORIENTED_EDGE ( 'NONE', *, *, #173, .T. ) ;
#28453 = ORIENTED_EDGE ( 'NONE', *, *, #67647, .T. ) ;
#28454 = DIRECTION ( 'NONE',  ( 0.000000000000000000, 1.000000000000000000, 0.000000000000000000 ) ) ;
#28455 = B_SPLINE_CURVE_WITH_KNOTS ( 'NONE', 3,
 ( #33657, #94544, #57009, #25032 ),
 .UNSPECIFIED., .F., .F.,
 ( 4, 4 ),
 ( 0.8393800999571321420, 0.8403808469978977236 ),
 .UNSPECIFIED. ) ;
#28456 = CARTESIAN_POINT ( 'NONE',  ( -126.6228709571500559, -24.35013146730204525, 9.818937971375094165 ) ) ;
#28457 = ORIENTED_EDGE ( 'NONE', *, *, #99124, .F. ) ;
#28458 = ORIENTED_EDGE ( 'NONE', *, *, #19534, .T. ) ;
#28459 = B_SPLINE_CURVE_WITH_KNOTS ( 'NONE', 3,
 ( #99010, #73819, #4322, #19526, #67596, #45743, #50004, #21384, #30006, #30510, #90916, #61479, #53366, #52361, #44751, #83295, #11424, #13775 ),
 .UNSPECIFIED., .F., .F.,
 ( 4, 2, 2, 2, 2, 2, 2, 2, 4 ),
 ( 0.000000000000000000, 0.0002960763747946566164, 0.0005921527495893132327, 0.0008882291243839698491, 0.001184305499178626465, 0.001480381873973283082, 0.001776458248767939698, 0.002072534623562596531, 0.002368610998357252931 ),
 .UNSPECIFIED. ) ;
#28460 =( REPRESENTATION_RELATIONSHIP ('NONE','NONE', #96270, #55609 ) REPRESENTATION_RELATIONSHIP_WITH_TRANSFORMATION ( #81090 )SHAPE_REPRESENTATION_RELATIONSHIP( ) );
#28461 = ORIENTED_EDGE ( 'NONE', *, *, #38465, .F. ) ;
#28462 = DIRECTION ( 'NONE',  ( 1.000000000000000000, 3.773278334444167608E-23, 8.201307833595939069E-29 ) ) ;
#28463 = CARTESIAN_POINT ( 'NONE',  ( -28.61148789775794654, -23.58142141106679546, 11.05961558438220749 ) ) ;
#28464 = CARTESIAN_POINT ( 'NONE',  ( -49.10457154551149728, -25.27419814425984512, 3.999772249604824914 ) ) ;
#28465 = CARTESIAN_POINT ( 'NONE',  ( -20.46667790307254009, -3.548193229090686796, -1.500000000000002220 ) ) ;
#28466 = EDGE_CURVE ( 'NONE', #55720, #61817, #7530, .T. ) ;
#28467 = CARTESIAN_POINT ( 'NONE',  ( 21.72137571921558319, 1.130696696492564213, 11.49999999999999645 ) ) ;
#28468 = ORIENTED_EDGE ( 'NONE', *, *, #36713, .F. ) ;
#28469 = CARTESIAN_POINT ( 'NONE',  ( -40.91098280806539833, -25.31583749408676809, 4.981853969359134382 ) ) ;
#28470 = CARTESIAN_POINT ( 'NONE',  ( -4.141025641025642301, -5.876774720514409189, 19.19230769230769695 ) ) ;
#28471 = CARTESIAN_POINT ( 'NONE',  ( -115.6239652621308664, -24.92564183028979130, 1.928384488918252870 ) ) ;
#28472 = CARTESIAN_POINT ( 'NONE',  ( 4.981011153104904388, 21.88276397462241363, -1.500000000000002220 ) ) ;
#28473 = CARTESIAN_POINT ( 'NONE',  ( -51.29687923781917647, -25.26334590255974533, 3.993462177038400895 ) ) ;
#28474 = CARTESIAN_POINT ( 'NONE',  ( -102.5228709571500758, -24.64965694238407323, 8.947790433994194714 ) ) ;
#28475 = ORIENTED_EDGE ( 'NONE', *, *, #59414, .T. ) ;
#28476 = CARTESIAN_POINT ( 'NONE',  ( -71.67926322476502321, -25.28257675302215901, 5.899957443109282273 ) ) ;
#28477 = CARTESIAN_POINT ( 'NONE',  ( -77.62287095715009855, -23.47596703998600631, 11.44779298504227683 ) ) ;
#28478 = ORIENTED_EDGE ( 'NONE', *, *, #76044, .T. ) ;
#28479 = ORIENTED_EDGE ( 'NONE', *, *, #36961, .F. ) ;
#28481 = ADVANCED_FACE ( 'NONE', ( #11662 ), #3574, .F. ) ;
#28480 = DIRECTION ( 'NONE',  ( 0.000000000000000000, -1.000000000000000000, 0.000000000000000000 ) ) ;
#28482 = ORIENTED_EDGE ( 'NONE', *, *, #6718, .T. ) ;
#28483 = VECTOR ( 'NONE', #96857, 1000.000000000000000 ) ;
#28484 = CARTESIAN_POINT ( 'NONE',  ( -4.730540317195566224, 20.75322969461001676, -1.500000000000002220 ) ) ;
#28485 = ADVANCED_FACE ( 'NONE', ( #50741 ), #60236, .F. ) ;
#28486 = VERTEX_POINT ( 'NONE', #29262 ) ;
#28487 = CARTESIAN_POINT ( 'NONE',  ( -80.52287095715004739, -25.00182538069145366, 7.747789668545104647 ) ) ;
#28488 = VECTOR ( 'NONE', #48611, 1000.000000000000000 ) ;
#28489 = CARTESIAN_POINT ( 'NONE',  ( 9.643594380127815668, 19.59848315111488759, -1.500000000000002220 ) ) ;
#28490 = CARTESIAN_POINT ( 'NONE',  ( 10.86264264036872440, -0.3587747205144257157, -28.05717073575603138 ) ) ;
#28491 = CARTESIAN_POINT ( 'NONE',  ( 12.08046422559826816, 19.21373320108137861, -1.500000000000002220 ) ) ;
#28492 = CARTESIAN_POINT ( 'NONE',  ( -40.75388878839229534, -25.28892429803972774, 3.329423022938666765 ) ) ;
#28493 = VECTOR ( 'NONE', #23264, 1000.000000000000000 ) ;
#28494 = DIRECTION ( 'NONE',  ( -0.6401411605457395515, 0.000000000000000000, -0.7682573101345366862 ) ) ;
#28495 = CARTESIAN_POINT ( 'NONE',  ( -0.1377007522546883911, -21.91379463844567965, -1.500000000000002220 ) ) ;
#28496 = CARTESIAN_POINT ( 'NONE',  ( -39.52287095715004739, -24.34917612406835730, 0.1852690917426483286 ) ) ;
#28497 = ORIENTED_EDGE ( 'NONE', *, *, #5664, .T. ) ;
#28498 = CARTESIAN_POINT ( 'NONE',  ( -122.6239430697742847, -24.51419770103158413, 9.386484678747169852 ) ) ;
#28499 = ADVANCED_FACE ( 'NONE', ( #22135 ), #34015, .F. ) ;
#28500 = AXIS2_PLACEMENT_3D ( 'NONE', #82672, #97403, #76541 ) ;
#28501 = VECTOR ( 'NONE', #30429, 1000.000000000000000 ) ;
#28502 = EDGE_CURVE ( 'NONE', #78378, #51347, #57962, .T. ) ;
#28503 = ORIENTED_EDGE ( 'NONE', *, *, #1033, .F. ) ;
#28504 = FACE_OUTER_BOUND ( 'NONE', #3967, .T. ) ;
#28505 = DIRECTION ( 'NONE',  ( 0.000000000000000000, -1.000000000000000000, -2.816109538923387391E-16 ) ) ;
#28506 = CARTESIAN_POINT ( 'NONE',  ( -29.49875734969026198, 0.3587747205144265483, 10.11402280011862587 ) ) ;
#28507 = CARTESIAN_POINT ( 'NONE',  ( -15.80959461918071618, 14.24510877297761446, -1.500000000000002220 ) ) ;
#28508 = CARTESIAN_POINT ( 'NONE',  ( -98.62739836056972820, -24.35071581493543746, 9.817618358456027039 ) ) ;
#28509 = CARTESIAN_POINT ( 'NONE',  ( -26.12582186233688830, -24.97064840753675341, 4.293463527599305607 ) ) ;
#28510 = CARTESIAN_POINT ( 'NONE',  ( -114.5228709571500474, -24.51283580621455371, 0.6167428607046516742 ) ) ;
#28511 = CARTESIAN_POINT ( 'NONE',  ( -29.58953762381673869, -23.40614417124189117, -1.443836160644816680 ) ) ;
#28512 = CARTESIAN_POINT ( 'NONE',  ( -117.5912915777627177, -23.96169478059714564, 10.65365249895717170 ) ) ;
#28513 = ORIENTED_EDGE ( 'NONE', *, *, #59889, .T. ) ;
#28514 = CARTESIAN_POINT ( 'NONE',  ( -10.41718274906430786, -16.55731393670301088, 11.49999999999999645 ) ) ;
#28515 = CARTESIAN_POINT ( 'NONE',  ( -66.62287095715009855, -23.73934037231756733, 11.05740245334329153 ) ) ;
#28516 = DIRECTION ( 'NONE',  ( 0.000000000000000000, -1.000000000000000000, 0.000000000000000000 ) ) ;
#28517 = ORIENTED_EDGE ( 'NONE', *, *, #99415, .T. ) ;
#28518 = PLANE ( 'NONE',  #94377 ) ;
#28519 = CARTESIAN_POINT ( 'NONE',  ( -101.9326655587415331, -25.23357337914073995, 6.326899518756052387 ) ) ;
#28520 = B_SPLINE_CURVE_WITH_KNOTS ( 'NONE', 3,
 ( #45464, #61688, #60192, #98729 ),
 .UNSPECIFIED., .F., .F.,
 ( 4, 4 ),
 ( 0.000000000000000000, 9.999999999999592548E-05 ),
 .UNSPECIFIED. ) ;
#28521 = CARTESIAN_POINT ( 'NONE',  ( -116.5895376238167387, -23.48783264082478794, -1.443836473390058606 ) ) ;
#28522 = CARTESIAN_POINT ( 'NONE',  ( -106.5228709571500758, -24.65952944569305316, 1.056160979905704123 ) ) ;
#28523 = EDGE_CURVE ( 'NONE', #98946, #50260, #49756, .T. ) ;
#28524 = CARTESIAN_POINT ( 'NONE',  ( -16.18664964019209052, -11.25563402961023662, -1.500000000000002220 ) ) ;
#28525 = VERTEX_POINT ( 'NONE', #81182 ) ;
#28526 = CARTESIAN_POINT ( 'NONE',  ( 10.95759398273795249, 4.132774720514426292, -26.86884997114579932 ) ) ;
#28527 = CARTESIAN_POINT ( 'NONE',  ( 29.73860345376319358, 3.356774720514427379, 1.647607965253216067 ) ) ;
#28528 = PERSON_AND_ORGANIZATION_ROLE ( 'creator' ) ;
#28529 = ORIENTED_EDGE ( 'NONE', *, *, #1623, .F. ) ;
#28530 = CARTESIAN_POINT ( 'NONE',  ( 8.974114877419669511, -0.9738252115640718687, 3.736985260579222867 ) ) ;
#28531 = DIRECTION ( 'NONE',  ( 0.000000000000000000, -1.000000000000000000, 0.000000000000000000 ) ) ;
#28532 = CARTESIAN_POINT ( 'NONE',  ( -47.63994789387633944, -24.15543982623907127, -0.2315651400026536022 ) ) ;
#28533 = CARTESIAN_POINT ( 'NONE',  ( -118.5879173097015240, -24.65952944569305316, 1.056160979905708119 ) ) ;
#28534 = CARTESIAN_POINT ( 'NONE',  ( -6.905879715866854340, -6.376774720514411854, 19.48240003225459560 ) ) ;
#28535 = DIRECTION ( 'NONE',  ( 0.000000000000000000, -2.173523156925980399E-06, 0.9999999999976378895 ) ) ;
#28536 = CARTESIAN_POINT ( 'NONE',  ( -116.5228709571500616, -29.50250243563736774, 8.947779886222134493 ) ) ;
#28537 = CARTESIAN_POINT ( 'NONE',  ( -7.409219584043468920, -18.53548363135739052, 11.49999999999998934 ) ) ;
#28538 = CARTESIAN_POINT ( 'NONE',  ( -4.621320343559254695, 11.49999999999999645, 2.100000000000000089 ) ) ;
#28539 = CARTESIAN_POINT ( 'NONE',  ( -0.03226556487338757412, -22.63229690711892772, 1.846386587601361651 ) ) ;
#28540 = EDGE_LOOP ( 'NONE', ( #25955, #11490, #10768, #53913 ) ) ;
#28541 = CARTESIAN_POINT ( 'NONE',  ( -128.5228709571500758, -23.48786465467242479, 11.44779295918253581 ) ) ;
#28542 = CARTESIAN_POINT ( 'NONE',  ( 4.653726706778644306, -5.876774720514415407, 20.04674869880385302 ) ) ;
#28543 = VECTOR ( 'NONE', #60142, 999.9999999999998863 ) ;
#28544 = B_SPLINE_CURVE_WITH_KNOTS ( 'NONE', 3,
 ( #26856, #89758, #51198, #65945, #50202, #56829, #87762, #96868, #72541, #82141, #27853, #19236, #3034, #25853, #88767, #95366, #11622, #73535, #18735, #58320, #18244, #4028, #58810 ),
 .UNSPECIFIED., .F., .F.,
 ( 4, 1, 1, 1, 1, 1, 1, 1, 1, 1, 1, 1, 1, 1, 1, 1, 1, 1, 1, 1, 4 ),
 ( 0.000000000000000000, 0.06568119799063895647, 0.1284864641740642022, 0.1881751303280073950, 0.2451061306699852116, 0.2994484245294744551, 0.3508229360093824134, 0.3999416805337764336, 0.4466717436323716650, 0.4912545333734980035, 0.5333763442704358981, 0.5738527549682231887, 0.6125263117194529316, 0.6495971364453292374, 0.6855320415538496137, 0.7201057860682000822, 0.7538376629736500689, 0.8189254160467134280, 0.8804934616501639555, 0.9403113338460573623, 1.000000000000000000 ),
 .UNSPECIFIED. ) ;
#28545 = FACE_OUTER_BOUND ( 'NONE', #98402, .T. ) ;
#28546 = DIRECTION ( 'NONE',  ( 0.000000000000000000, -2.173523156925980399E-06, 0.9999999999976378895 ) ) ;
#28547 = CARTESIAN_POINT ( 'NONE',  ( -125.0507906094695585, -25.24724330731294231, 6.200220586889952479 ) ) ;
#28548 = CARTESIAN_POINT ( 'NONE',  ( -81.62949391327481408, -24.34968618360933945, 0.1864209137778954084 ) ) ;
#28549 = CARTESIAN_POINT ( 'NONE',  ( -2.899999999999996803, 31.80000000000000071, 2.100000000000000089 ) ) ;
#28550 = CARTESIAN_POINT ( 'NONE',  ( -1.501937386944296460, -5.876774720514415407, 19.86422795159478483 ) ) ;
#28551 = AXIS2_PLACEMENT_3D ( 'NONE', #42943, #72888, #65298 ) ;
#28553 = EDGE_CURVE ( 'NONE', #61715, #57842, #17235, .T. ) ;
#28552 = ORIENTED_EDGE ( 'NONE', *, *, #75219, .F. ) ;
#28554 = B_SPLINE_CURVE_WITH_KNOTS ( 'NONE', 3,
 ( #95737, #81518, #66308, #95237, #80509, #11993, #97235, #72911, #26226, #2906 ),
 .UNSPECIFIED., .F., .F.,
 ( 4, 2, 2, 2, 4 ),
 ( 0.000000000000000000, 0.0004686948575969753904, 0.0009373897151939507809, 0.001406084572790926171, 0.001874779430387901562 ),
 .UNSPECIFIED. ) ;
#28555 = CARTESIAN_POINT ( 'NONE',  ( -79.62287095715007013, -24.35013146730204525, 9.818937971375108376 ) ) ;
#28557 = VECTOR ( 'NONE', #71287, 1000.000000000000000 ) ;
#28556 = CARTESIAN_POINT ( 'NONE',  ( 5.742690948595683409, -6.376774720514427841, 21.62260900090680593 ) ) ;
#28558 = VERTEX_POINT ( 'NONE', #53118 ) ;
#28559 = VECTOR ( 'NONE', #63717, 1000.000000000000114 ) ;
#28560 = CARTESIAN_POINT ( 'NONE',  ( 19.26017855675105750, 6.235128648364509196, 11.49999999999998934 ) ) ;
#28561 = B_SPLINE_CURVE_WITH_KNOTS ( 'NONE', 3,
 ( #41568, #18702, #81114, #64425 ),
 .UNSPECIFIED., .F., .F.,
 ( 4, 4 ),
 ( 0.000000000000000000, 9.999999999998897304E-05 ),
 .UNSPECIFIED. ) ;
#28562 = CARTESIAN_POINT ( 'NONE',  ( -69.67778434337223814, -25.31561343761894634, 4.981274948899643285 ) ) ;
#28563 = VECTOR ( 'NONE', #97038, 1000.000000000000000 ) ;
#28564 = CARTESIAN_POINT ( 'NONE',  ( 20.98022359556508931, 4.383291743620153724, -17.13764241148466994 ) ) ;
#28565 = EDGE_CURVE ( 'NONE', #55078, #70110, #12374, .T. ) ;
#28566 = EDGE_CURVE ( 'NONE', #96746, #83609, #94693, .T. ) ;
#28567 = AXIS2_PLACEMENT_3D ( 'NONE', #68753, #38791, #69246 ) ;
#28568 = FACE_OUTER_BOUND ( 'NONE', #27928, .T. ) ;
#28569 = EDGE_CURVE ( 'NONE', #91742, #61087, #43128, .T. ) ;
#28570 = EDGE_LOOP ( 'NONE', ( #21248, #65194, #23955, #40149 ) ) ;
#28571 = CARTESIAN_POINT ( 'NONE',  ( -79.97841713288102028, -25.30708236192187854, 4.547326657696674879 ) ) ;
#28572 = CARTESIAN_POINT ( 'NONE',  ( -52.52287095715005449, -24.35013146730203104, 9.818937971375113705 ) ) ;
#28573 = CARTESIAN_POINT ( 'NONE',  ( 1.781536345648733199, 20.00535218256611358, -1.500000000000002220 ) ) ;
#28574 = CARTESIAN_POINT ( 'NONE',  ( -17.33045254171255678, -11.89390297951003816, 11.49999999999999645 ) ) ;
#28575 = EDGE_CURVE ( 'NONE', #45069, #45070, #21634, .T. ) ;
#28576 = CARTESIAN_POINT ( 'NONE',  ( -29.11574841292185312, -25.12648593425884513, 6.386170400369471700 ) ) ;
#28577 = CARTESIAN_POINT ( 'NONE',  ( -70.58914684821826313, -24.52399227489126687, 9.353111116836529959 ) ) ;
#28578 = CARTESIAN_POINT ( 'NONE',  ( -22.03165466229905789, 1.424673820674137614, 11.49999999999998934 ) ) ;
#28579 = CARTESIAN_POINT ( 'NONE',  ( -47.22287095715005023, -23.47596703998600276, 11.44779298504227683 ) ) ;
#28580 = CARTESIAN_POINT ( 'NONE',  ( 9.278253834636469577, -5.876774720514426953, 18.51871304725684553 ) ) ;
#28581 = CARTESIAN_POINT ( 'NONE',  ( -34.52287095715006160, -29.50248528299804818, 1.056150453629029817 ) ) ;
#28582 = ORIENTED_EDGE ( 'NONE', *, *, #45028, .T. ) ;
#28583 = CARTESIAN_POINT ( 'NONE',  ( -99.12732697106135049, -25.26762180873494756, 3.920099948859327554 ) ) ;
#28584 = CARTESIAN_POINT ( 'NONE',  ( -31.57094520315825648, -23.48783264082477018, -1.443836473390079256 ) ) ;
#28585 = ORIENTED_EDGE ( 'NONE', *, *, #45555, .F. ) ;
#28586 = ORIENTED_EDGE ( 'NONE', *, *, #20269, .T. ) ;
#28587 = CARTESIAN_POINT ( 'NONE',  ( -49.52287095715006160, -23.47596703998600631, 11.44779298504229104 ) ) ;
#28588 = CARTESIAN_POINT ( 'NONE',  ( -106.6228709571500559, -23.48786465467241769, 11.44779295918253759 ) ) ;
#28589 = CARTESIAN_POINT ( 'NONE',  ( -48.52287095715006160, -24.66019654487200086, 8.947790411086119278 ) ) ;
#28590 = B_SPLINE_CURVE_WITH_KNOTS ( 'NONE', 3,
 ( #4484, #3488, #57774, #2991 ),
 .UNSPECIFIED., .F., .F.,
 ( 4, 4 ),
 ( 0.7710505883516606263, 0.7800570196237761600 ),
 .UNSPECIFIED. ) ;
#28591 = CARTESIAN_POINT ( 'NONE',  ( 20.58124611042576646, 0.8182449333618511123, -1.500000000000002220 ) ) ;
#28592 = EDGE_CURVE ( 'NONE', #89739, #24459, #12525, .T. ) ;
#28593 = EDGE_CURVE ( 'NONE', #20863, #35820, #83545, .T. ) ;
#28594 = CARTESIAN_POINT ( 'NONE',  ( -17.63906703526961550, 12.34593017946836291, 11.49999999999999645 ) ) ;
#28595 = ORIENTED_EDGE ( 'NONE', *, *, #26986, .T. ) ;
#28596 = CARTESIAN_POINT ( 'NONE',  ( -48.62287095715004881, -24.64965695001467694, 8.947790433994185832 ) ) ;
#28597 = CARTESIAN_POINT ( 'NONE',  ( -99.49719608488790357, -25.30438760448027935, 4.819451417661368531 ) ) ;
#28598 = CIRCLE ( 'NONE', #64348, 252.4458649670781085 ) ;
#28599 = DIRECTION ( 'NONE',  ( 0.000000000000000000, 0.000000000000000000, 1.000000000000000000 ) ) ;
#28600 = CARTESIAN_POINT ( 'NONE',  ( 21.44611857939883137, 6.294191480875499067, 11.49999999999998934 ) ) ;
#28601 = CARTESIAN_POINT ( 'NONE',  ( -93.52287095715006160, -23.47593901973090524, -1.443836447538996648 ) ) ;
#28602 = FACE_OUTER_BOUND ( 'NONE', #18849, .T. ) ;
#28603 = EDGE_CURVE ( 'NONE', #9599, #14974, #74078, .T. ) ;
#28604 = ORIENTED_EDGE ( 'NONE', *, *, #61591, .F. ) ;
#28605 = CARTESIAN_POINT ( 'NONE',  ( -110.5228709571500616, -25.00158670708909625, 2.256160236439166411 ) ) ;
#28606 = CARTESIAN_POINT ( 'NONE',  ( -48.22287095715007155, -23.47596703998600276, 11.44779298504227683 ) ) ;
#28607 = B_SPLINE_CURVE_WITH_KNOTS ( 'NONE', 3,
 ( #11475, #43930, #34822, #19582 ),
 .UNSPECIFIED., .F., .F.,
 ( 4, 4 ),
 ( 0.000000000000000000, 9.999999999997510880E-05 ),
 .UNSPECIFIED. ) ;
#28608 = CARTESIAN_POINT ( 'NONE',  ( 20.33208665566141704, 4.825383418962623239, 11.49999999999998934 ) ) ;
#28609 = EDGE_LOOP ( 'NONE', ( #67296, #90429, #4093, #85818 ) ) ;
#28612 = ORIENTED_EDGE ( 'NONE', *, *, #71348, .T. ) ;
#28611 = EDGE_CURVE ( 'NONE', #95350, #7760, #19040, .T. ) ;
#28610 = CARTESIAN_POINT ( 'NONE',  ( 14.61581676223891613, -2.682774720514426559, -27.35847991879931485 ) ) ;
#28613 = ORIENTED_EDGE ( 'NONE', *, *, #2595, .F. ) ;
#28614 = CARTESIAN_POINT ( 'NONE',  ( -100.5087600408661928, -24.63419186844611275, 9.035850630976915099 ) ) ;
#28615 = CARTESIAN_POINT ( 'NONE',  ( 11.82777538550527119, 17.46297031709455183, -1.500000000000002220 ) ) ;
#28616 = ORIENTED_EDGE ( 'NONE', *, *, #55762, .F. ) ;
#28617 = CARTESIAN_POINT ( 'NONE',  ( -60.52287095715006160, -24.99156044556119838, 7.747789690856173195 ) ) ;
#28618 = FACE_OUTER_BOUND ( 'NONE', #97999, .T. ) ;
#28619 = CARTESIAN_POINT ( 'NONE',  ( -120.5222358195599810, -23.48786465467241769, 11.44779295918253936 ) ) ;
#28620 = CARTESIAN_POINT ( 'NONE',  ( -76.63827036425878703, -23.96169478059713143, 10.65365249895718058 ) ) ;
#28621 = CARTESIAN_POINT ( 'NONE',  ( -74.62287095715005592, -24.65952944569304606, 1.056160979905696351 ) ) ;
#28622 = CARTESIAN_POINT ( 'NONE',  ( -3.058130702743298901, -21.54894043062209263, -1.500000000000002220 ) ) ;
#28623 = CARTESIAN_POINT ( 'NONE',  ( -98.62287095715005592, -23.48786465467241769, 11.44779295918254292 ) ) ;
#28625 = ORIENTED_EDGE ( 'NONE', *, *, #67772, .T. ) ;
#28624 = CARTESIAN_POINT ( 'NONE',  ( -14.53400517605410158, 16.95891092046126403, 11.49999999999999645 ) ) ;
#28626 = CARTESIAN_POINT ( 'NONE',  ( -57.52287095715003318, -24.66019654487198665, 8.947790411086121054 ) ) ;
#28627 = DIRECTION ( 'NONE',  ( 0.7071067811865474617, 0.000000000000000000, 0.7071067811865476838 ) ) ;
#28628 = FACE_OUTER_BOUND ( 'NONE', #60608, .T. ) ;
#28630 = ORIENTED_EDGE ( 'NONE', *, *, #15364, .F. ) ;
#28629 = EDGE_CURVE ( 'NONE', #56116, #62739, #53554, .T. ) ;
#28631 = VECTOR ( 'NONE', #75077, 1000.000000000000227 ) ;
#28632 = ADVANCED_FACE ( 'NONE', ( #91655 ), #92650, .F. ) ;
#28633 = VERTEX_POINT ( 'NONE', #93147 ) ;
#28634 = EDGE_CURVE ( 'NONE', #45943, #45676, #16523, .T. ) ;
#28635 = EDGE_LOOP ( 'NONE', ( #45772, #28210, #25252, #17125, #89820, #48327, #47088, #36855, #14683 ) ) ;
#28636 = CARTESIAN_POINT ( 'NONE',  ( -27.25988310792305214, -0.3587747205144265483, 30.32664379231667695 ) ) ;
#28637 = DIRECTION ( 'NONE',  ( -3.773278334453079618E-23, 0.9999999999976377785, 2.173523156925979975E-06 ) ) ;
#28638 = CARTESIAN_POINT ( 'NONE',  ( 30.60862754225505000, -4.127879075750807480, 27.06827100787837992 ) ) ;
#28639 = DIRECTION ( 'NONE',  ( -0.000000000000000000, 1.000000000000000000, -0.000000000000000000 ) ) ;
#28640 = CARTESIAN_POINT ( 'NONE',  ( -7.246369895950522277, -17.95243785538732340, -1.500000000000002220 ) ) ;
#28641 = CARTESIAN_POINT ( 'NONE',  ( -51.27945410110257995, -25.31566608536513030, 5.069311121527179331 ) ) ;
#28642 = ORIENTED_EDGE ( 'NONE', *, *, #36009, .T. ) ;
#28643 = AXIS2_PLACEMENT_3D ( 'NONE', #93752, #39475, #25751 ) ;
#28644 = CARTESIAN_POINT ( 'NONE',  ( 19.05472526407214673, 3.605321472892077050, 11.49999999999999645 ) ) ;
#28645 = LINE ( 'NONE', #81930, #69832 ) ;
#28646 = VECTOR ( 'NONE', #50329, 1000.000000000000000 ) ;
#28647 = ORIENTED_EDGE ( 'NONE', *, *, #4539, .F. ) ;
#28648 = DIRECTION ( 'NONE',  ( 0.000000000000000000, 0.000000000000000000, -1.000000000000000000 ) ) ;
#28649 = CARTESIAN_POINT ( 'NONE',  ( 10.77631500667670572, 5.356774720514423827, -24.99100794736120434 ) ) ;
#28650 = CARTESIAN_POINT ( 'NONE',  ( -64.52287095715006160, -29.50250243563736774, 8.947779886222145151 ) ) ;
#28651 = CIRCLE ( 'NONE', #4326, 2.500000000000189626 ) ;
#28652 = CARTESIAN_POINT ( 'NONE',  ( -36.52287095715008292, -24.51387760970724017, 9.387446482453407626 ) ) ;
#28653 = CARTESIAN_POINT ( 'NONE',  ( 19.03533760385612439, 4.641190475545474037, 11.49999999999998934 ) ) ;
#28654 = DIRECTION ( 'NONE',  ( 0.000000000000000000, 0.000000000000000000, 1.000000000000000000 ) ) ;
#28655 = EDGE_LOOP ( 'NONE', ( #97767, #13845, #4119, #94119 ) ) ;
#28656 = CARTESIAN_POINT ( 'NONE',  ( -21.01953065494444317, -4.859126342152997324, -1.500000000000002220 ) ) ;
#28657 = CARTESIAN_POINT ( 'NONE',  ( -86.52287095715006160, -23.47596703998600631, 11.44779298504228393 ) ) ;
#28658 = DIRECTION ( 'NONE',  ( -0.000000000000000000, 1.000000000000000000, -0.000000000000000000 ) ) ;
#28659 = LINE ( 'NONE', #44394, #78364 ) ;
#28660 = CARTESIAN_POINT ( 'NONE',  ( -100.4008197971955667, -25.18439335906099075, 3.294680639966506508 ) ) ;
#28661 = CARTESIAN_POINT ( 'NONE',  ( -22.94451526424785115, -1.264959178018935315, -1.500000000000002220 ) ) ;
#28662 = APPLICATION_PROTOCOL_DEFINITION ( 'international standard', 'config_control_design', 1994, #92623 ) ;
#28663 = DIRECTION ( 'NONE',  ( 0.000000000000000000, -1.000000000000000000, 0.000000000000000000 ) ) ;
#28664 = CARTESIAN_POINT ( 'NONE',  ( -100.6814946224345846, -25.30401792888237367, 5.197789011716578145 ) ) ;
#28665 = CARTESIAN_POINT ( 'NONE',  ( -4.233023369943174075, 19.68221892606961987, 11.49999999999999645 ) ) ;
#28666 = CARTESIAN_POINT ( 'NONE',  ( -101.5562042904833930, -24.64898659630528499, 1.056161002820828143 ) ) ;
#28667 = FACE_OUTER_BOUND ( 'NONE', #58174, .T. ) ;
#28668 = B_SPLINE_CURVE_WITH_KNOTS ( 'NONE', 3,
 ( #12862, #30088, #38197, #83876, #100074, #14857 ),
 .UNSPECIFIED., .F., .F.,
 ( 4, 2, 4 ),
 ( 6.384118678611908238E-06, 0.001386860460828373900, 0.002767336802978135821 ),
 .UNSPECIFIED. ) ;
#28669 = CARTESIAN_POINT ( 'NONE',  ( -4.289200894924355190, -5.876774720514414518, 19.85590024959437017 ) ) ;
#28670 = B_SPLINE_CURVE_WITH_KNOTS ( 'NONE', 3,
 ( #5985, #35939, #44555, #67400, #58293, #97341 ),
 .UNSPECIFIED., .F., .F.,
 ( 4, 2, 4 ),
 ( 0.000000000000000000, 0.001381510080715903652, 0.002763020161431807304 ),
 .UNSPECIFIED. ) ;
#28671 = CARTESIAN_POINT ( 'NONE',  ( -7.749999999999996447, 23.99999999999999289, 0.000000000000000000 ) ) ;
#28672 = CARTESIAN_POINT ( 'NONE',  ( 10.86264265030973952, -5.965225279485574461, -27.62597719988137612 ) ) ;
#28673 = CARTESIAN_POINT ( 'NONE',  ( -17.31707178780640533, -9.736581320607820444, -1.500000000000002220 ) ) ;
#28674 = PLANE ( 'NONE',  #4224 ) ;
#28675 = CARTESIAN_POINT ( 'NONE',  ( 16.85830656838225039, -10.38424343889589707, -1.500000000000002220 ) ) ;
#28676 = AXIS2_PLACEMENT_3D ( 'NONE', #41461, #59691, #27237 ) ;
#28677 = FACE_OUTER_BOUND ( 'NONE', #34058, .T. ) ;
#28678 = DIRECTION ( 'NONE',  ( 0.9913618264504693300, 5.365801633547217234E-16, -0.1311553622875920033 ) ) ;
#28679 = CARTESIAN_POINT ( 'NONE',  ( -1.304987980769231948, -6.376774720514413630, 19.76512419871795245 ) ) ;
#28680 = CARTESIAN_POINT ( 'NONE',  ( 9.361532043782798240, 18.45020211870636118, 11.49999999999999645 ) ) ;
#28681 = AXIS2_PLACEMENT_3D ( 'NONE', #40368, #25126, #56105 ) ;
#28682 = CARTESIAN_POINT ( 'NONE',  ( -99.16166289166535819, -25.30166215957521914, 5.311370747606397380 ) ) ;
#28683 = DIRECTION ( 'NONE',  ( 1.000000000000000000, 1.875376730785737473E-16, 0.000000000000000000 ) ) ;
#28684 = CARTESIAN_POINT ( 'NONE',  ( -50.37830952628071657, -25.31439277241203101, 5.197788989166616247 ) ) ;
#28685 = CARTESIAN_POINT ( 'NONE',  ( -17.38503614929206265, -14.63273120789127013, 11.49999999999999645 ) ) ;
#28686 = ORIENTED_EDGE ( 'NONE', *, *, #39215, .T. ) ;
#28687 = B_SPLINE_SURFACE_WITH_KNOTS ( 'NONE', 3, 3, ( 
 ( #63853, #72447, #27270, #25762 ),
 ( #64860, #89165, #50603, #33367 ),
 ( #81556, #94767, #87666, #66844 ),
 ( #51104, #4928, #12528, #43497 ),
 ( #13520, #35875, #74435, #97274 ),
 ( #20141, #35386, #82047, #59723 ),
 ( #51602, #67837, #82540, #13020 ) ),
 .UNSPECIFIED., .F., .F., .F.,
 ( 4, 3, 4 ),
 ( 4, 4 ),
 ( 0.7945040050992244751, 0.8970133687736503436, 0.9995227324480762121 ),
 ( 0.7296794188957508309, 0.7310290118914040125 ),
 .UNSPECIFIED. ) ;
#28688 = CARTESIAN_POINT ( 'NONE',  ( -46.62287095715004881, -24.66019654487198665, 8.947790411086135265 ) ) ;
#28690 = ADVANCED_FACE ( 'NONE', ( #7922 ), #17033, .T. ) ;
#28689 = CARTESIAN_POINT ( 'NONE',  ( 30.60441873609196151, 4.296715115238376015, 26.89749680779764773 ) ) ;
#28691 = ADVANCED_FACE ( 'NONE', ( #31765 ), #53620, .F. ) ;
#28692 = FACE_OUTER_BOUND ( 'NONE', #34454, .T. ) ;
#28693 = EDGE_CURVE ( 'NONE', #73934, #52090, #51029, .T. ) ;
#28694 = CARTESIAN_POINT ( 'NONE',  ( -93.62287095715005592, -23.48786465467241769, 11.44779295918254114 ) ) ;
#28695 = EDGE_CURVE ( 'NONE', #76406, #83129, #69235, .T. ) ;
#28696 = ORIENTED_EDGE ( 'NONE', *, *, #29493, .T. ) ;
#28697 = VECTOR ( 'NONE', #38368, 1000.000000000000000 ) ;
#28698 = ADVANCED_FACE ( 'NONE', ( #38372 ), #24144, .F. ) ;
#28699 = ORIENTED_EDGE ( 'NONE', *, *, #59191, .T. ) ;
#28700 = LINE ( 'NONE', #5359, #85756 ) ;
#28701 = B_SPLINE_CURVE_WITH_KNOTS ( 'NONE', 3,
 ( #28076, #59031, #60533, #35191, #74728, #5725, #52910, #45297, #67152, #98060, #28562, #91447, #13324, #43305, #75718, #90463 ),
 .UNSPECIFIED., .F., .F.,
 ( 4, 2, 2, 2, 2, 2, 2, 4 ),
 ( 0.000000000000000000, 0.0002615882740771409095, 0.0005231765481542818190, 0.001046353096308548242, 0.001307941370385681942, 0.001569529644462814991, 0.001831117918539948257, 0.002092706192617081306 ),
 .UNSPECIFIED. ) ;
#28702 = CARTESIAN_POINT ( 'NONE',  ( 21.14566350062385780, -8.679158401671109857, -1.500000000000002220 ) ) ;
#28703 = CARTESIAN_POINT ( 'NONE',  ( -29.54490261039654442, -24.07229224446866667, -0.2315648265717072385 ) ) ;
#28704 = CARTESIAN_POINT ( 'NONE',  ( -2.376235263977734657, 21.45616117177731041, -1.500000000000002220 ) ) ;
#28705 = CARTESIAN_POINT ( 'NONE',  ( -113.5517671225293128, -24.51419770103157347, 9.386484678747168076 ) ) ;
#28706 = DIRECTION ( 'NONE',  ( 1.000000000000000000, 0.000000000000000000, 0.000000000000000000 ) ) ;
#28707 = CARTESIAN_POINT ( 'NONE',  ( -10.21242994381667657, -20.12718729479640700, 11.49999999999999645 ) ) ;
#28708 = VERTEX_POINT ( 'NONE', #23130 ) ;
#28709 = DIRECTION ( 'NONE',  ( 0.000000000000000000, -2.173523156925980399E-06, 0.9999999999976378895 ) ) ;
#28710 = CARTESIAN_POINT ( 'NONE',  ( -6.321128248299066499, 21.05883132939252533, -1.500000000000002220 ) ) ;
#28711 = VECTOR ( 'NONE', #1875, 1000.000000000000000 ) ;
#28712 = CARTESIAN_POINT ( 'NONE',  ( -105.5100248002994050, -24.73531770709095312, 8.716586749053508498 ) ) ;
#28713 = CARTESIAN_POINT ( 'NONE',  ( -28.09930172958063466, -24.79700303329384425, 7.540558023410448563 ) ) ;
#28714 = ORIENTED_EDGE ( 'NONE', *, *, #47939, .T. ) ;
#28715 = CARTESIAN_POINT ( 'NONE',  ( -89.62287095715008434, -23.73934037231757799, 11.05740245334328797 ) ) ;
#28716 = CARTESIAN_POINT ( 'NONE',  ( -90.63102145325892423, -24.52399227489127398, 9.353111116836531735 ) ) ;
#28717 = ORIENTED_EDGE ( 'NONE', *, *, #39910, .T. ) ;
#28718 = CARTESIAN_POINT ( 'NONE',  ( -5.366453405989236813, 1.999999999999998224, 19.19609335255483984 ) ) ;
#28719 = VERTEX_POINT ( 'NONE', #68832 ) ;
#28720 = AXIS2_PLACEMENT_3D ( 'NONE', #86659, #87162, #80050 ) ;
#28721 = ORIENTED_EDGE ( 'NONE', *, *, #1798, .T. ) ;
#28722 = CARTESIAN_POINT ( 'NONE',  ( -49.28021062419514919, -25.26817783364414183, 6.077668871661954242 ) ) ;
#28723 = CARTESIAN_POINT ( 'NONE',  ( 3.750000000000001776, 26.59999999999999432, 2.100000000000000089 ) ) ;
#28724 = CARTESIAN_POINT ( 'NONE',  ( -57.58284588185660624, -24.51314013834315375, 0.6176544820404114011 ) ) ;
#28725 = CARTESIAN_POINT ( 'NONE',  ( 2.691128592823461840, 20.25793168094256202, -1.500000000000002220 ) ) ;
#28726 = ADVANCED_FACE ( 'NONE', ( #92153 ), #85542, .T. ) ;
#28727 = VERTEX_POINT ( 'NONE', #77418 ) ;
#28728 = FACE_OUTER_BOUND ( 'NONE', #62862, .T. ) ;
#28729 = CARTESIAN_POINT ( 'NONE',  ( -30.59326697242301663, -24.88273649812090227, 8.549170486301877148 ) ) ;
#28730 = CARTESIAN_POINT ( 'NONE',  ( -105.6382416112896436, -23.48783264082477018, -1.443836473390094355 ) ) ;
#28731 = CARTESIAN_POINT ( 'NONE',  ( -7.160000000000000142, 10.80195425911416507, -0.9450485415980990345 ) ) ;
#28732 = EDGE_CURVE ( 'NONE', #95160, #66603, #88593, .T. ) ;
#28733 = EDGE_LOOP ( 'NONE', ( #8839, #84296, #61987 ) ) ;
#28734 = FACE_OUTER_BOUND ( 'NONE', #83776, .T. ) ;
#28735 = CARTESIAN_POINT ( 'NONE',  ( -94.62287095715005592, -23.47593901973091235, -1.443836447539002865 ) ) ;
#28736 = CARTESIAN_POINT ( 'NONE',  ( 2.677173591928626806, -20.63698567995287902, 11.49999999999998934 ) ) ;
#28737 = ORIENTED_EDGE ( 'NONE', *, *, #73971, .F. ) ;
#28739 = ORIENTED_EDGE ( 'NONE', *, *, #13134, .F. ) ;
#28738 = LINE ( 'NONE', #59699, #73405 ) ;
#28740 = DIRECTION ( 'NONE',  ( 0.000000000000000000, 0.9999999999976377785, 2.173523156925979975E-06 ) ) ;
#28741 = CARTESIAN_POINT ( 'NONE',  ( -129.5217890828018312, -24.66019654487200086, 8.947790411086113949 ) ) ;
#28742 = ORIENTED_EDGE ( 'NONE', *, *, #17690, .F. ) ;
#28743 = ORIENTED_EDGE ( 'NONE', *, *, #64240, .T. ) ;
#28744 = DIRECTION ( 'NONE',  ( 0.000000000000000000, 0.000000000000000000, -1.000000000000000000 ) ) ;
#28745 = DIRECTION ( 'NONE',  ( -1.000000000000000000, -0.000000000000000000, -0.000000000000000000 ) ) ;
#28746 = CARTESIAN_POINT ( 'NONE',  ( -109.5228709571500616, -24.64898659630530275, 1.056161002820831474 ) ) ;
#28747 = CARTESIAN_POINT ( 'NONE',  ( -71.29000553066028090, -25.24515197902177022, 6.029837115414142801 ) ) ;
#28749 = ORIENTED_EDGE ( 'NONE', *, *, #97337, .T. ) ;
#28748 = CARTESIAN_POINT ( 'NONE',  ( -19.76278938440450617, -9.944092408650034187, 11.49999999999999645 ) ) ;
#28750 = CARTESIAN_POINT ( 'NONE',  ( -75.52287095715006160, -29.50249982740957577, 7.747779886224967605 ) ) ;
#28751 = CARTESIAN_POINT ( 'NONE',  ( 12.73759380600583846, -18.68238426224762350, -1.500000000000002220 ) ) ;
#28752 = AXIS2_PLACEMENT_3D ( 'NONE', #20006, #42865, #43361 ) ;
#28753 = EDGE_CURVE ( 'NONE', #92012, #27790, #43841, .T. ) ;
#28755 = VERTEX_POINT ( 'NONE', #77916 ) ;
#28754 = CARTESIAN_POINT ( 'NONE',  ( -115.5883522698519954, -24.73531770709096023, 8.716586749053508498 ) ) ;
#28756 = ORIENTED_EDGE ( 'NONE', *, *, #8646, .T. ) ;
#28757 = VECTOR ( 'NONE', #45505, 1000.000000000000000 ) ;
#28758 = DIRECTION ( 'NONE',  ( 0.000000000000000000, 1.000000000000000000, 0.000000000000000000 ) ) ;
#28759 = ADVANCED_FACE ( 'NONE', ( #47495, #46491, #46993 ), #813, .T. ) ;
#28760 = CARTESIAN_POINT ( 'NONE',  ( -7.807601069497579260, -18.53474111305376937, 11.49999999999998934 ) ) ;
#28761 = CARTESIAN_POINT ( 'NONE',  ( 27.53860345374771867, -500000.0000000000582, -9.482392034746242260 ) ) ;
#28762 = ORIENTED_EDGE ( 'NONE', *, *, #91146, .F. ) ;
#28763 = CARTESIAN_POINT ( 'NONE',  ( -40.09822460666767086, -25.30507952954706852, 5.519450557857781270 ) ) ;
#28764 = CARTESIAN_POINT ( 'NONE',  ( -17.00426676922356606, 14.40147940013276973, -1.500000000000002220 ) ) ;
#28765 = CARTESIAN_POINT ( 'NONE',  ( -50.40895856474225667, -25.03220906767835885, 7.563174217889635287 ) ) ;
#28766 = ORIENTED_EDGE ( 'NONE', *, *, #70865, .F. ) ;
#28767 = CARTESIAN_POINT ( 'NONE',  ( -110.5228709571500616, -23.48786465467242479, 11.44779295918253936 ) ) ;
#28768 = FACE_OUTER_BOUND ( 'NONE', #4245, .T. ) ;
#28769 = CARTESIAN_POINT ( 'NONE',  ( -109.8650282762807393, -29.50249556043354460, 5.784618828537300139 ) ) ;
#28770 = AXIS2_PLACEMENT_3D ( 'NONE', #94290, #86186, #17170 ) ;
#28771 = DIRECTION ( 'NONE',  ( 0.5661055431922977776, 0.000000000000000000, -0.8243327689513219036 ) ) ;
#28772 = FACE_OUTER_BOUND ( 'NONE', #4903, .T. ) ;
#28773 = CARTESIAN_POINT ( 'NONE',  ( -6.230579426152004885, -18.48807627814308674, -1.500000000000002220 ) ) ;
#28774 = CARTESIAN_POINT ( 'NONE',  ( -19.33005188562793819, 9.364626179424670127, -1.500000000000002220 ) ) ;
#28775 = CARTESIAN_POINT ( 'NONE',  ( -2.656471864501908975, -5.876774720514410077, 19.66116880005639800 ) ) ;
#28776 = LINE ( 'NONE', #21150, #48126 ) ;
#28777 = CARTESIAN_POINT ( 'NONE',  ( -50.38822539166533687, -29.50249328176098729, 4.736241424693623081 ) ) ;
#28778 = CARTESIAN_POINT ( 'NONE',  ( 6.015242202445381992, 21.98585358372262633, -1.500000000000002220 ) ) ;
#28779 = AXIS2_PLACEMENT_3D ( 'NONE', #55196, #100321, #71411 ) ;
#28780 = CALENDAR_DATE ( 2026, 9, 10 ) ;
#28781 = CARTESIAN_POINT ( 'NONE',  ( -39.52287095715007581, -23.94994826722565406, -0.6494450866342755813 ) ) ;
#28782 = DIRECTION ( 'NONE',  ( -3.773278334453080206E-23, 0.9999999999976377785, 2.173523156925979552E-06 ) ) ;
#28783 = CARTESIAN_POINT ( 'NONE',  ( 7.431233518514567926, -18.57414813805618081, 11.49999999999999645 ) ) ;
#28784 = CARTESIAN_POINT ( 'NONE',  ( -24.55517127435777525, -0.3587747205143967943, -15.44180958690143157 ) ) ;
#28785 = AXIS2_PLACEMENT_3D ( 'NONE', #42758, #73691, #49877 ) ;
#28786 = CARTESIAN_POINT ( 'NONE',  ( -123.6228709571500701, -23.94994826722515668, -0.6494450866351689777 ) ) ;
#28787 = DIRECTION ( 'NONE',  ( -0.000000000000000000, -0.000000000000000000, -1.000000000000000000 ) ) ;
#28788 = ORIENTED_EDGE ( 'NONE', *, *, #8472, .T. ) ;
#28789 = CARTESIAN_POINT ( 'NONE',  ( 9.450000000000002842, -2.000000000000001332, 19.19609335255483629 ) ) ;
#28790 = PLANE ( 'NONE',  #24765 ) ;
#28791 = CARTESIAN_POINT ( 'NONE',  ( 14.84582651547613352, 15.88809324551894520, -1.500000000000002220 ) ) ;
#28792 = DIRECTION ( 'NONE',  ( -0.2164396139380966033, 0.9762960071199348056, 0.000000000000000000 ) ) ;
#28793 = CARTESIAN_POINT ( 'NONE',  ( 16.73968668634701729, 10.17700309559984717, -1.500000000000002220 ) ) ;
#28794 = CARTESIAN_POINT ( 'NONE',  ( -99.71650429754699019, -25.16638005418298718, 6.902600843980934542 ) ) ;
#28795 = ORIENTED_EDGE ( 'NONE', *, *, #91456, .F. ) ;
#28796 = DATE_TIME_ROLE ( 'classification_date' ) ;
#28797 = CARTESIAN_POINT ( 'NONE',  ( -60.62287095715006302, -24.15516710230295416, 10.28746687063727272 ) ) ;
#28798 = DIRECTION ( 'NONE',  ( -0.000000000000000000, -1.000000000000000000, -0.000000000000000000 ) ) ;
#28799 = CARTESIAN_POINT ( 'NONE',  ( -10.66544979547405347, 17.54311462378693420, 11.49999999999999645 ) ) ;
#28800 = CARTESIAN_POINT ( 'NONE',  ( -93.62287095715005592, -29.50250243563736774, 8.947779886222139822 ) ) ;
#28801 = PLANE ( 'NONE',  #72418 ) ;
#28802 = VERTEX_POINT ( 'NONE', #94152 ) ;
#28803 = CARTESIAN_POINT ( 'NONE',  ( 31.35973677934181936, -4.378374783736292741, 0.3342810658314839256 ) ) ;
#28804 = CARTESIAN_POINT ( 'NONE',  ( -43.55620429048340014, -24.66019654487199020, 8.947790411086137041 ) ) ;
#28806 = ADVANCED_FACE ( 'NONE', ( #24638 ), #55618, .F. ) ;
#28805 = CARTESIAN_POINT ( 'NONE',  ( -110.6228709571500559, -29.50249982740957577, 7.747779886224967605 ) ) ;
#28807 = CARTESIAN_POINT ( 'NONE',  ( 22.02124265030973760, -6.376774720514428729, 16.20402280011862217 ) ) ;
#28809 = ORIENTED_EDGE ( 'NONE', *, *, #28043, .T. ) ;
#28808 = EDGE_CURVE ( 'NONE', #75490, #71750, #96171, .T. ) ;
#28810 = PLANE ( 'NONE',  #67418 ) ;
#28811 = AXIS2_PLACEMENT_3D ( 'NONE', #76760, #99599, #53464 ) ;
#28812 = EDGE_CURVE ( 'NONE', #23301, #41495, #40382, .T. ) ;
#28813 = B_SPLINE_CURVE_WITH_KNOTS ( 'NONE', 3,
 ( #10952, #42911, #4346, #20057 ),
 .UNSPECIFIED., .F., .F.,
 ( 4, 4 ),
 ( 0.000000000000000000, 9.999999999998897304E-05 ),
 .UNSPECIFIED. ) ;
#28814 = CARTESIAN_POINT ( 'NONE',  ( -8.820007276677138464, 21.28423624206370945, 11.49999999999999645 ) ) ;
#28815 = CARTESIAN_POINT ( 'NONE',  ( -18.67006117854901959, 13.05921059288911934, -1.500000000000002220 ) ) ;
#28816 = CARTESIAN_POINT ( 'NONE',  ( -70.50669286463424612, -25.30458798213071248, 4.857674088053123285 ) ) ;
#28817 = B_SPLINE_SURFACE_WITH_KNOTS ( 'NONE', 3, 3, ( 
 ( #67771, #60655, #83969, #20074 ),
 ( #53038, #37800, #29685, #97698 ),
 ( #99669, #35808, #6843, #30174 ),
 ( #20567, #89592, #36806, #12951 ),
 ( #13452, #76343, #68752, #52530 ),
 ( #43432, #74363, #83464, #51538 ),
 ( #44928, #59656, #6350, #75850 ) ),
 .UNSPECIFIED., .F., .F., .F.,
 ( 4, 3, 4 ),
 ( 4, 4 ),
 ( 0.0004766839783818343059, 0.1029713700210893729, 0.2054660560637969202 ),
 ( 0.6696643484175435201, 0.6709860548734745134 ),
 .UNSPECIFIED. ) ;
#28818 = EDGE_CURVE ( 'NONE', #56886, #13066, #48504, .T. ) ;
#28819 = LINE ( 'NONE', #92697, #23618 ) ;
#28820 = DIRECTION ( 'NONE',  ( 0.000000000000000000, -0.9999999999976377785, -2.173523156925979975E-06 ) ) ;
#28821 = CARTESIAN_POINT ( 'NONE',  ( 2.499999999999995115, 19.99999999999999645, 2.100000000000000089 ) ) ;
#28822 = EDGE_CURVE ( 'NONE', #38937, #76505, #34144, .T. ) ;
#28823 = CARTESIAN_POINT ( 'NONE',  ( -110.6235417928964040, -25.00158670708910336, 2.256160236439218814 ) ) ;
#28824 = CARTESIAN_POINT ( 'NONE',  ( -17.52905966558703454, -13.16386835867055716, -1.500000000000002220 ) ) ;
#28825 = CARTESIAN_POINT ( 'NONE',  ( 7.072045900997899537, -5.876774720514426953, 21.62824307385093192 ) ) ;
#28826 = PLANE ( 'NONE',  #46297 ) ;
#28827 = CARTESIAN_POINT ( 'NONE',  ( -40.91416358624242378, -25.31564009351394162, 4.986335130569790053 ) ) ;
#28828 = CARTESIAN_POINT ( 'NONE',  ( 9.383883476483161346, 17.86611652351680846, 2.100000000000000089 ) ) ;
#28829 = LINE ( 'NONE', #99809, #71154 ) ;
#28830 = CARTESIAN_POINT ( 'NONE',  ( -60.91704107235849364, -25.28799268357646568, 6.054714359087114417 ) ) ;
#28831 = VERTEX_POINT ( 'NONE', #49003 ) ;
#28832 = PRODUCT ( 'oval head_am_B18.6.7M - M2.5 x 0.45 x 20 Type I Cross Recessed OHMS --20C', 'oval head_am_B18.6.7M - M2.5 x 0.45 x 20 Type I Cross Recessed OHMS --20C', '', ( #46012 ) ) ;
#28833 = CARTESIAN_POINT ( 'NONE',  ( 10.78675619948152864, -17.38023510967517637, 11.49999999999998934 ) ) ;
#28834 = ORIENTED_EDGE ( 'NONE', *, *, #49725, .F. ) ;
#28835 = ORIENTED_EDGE ( 'NONE', *, *, #98908, .T. ) ;
#28836 = ORIENTED_EDGE ( 'NONE', *, *, #37859, .F. ) ;
#28837 = ORIENTED_EDGE ( 'NONE', *, *, #1964, .F. ) ;
#28838 = CARTESIAN_POINT ( 'NONE',  ( 22.66633601775066253, -4.223608244049824378, -1.500000000000002220 ) ) ;
#28839 = CARTESIAN_POINT ( 'NONE',  ( -61.62757367957146926, -24.51314013834316441, 0.6176544820404165081 ) ) ;
#28840 = CARTESIAN_POINT ( 'NONE',  ( -16.41926757845921614, -11.79510067912178606, -1.500000000000002220 ) ) ;
#28841 = ORIENTED_EDGE ( 'NONE', *, *, #56811, .F. ) ;
#28842 = CARTESIAN_POINT ( 'NONE',  ( -28.21458010398708893, -24.83337313992710449, 7.636915180611340226 ) ) ;
#28843 = VECTOR ( 'NONE', #33271, 1000.000000000000000 ) ;
#28844 = CARTESIAN_POINT ( 'NONE',  ( -40.84751817244628569, -25.30517900822009736, 5.505870246111851607 ) ) ;
#28845 = EDGE_CURVE ( 'NONE', #70766, #31222, #99989, .T. ) ;
#28846 = B_SPLINE_CURVE_WITH_KNOTS ( 'NONE', 3,
 ( #28054, #12806, #75210, #98539 ),
 .UNSPECIFIED., .F., .F.,
 ( 4, 4 ),
 ( 0.000000000000000000, 0.0001000000000000028644 ),
 .UNSPECIFIED. ) ;
#28847 = PLANE ( 'NONE',  #83714 ) ;
#28848 = CARTESIAN_POINT ( 'NONE',  ( -99.50978007678189385, -24.51419770103158413, 9.386484678747176957 ) ) ;
#28850 = EDGE_LOOP ( 'NONE', ( #38805, #46342, #64899, #65008 ) ) ;
#28849 = CARTESIAN_POINT ( 'NONE',  ( 1.185105815240312888, -21.37944065014308848, 11.49999999999999645 ) ) ;
#28851 = CARTESIAN_POINT ( 'NONE',  ( -77.55620429048339304, -23.48783264082478084, -1.443836473390065933 ) ) ;
#28852 = ORIENTED_EDGE ( 'NONE', *, *, #15059, .T. ) ;
#28853 = CARTESIAN_POINT ( 'NONE',  ( -19.59449498831206782, -6.737714454370689054, 11.49999999999998934 ) ) ;
#28854 = AXIS2_PLACEMENT_3D ( 'NONE', #32084, #63060, #68661 ) ;
#28855 = EDGE_LOOP ( 'NONE', ( #41857, #17765, #36330, #37223, #79399 ) ) ;
#28856 = LINE ( 'NONE', #91741, #12959 ) ;
#28857 = ORIENTED_EDGE ( 'NONE', *, *, #42201, .F. ) ;
#28858 = DIRECTION ( 'NONE',  ( 0.000000000000000000, 1.000000000000000000, 0.000000000000000000 ) ) ;
#28859 = AXIS2_PLACEMENT_3D ( 'NONE', #50784, #49797, #27447 ) ;
#28860 = ORIENTED_EDGE ( 'NONE', *, *, #1818, .F. ) ;
#28861 = B_SPLINE_CURVE_WITH_KNOTS ( 'NONE', 3,
 ( #80917, #82407, #42382, #43860 ),
 .UNSPECIFIED., .F., .F.,
 ( 4, 4 ),
 ( 0.000000000000000000, 0.0001000000000000028644 ),
 .UNSPECIFIED. ) ;
#28862 = CARTESIAN_POINT ( 'NONE',  ( -15.31302551872622075, -14.39686070098267479, -1.500000000000002220 ) ) ;
#28863 = CARTESIAN_POINT ( 'NONE',  ( -21.26704322615652032, -5.532269525099344776, 11.49999999999999645 ) ) ;
#28864 = CARTESIAN_POINT ( 'NONE',  ( -37.58093832661909772, -24.51419770103156637, 9.386484678747175181 ) ) ;
#28865 = CARTESIAN_POINT ( 'NONE',  ( -21.23328875057882570, -7.520457577684837247, -1.500000000000002220 ) ) ;
#28866 = CARTESIAN_POINT ( 'NONE',  ( -8.441512789788195192, 19.21024974253229800, -1.500000000000002220 ) ) ;
#28867 = CARTESIAN_POINT ( 'NONE',  ( 5.697397333356354565, -5.876774720514418071, 20.51730809691671809 ) ) ;
#28868 = CARTESIAN_POINT ( 'NONE',  ( -72.62287095715004170, -23.94994826722515313, -0.6494450866351729745 ) ) ;
#28869 = PLANE ( 'NONE',  #34602 ) ;
#28870 = ORIENTED_EDGE ( 'NONE', *, *, #97028, .F. ) ;
#28871 = ORIENTED_EDGE ( 'NONE', *, *, #24832, .F. ) ;
#28872 = EDGE_LOOP ( 'NONE', ( #10899, #33909, #3032, #97501 ) ) ;
#28873 = CARTESIAN_POINT ( 'NONE',  ( -124.6228709571500701, -23.47596703998600631, 11.44779298504227860 ) ) ;
#28874 = CARTESIAN_POINT ( 'NONE',  ( 21.23773461148298836, -3.020459416520930862, -1.500000000000002220 ) ) ;
#28875 = EDGE_CURVE ( 'NONE', #39863, #76643, #84978, .T. ) ;
#28876 = CARTESIAN_POINT ( 'NONE',  ( -105.5228709571500474, -24.91570333825769623, 8.075032458260368529 ) ) ;
#28877 = ORIENTED_EDGE ( 'NONE', *, *, #99, .T. ) ;
#28878 = CARTESIAN_POINT ( 'NONE',  ( -12.37649675270136918, 17.12833386298736471, -1.500000000000002220 ) ) ;
#28879 = CARTESIAN_POINT ( 'NONE',  ( -52.62287095715004170, -23.47596703998600276, 11.44779298504227505 ) ) ;
#28880 = CARTESIAN_POINT ( 'NONE',  ( -64.63158557479336253, -24.34968618360933590, 0.1864209137778785330 ) ) ;
#28881 = CARTESIAN_POINT ( 'NONE',  ( -83.54431499582896947, -24.51419770103157347, 9.386484678747180510 ) ) ;
#28882 = DIRECTION ( 'NONE',  ( -1.000000000000000000, -3.773278334444167608E-23, -8.201307833595939069E-29 ) ) ;
#28883 = CARTESIAN_POINT ( 'NONE',  ( -0.5830141525297981575, -5.876774720514410077, 19.15054976246387497 ) ) ;
#28884 = CARTESIAN_POINT ( 'NONE',  ( 21.80885565983754404, 3.581153529568561478, -1.500000000000002220 ) ) ;
#28885 = CARTESIAN_POINT ( 'NONE',  ( -30.47961041733904608, -23.47593902323810156, -1.442222850822345581 ) ) ;
#28886 = EDGE_CURVE ( 'NONE', #86024, #35233, #6263, .T. ) ;
#28887 = CARTESIAN_POINT ( 'NONE',  ( -109.0882301073077514, -25.30385130285613471, 4.785588035035526211 ) ) ;
#28888 = CARTESIAN_POINT ( 'NONE',  ( 12.17309066428871667, 5.143895418987112222, -26.49515656621686333 ) ) ;
#28889 = LINE ( 'NONE', #14656, #6376 ) ;
#28890 = DIRECTION ( 'NONE',  ( -1.655121434032223174E-15, 1.000000000000000000, 0.000000000000000000 ) ) ;
#28891 = CARTESIAN_POINT ( 'NONE',  ( -16.21482014894483470, 10.69450053600103345, 11.49999999999998934 ) ) ;
#28892 = CARTESIAN_POINT ( 'NONE',  ( -20.51402961445061734, 6.013860829077147585, 11.49999999999998934 ) ) ;
#28893 = CARTESIAN_POINT ( 'NONE',  ( -66.62287095715005592, -23.48783264082478439, -1.443836473390067487 ) ) ;
#28894 = CARTESIAN_POINT ( 'NONE',  ( -85.62287095715004170, -24.99156045073393173, 7.747789690856161648 ) ) ;
#28895 = LINE ( 'NONE', #45628, #9794 ) ;
#28896 = DIRECTION ( 'NONE',  ( 3.469446951953611033E-15, 1.000000000000000000, 0.000000000000000000 ) ) ;
#28897 = APPROVAL ( #4478, 'UNSPECIFIED' ) ;
#28898 = CARTESIAN_POINT ( 'NONE',  ( 0.4201012023153268271, 22.63755686032812164, -1.500000000000002220 ) ) ;
#28899 = B_SPLINE_SURFACE_WITH_KNOTS ( 'NONE', 3, 3, ( 
 ( #91400, #14271, #20888, #60974 ),
 ( #13770, #13276, #36624, #75669 ),
 ( #67102, #30002, #6171, #21380 ),
 ( #7166, #52358, #75179, #45245 ),
 ( #6668, #38115, #51864, #5674 ),
 ( #91899, #22376, #53361, #21877 ),
 ( #5177, #76170, #76661, #61475 ) ),
 .UNSPECIFIED., .F., .F., .F.,
 ( 4, 3, 4 ),
 ( 4, 4 ),
 ( 0.0004766839783832283730, 0.1029713700210899835, 0.2054660560637967259 ),
 ( 0.9697406827104064764, 0.9712008438356087847 ),
 .UNSPECIFIED. ) ;
#28900 = EDGE_LOOP ( 'NONE', ( #77105, #86356, #77388, #59576 ) ) ;
#28901 = CARTESIAN_POINT ( 'NONE',  ( -4.141025641025640525, -6.376774720514418959, 20.67377804487179915 ) ) ;
#28902 = CARTESIAN_POINT ( 'NONE',  ( -97.58953762381671027, -24.64898659630367916, 1.056161002820388717 ) ) ;
#28903 = CARTESIAN_POINT ( 'NONE',  ( 19.75791096855702733, 1.210928449428283038, 11.49999999999999645 ) ) ;
#28904 = CARTESIAN_POINT ( 'NONE',  ( -82.62287095715004170, -24.33927499327854704, 9.819080762295817166 ) ) ;
#28905 = CARTESIAN_POINT ( 'NONE',  ( -119.5895376238167103, -24.66019654487200086, 8.947790411086115725 ) ) ;
#28906 = ORIENTED_EDGE ( 'NONE', *, *, #94937, .F. ) ;
#28907 = CARTESIAN_POINT ( 'NONE',  ( 15.32643653063177958, -2.682774720514426559, -27.14485409495429380 ) ) ;
#28908 = CARTESIAN_POINT ( 'NONE',  ( -29.66447556523817397, -25.26026669889196086, 3.393817555207442105 ) ) ;
#28909 = LINE ( 'NONE', #89318, #86904 ) ;
#28910 = CARTESIAN_POINT ( 'NONE',  ( -2.642555958445479192, -21.45212208726272607, -1.500000000000002220 ) ) ;
#28911 = CARTESIAN_POINT ( 'NONE',  ( -99.62287095715008434, -23.73907113216991860, -1.053371485793223927 ) ) ;
#28912 = VECTOR ( 'NONE', #24668, 1000.000000000000000 ) ;
#28913 = CARTESIAN_POINT ( 'NONE',  ( -66.52287095715003318, -24.35013146730204170, 9.818937971375099494 ) ) ;
#28914 = CARTESIAN_POINT ( 'NONE',  ( 32.66876533700882845, -5.965225279485572685, -12.58926540598385557 ) ) ;
#28915 = CARTESIAN_POINT ( 'NONE',  ( -35.62287095715004170, -23.85196035786900737, -0.8779234886474999167 ) ) ;
#28916 = CARTESIAN_POINT ( 'NONE',  ( -8.418173371947181849, -17.93405594323863284, 11.49999999999998934 ) ) ;
#28917 = EDGE_LOOP ( 'NONE', ( #94655, #36368, #7535, #47069 ) ) ;
#28918 = CARTESIAN_POINT ( 'NONE',  ( 15.61528876134825161, -13.05345633644532732, 11.49999999999999645 ) ) ;
#28919 = DIRECTION ( 'NONE',  ( 0.1478094111296165969, -0.9890158633619159367, 0.000000000000000000 ) ) ;
#28920 = DIRECTION ( 'NONE',  ( -3.773278334453079618E-23, 0.9999999999976377785, 2.173523156925979975E-06 ) ) ;
#28921 = ORIENTED_EDGE ( 'NONE', *, *, #25756, .T. ) ;
#28922 = CARTESIAN_POINT ( 'NONE',  ( -102.5930986047791151, -23.96169478059713498, 10.65365249895717881 ) ) ;
#28923 = CARTESIAN_POINT ( 'NONE',  ( -111.6468792378192063, -25.29712067403330877, 4.332404411321261861 ) ) ;
#28924 = FACE_OUTER_BOUND ( 'NONE', #235, .T. ) ;
#28925 = CIRCLE ( 'NONE', #25749, 252.4458649670781085 ) ;
#28926 = DIRECTION ( 'NONE',  ( 0.3133898629642186684, -7.885106708985488048E-16, -0.9496245541219267006 ) ) ;
#28927 = CARTESIAN_POINT ( 'NONE',  ( -48.62287095715004881, -23.47596703998600276, 11.44779298504227505 ) ) ;
#28928 = CARTESIAN_POINT ( 'NONE',  ( -16.72505113720834657, 11.10480813184383742, -1.500000000000002220 ) ) ;
#28929 = PLANE ( 'NONE',  #40230 ) ;
#28930 = ORIENTED_EDGE ( 'NONE', *, *, #43090, .F. ) ;
#28931 = B_SPLINE_CURVE_WITH_KNOTS ( 'NONE', 3,
 ( #97343, #80617, #73021, #12599, #89233, #26832 ),
 .UNSPECIFIED., .F., .F.,
 ( 4, 2, 4 ),
 ( 0.000000000000000000, 0.5000000000000000000, 1.000000000000000000 ),
 .UNSPECIFIED. ) ;
#28932 = FACE_OUTER_BOUND ( 'NONE', #36599, .T. ) ;
#28933 = VECTOR ( 'NONE', #87967, 1000.000000000000114 ) ;
#28934 = CARTESIAN_POINT ( 'NONE',  ( 19.70479270790718829, 11.56945388388114360, 11.49999999999999645 ) ) ;
#28935 = CARTESIAN_POINT ( 'NONE',  ( -30.47287095715005734, -24.90571414232896785, 1.932341227645357318 ) ) ;
#28936 = EDGE_CURVE ( 'NONE', #43843, #47644, #87047, .T. ) ;
#28937 = DIRECTION ( 'NONE',  ( 0.000000000000000000, -0.9999999999976377785, -2.173523156925979975E-06 ) ) ;
#28938 = CARTESIAN_POINT ( 'NONE',  ( -10.34999999999999432, 3.499999999999998668, 0.000000000000000000 ) ) ;
#28939 = EDGE_CURVE ( 'NONE', #95847, #90525, #9417, .T. ) ;
#28940 = LINE ( 'NONE', #38048, #5957 ) ;
#28941 = CARTESIAN_POINT ( 'NONE',  ( -66.52287095715006160, -29.50250243563736774, 8.947779886222143375 ) ) ;
#28942 = PLANE ( 'NONE',  #69555 ) ;
#28943 = VERTEX_POINT ( 'NONE', #88558 ) ;
#28944 = CARTESIAN_POINT ( 'NONE',  ( 10.94010344783756672, -17.16519937159427656, -1.500000000000002220 ) ) ;
#28945 = VERTEX_POINT ( 'NONE', #78925 ) ;
#28946 = EDGE_CURVE ( 'NONE', #37803, #82227, #19033, .T. ) ;
#28947 = CARTESIAN_POINT ( 'NONE',  ( 4.748521865011817944, 22.44708532425888592, -1.500000000000002220 ) ) ;
#28948 = CARTESIAN_POINT ( 'NONE',  ( 5.514125806255895004E-17, -29.50248528299875161, 1.056150778585261296 ) ) ;
#28949 = EDGE_LOOP ( 'NONE', ( #68400, #18381, #96037, #53203 ) ) ;
#28950 = PLANE ( 'NONE',  #36403 ) ;
#28951 = CARTESIAN_POINT ( 'NONE',  ( -77.58808754410065944, -24.35071581493544102, 9.817618358456021710 ) ) ;
#28952 = CARTESIAN_POINT ( 'NONE',  ( 32.16024265030974050, -0.3587747205144265483, 16.27760796525321751 ) ) ;
#28954 = ORIENTED_EDGE ( 'NONE', *, *, #89653, .F. ) ;
#28953 = CARTESIAN_POINT ( 'NONE',  ( -18.72683625574626376, -10.08736549105613278, 11.49999999999999645 ) ) ;
#28955 = ORIENTED_EDGE ( 'NONE', *, *, #21794, .T. ) ;
#28956 = CARTESIAN_POINT ( 'NONE',  ( -10.56713949322891999, -19.48831581008217384, 11.49999999999998934 ) ) ;
#28957 = CARTESIAN_POINT ( 'NONE',  ( -18.82610421443283499, -8.410905081555696938, -1.500000000000002220 ) ) ;
#28958 = VERTEX_POINT ( 'NONE', #50007 ) ;
#28959 = ORIENTED_EDGE ( 'NONE', *, *, #54883, .T. ) ;
#28960 = CARTESIAN_POINT ( 'NONE',  ( -64.52287095715006160, -23.47596703998600631, 11.44779298504228926 ) ) ;
#28961 = CARTESIAN_POINT ( 'NONE',  ( -39.51069479889651603, -25.17639606163672283, 3.166201134751521540 ) ) ;
#28962 = ORIENTED_EDGE ( 'NONE', *, *, #27688, .F. ) ;
#28963 = AXIS2_PLACEMENT_3D ( 'NONE', #58233, #74920, #90658 ) ;
#28964 = VERTEX_POINT ( 'NONE', #10930 ) ;
#28965 = LINE ( 'NONE', #90866, #63249 ) ;
#28966 = CARTESIAN_POINT ( 'NONE',  ( -75.62287095715005592, -23.84081130438200802, 10.88220057463249013 ) ) ;
#28967 = CARTESIAN_POINT ( 'NONE',  ( -83.52287095715006160, -23.47593901973090524, -1.443836447538996648 ) ) ;
#28968 = CARTESIAN_POINT ( 'NONE',  ( 20.09396958936853395, 5.161349618257207617, -1.500000000000002220 ) ) ;
#28969 = CARTESIAN_POINT ( 'NONE',  ( -14.02725853290852243, 16.66567569088042688, 11.49999999999999645 ) ) ;
#28970 = CARTESIAN_POINT ( 'NONE',  ( -35.62287095715005592, -29.50249982740957577, 7.747779886224967605 ) ) ;
#28971 = CARTESIAN_POINT ( 'NONE',  ( -2.499999999999993339, 19.99999999999999645, 2.100000000000000089 ) ) ;
#28972 = CARTESIAN_POINT ( 'NONE',  ( -115.5868014046007204, -25.00158670708910691, 2.256160236439219258 ) ) ;
#28973 = CARTESIAN_POINT ( 'NONE',  ( -22.41777205227948855, 0.6913007675000180097, -1.500000000000002220 ) ) ;
#28974 = AXIS2_PLACEMENT_3D ( 'NONE', #86630, #31852, #24229 ) ;
#28975 = DIRECTION ( 'NONE',  ( -0.000000000000000000, 1.000000000000000000, -0.000000000000000000 ) ) ;
#28977 = EDGE_CURVE ( 'NONE', #86861, #79629, #15773, .T. ) ;
#28976 = ORIENTED_EDGE ( 'NONE', *, *, #82307, .F. ) ;
#28978 = DIRECTION ( 'NONE',  ( -3.773278334453079618E-23, 0.9999999999976377785, 2.173523156925979975E-06 ) ) ;
#28979 = CARTESIAN_POINT ( 'NONE',  ( -50.70524595056228634, -25.11617103263561290, 2.864784757501792622 ) ) ;
#28980 = ORIENTED_EDGE ( 'NONE', *, *, #99098, .F. ) ;
#28981 = AXIS2_PLACEMENT_3D ( 'NONE', #56411, #43047, #87330 ) ;
#28982 = ORIENTED_EDGE ( 'NONE', *, *, #20555, .T. ) ;
#28983 = CARTESIAN_POINT ( 'NONE',  ( -99.30784767537812741, -25.27538107857485272, 5.993649293344923912 ) ) ;
#28984 = EDGE_CURVE ( 'NONE', #61594, #73153, #20814, .T. ) ;
#28985 = EDGE_LOOP ( 'NONE', ( #19993, #53682, #1806, #84738 ) ) ;
#28986 = CARTESIAN_POINT ( 'NONE',  ( -12.14505723179402530, 17.47690347785001919, -1.500000000000002220 ) ) ;
#28987 = ORIENTED_EDGE ( 'NONE', *, *, #3147, .F. ) ;
#28988 = CARTESIAN_POINT ( 'NONE',  ( -5.903826827417286260, -5.876774720514418071, 20.39230070883895252 ) ) ;
#28989 = CARTESIAN_POINT ( 'NONE',  ( -9.798014431990228701, 18.61115389415964572, 11.49999999999998934 ) ) ;
#28990 = DIRECTION ( 'NONE',  ( 1.000000000000000000, 0.000000000000000000, 0.000000000000000000 ) ) ;
#28991 = CARTESIAN_POINT ( 'NONE',  ( 16.14549698687068968, 15.95341496147077720, 11.49999999999998934 ) ) ;
#28992 = AXIS2_PLACEMENT_3D ( 'NONE', #36419, #36918, #98304 ) ;
#28993 = CARTESIAN_POINT ( 'NONE',  ( 15.30881860688521989, -3.493868136757170451, -27.16033061360459300 ) ) ;
#28994 = DIRECTION ( 'NONE',  ( -3.773278334444167608E-23, 1.000000000000000000, 0.000000000000000000 ) ) ;
#28995 = CARTESIAN_POINT ( 'NONE',  ( -21.18249553426131015, -5.656070447573528170, -1.500000000000002220 ) ) ;
#28996 = CARTESIAN_POINT ( 'NONE',  ( -117.6228709571500559, -29.50250786944525672, 11.44777988621622811 ) ) ;
#28997 = ORIENTED_EDGE ( 'NONE', *, *, #9337, .F. ) ;
#28998 = CARTESIAN_POINT ( 'NONE',  ( -122.5564250028337767, -23.73791477778912551, 11.05961554403169878 ) ) ;
#28999 = LINE ( 'NONE', #21868, #88637 ) ;
#29000 = CARTESIAN_POINT ( 'NONE',  ( -41.62287095715007013, -23.96127896941631619, -0.6493128931037902563 ) ) ;
#29001 = CARTESIAN_POINT ( 'NONE',  ( 31.31283134548411340, 1.477225279485574028, -10.20862453625735533 ) ) ;
#29002 = CARTESIAN_POINT ( 'NONE',  ( -3.310264809446246570, -21.00426241492911927, 11.49999999999998934 ) ) ;
#29003 = CARTESIAN_POINT ( 'NONE',  ( -119.6228709571500559, -29.50247984919015209, -1.443849546365046699 ) ) ;
#29004 = DIRECTION ( 'NONE',  ( 0.000000000000000000, -1.000000000000000000, 0.000000000000000000 ) ) ;
#29005 = EDGE_CURVE ( 'NONE', #35855, #16750, #58121, .T. ) ;
#29006 = CARTESIAN_POINT ( 'NONE',  ( -85.54293262885111915, -24.73486907724917927, 1.287355809206964796 ) ) ;
#29007 = LINE ( 'NONE', #29501, #97791 ) ;
#29008 = APPROVAL ( #52618, 'UNSPECIFIED' ) ;
#29009 = VECTOR ( 'NONE', #18554, 1000.000000000000000 ) ;
#29010 = CARTESIAN_POINT ( 'NONE',  ( -117.5903086160344344, -24.15620529776629510, 10.23563542870659582 ) ) ;
#29011 = EDGE_LOOP ( 'NONE', ( #93612, #26476, #73671, #55167 ) ) ;
#29012 = CARTESIAN_POINT ( 'NONE',  ( -119.5895376238167245, -24.65952944569306027, 1.056160979905711894 ) ) ;
#29013 = CARTESIAN_POINT ( 'NONE',  ( 16.91694316922610497, -9.995573847407506207, 11.49999999999999645 ) ) ;
#29014 = CARTESIAN_POINT ( 'NONE',  ( -75.62287095715004170, -24.99156045073392818, 7.747789690856161648 ) ) ;
#29015 = CARTESIAN_POINT ( 'NONE',  ( -7.326923076923076650, -6.376774720514417183, 20.36318108974359831 ) ) ;
#29016 = ORIENTED_EDGE ( 'NONE', *, *, #17578, .F. ) ;
#29017 = CARTESIAN_POINT ( 'NONE',  ( -88.63497858377701277, -23.96169478059713853, 10.65365249895717703 ) ) ;
#29018 = EDGE_CURVE ( 'NONE', #12619, #5267, #41895, .T. ) ;
#29019 = CARTESIAN_POINT ( 'NONE',  ( -100.6347018612127613, -25.03409664067351059, 7.557395711288017459 ) ) ;
#29020 = CARTESIAN_POINT ( 'NONE',  ( -31.62287095715005236, -23.72747288104441665, -1.053458166803663554 ) ) ;
#29021 = CARTESIAN_POINT ( 'NONE',  ( -40.62287095715005592, -24.82576562982392687, 8.398263435472978600 ) ) ;
#29022 = CARTESIAN_POINT ( 'NONE',  ( -18.24397684793207830, 7.494555614300850266, 11.49999999999998934 ) ) ;
#29023 = ORIENTED_EDGE ( 'NONE', *, *, #28466, .T. ) ;
#29024 = DIRECTION ( 'NONE',  ( -0.8788171126619707119, 0.4771587602595986910, 0.000000000000000000 ) ) ;
#29025 = CARTESIAN_POINT ( 'NONE',  ( -126.6228709571500559, -24.64965695001469825, 8.947790433994173398 ) ) ;
#29026 = PERSON_AND_ORGANIZATION ( #70597, #27821 ) ;
#29027 = ORIENTED_EDGE ( 'NONE', *, *, #16253, .T. ) ;
#29028 = CARTESIAN_POINT ( 'NONE',  ( -107.5562042904834215, -24.64965694238575011, 8.947790433994189385 ) ) ;
#29029 = CARTESIAN_POINT ( 'NONE',  ( 6.600000000000001421, 0.000000000000000000, 0.000000000000000000 ) ) ;
#29030 = CARTESIAN_POINT ( 'NONE',  ( -55.62594774802067121, -24.92564183028978775, 1.928384488918253092 ) ) ;
#29031 = DIRECTION ( 'NONE',  ( -0.000000000000000000, -1.000000000000000000, -0.000000000000000000 ) ) ;
#29032 = CARTESIAN_POINT ( 'NONE',  ( -121.5228709571500616, -24.65952944569305316, 1.056160979905705899 ) ) ;
#29033 = AXIS2_PLACEMENT_3D ( 'NONE', #31178, #85464, #99189 ) ;
#29034 = CARTESIAN_POINT ( 'NONE',  ( -99.62287095715004170, -24.66019654487199730, 8.947790411086122830 ) ) ;
#29035 = CARTESIAN_POINT ( 'NONE',  ( -107.5179598396476024, -23.96119346886881729, -0.6495511937831858207 ) ) ;
#29037 = EDGE_CURVE ( 'NONE', #65549, #25965, #37264, .T. ) ;
#29036 = CARTESIAN_POINT ( 'NONE',  ( 13.87436705529610492, 14.39054836566213780, 11.49999999999998934 ) ) ;
#29038 = CARTESIAN_POINT ( 'NONE',  ( -127.6228709571500559, -23.72747288104441665, -1.053458166803660445 ) ) ;
#29039 = CARTESIAN_POINT ( 'NONE',  ( -0.0004629052523845373149, -23.04400732772759142, 4.713857633697502436 ) ) ;
#29040 = ORIENTED_EDGE ( 'NONE', *, *, #22177, .F. ) ;
#29041 = VECTOR ( 'NONE', #70042, 1000.000000000000000 ) ;
#29042 = LINE ( 'NONE', #59510, #63779 ) ;
#29043 = CARTESIAN_POINT ( 'NONE',  ( 4.639188450898540594, -5.876774720514418071, 20.39229233339611014 ) ) ;
#29044 = CIRCLE ( 'NONE', #42047, 6.119803529381341534 ) ;
#29045 = CARTESIAN_POINT ( 'NONE',  ( -119.5526355611971638, -24.65952944569305672, 1.056160979905715003 ) ) ;
#29046 = LINE ( 'NONE', #36664, #26499 ) ;
#29047 = CARTESIAN_POINT ( 'NONE',  ( -28.58953762381674224, -24.49351198072915281, 1.056161665704728136 ) ) ;
#29048 = CARTESIAN_POINT ( 'NONE',  ( -39.59380959696974855, -24.15543982623906416, -0.2315651400026677575 ) ) ;
#29049 = VECTOR ( 'NONE', #79112, 1000.000000000000114 ) ;
#29050 = EDGE_CURVE ( 'NONE', #21474, #37981, #1433, .T. ) ;
#29051 = LINE ( 'NONE', #22418, #26962 ) ;
#29052 = CARTESIAN_POINT ( 'NONE',  ( -51.04357394935764347, -25.26280107025014132, 4.940878043609458814 ) ) ;
#29053 = ORIENTED_EDGE ( 'NONE', *, *, #63883, .F. ) ;
#29054 = CARTESIAN_POINT ( 'NONE',  ( -34.62287095715006302, -24.51283580621363711, 0.6167428607019808107 ) ) ;
#29055 = CARTESIAN_POINT ( 'NONE',  ( -4.045674540461745572, 11.20951781186025897, 0.000000000000000000 ) ) ;
#29056 = ORIENTED_EDGE ( 'NONE', *, *, #35579, .F. ) ;
#29057 = CARTESIAN_POINT ( 'NONE',  ( -18.19507518397214341, 8.946258903265221107, 11.49999999999998934 ) ) ;
#29058 = CARTESIAN_POINT ( 'NONE',  ( -122.5222492194006207, -23.48783264082477373, -1.443836473390087471 ) ) ;
#29059 = EDGE_CURVE ( 'NONE', #61839, #62307, #96768, .T. ) ;
#29060 = CARTESIAN_POINT ( 'NONE',  ( -49.62287095715005592, -24.65952944569304250, 1.056160979905693020 ) ) ;
#29061 = ADVANCED_FACE ( 'NONE', ( #59113 ), #35276, .T. ) ;
#29062 = DIRECTION ( 'NONE',  ( -3.773278334453079030E-23, 0.9999999999976377785, 2.173523156925979128E-06 ) ) ;
#29063 = ORIENTED_EDGE ( 'NONE', *, *, #24091, .T. ) ;
#29064 = CARTESIAN_POINT ( 'NONE',  ( -78.52287095715004739, -24.66019654487199375, 8.947790411086119278 ) ) ;
#29065 = LINE ( 'NONE', #58048, #37323 ) ;
#29066 = CARTESIAN_POINT ( 'NONE',  ( -1.723993941171178879, -19.98520929721398431, -1.500000000000002220 ) ) ;
#29067 = CARTESIAN_POINT ( 'NONE',  ( 5.994809752082427501, 20.21905721239408393, 11.49999999999999645 ) ) ;
#29068 = PLANE ( 'NONE',  #64804 ) ;
#29069 = CARTESIAN_POINT ( 'NONE',  ( -70.62545108457702270, -24.92592662359561118, 8.075495903017998245 ) ) ;
#29070 = CARTESIAN_POINT ( 'NONE',  ( -14.46940225681120396, -16.66540133702554272, -1.500000000000002220 ) ) ;
#29071 = B_SPLINE_CURVE_WITH_KNOTS ( 'NONE', 3,
 ( #46323, #92983, #8262, #77251 ),
 .UNSPECIFIED., .F., .F.,
 ( 4, 4 ),
 ( 6.938893903907228378E-18, 0.0001000000000000167422 ),
 .UNSPECIFIED. ) ;
#29072 = CARTESIAN_POINT ( 'NONE',  ( -13.21525772315781388, 15.71049578022273785, 11.49999999999998934 ) ) ;
#29073 = PLANE ( 'NONE',  #23542 ) ;
#29074 = CARTESIAN_POINT ( 'NONE',  ( 31.59245846751552378, 5.049734226592146769, -4.287355462049295518 ) ) ;
#29075 = DIRECTION ( 'NONE',  ( -1.000000000000000000, -0.000000000000000000, -0.000000000000000000 ) ) ;
#29076 = VERTEX_POINT ( 'NONE', #20522 ) ;
#29077 = LINE ( 'NONE', #13346, #839 ) ;
#29078 = B_SPLINE_SURFACE_WITH_KNOTS ( 'NONE', 1, 3, ( 
 ( #35164, #44274, #43279, #12798, #51382, #97050, #51887, #43773, #81332, #67614 ),
 ( #90436, #12300, #98034, #66632, #27553, #98532, #89938, #28530, #74701, #4709 ) ),
 .UNSPECIFIED., .F., .F., .F.,
 ( 2, 2 ),
 ( 4, 2, 2, 2, 4 ),
 ( 0.000000000000000000, 1.000000000000000000 ),
 ( 0.000000000000000000, 0.2500000000000000000, 0.5000000000000000000, 0.7500000000000000000, 1.000000000000000000 ),
 .UNSPECIFIED. ) ;
#29079 = CARTESIAN_POINT ( 'NONE',  ( -29.55620429048340370, -23.39163958139442556, -1.443836129118754696 ) ) ;
#29080 = ORIENTED_EDGE ( 'NONE', *, *, #53805, .F. ) ;
#29081 = ORIENTED_EDGE ( 'NONE', *, *, #81844, .F. ) ;
#29082 = DIRECTION ( 'NONE',  ( -1.000000000000000000, -3.773278334444166432E-23, -8.201307841325785021E-29 ) ) ;
#29083 = DIRECTION ( 'NONE',  ( -0.000000000000000000, 1.000000000000000000, -0.000000000000000000 ) ) ;
#29084 = CARTESIAN_POINT ( 'NONE',  ( -76.53952647890686478, -24.65952944569303895, 1.056160979905700570 ) ) ;
#29085 = CARTESIAN_POINT ( 'NONE',  ( 7.647619880454145758, 19.11525441646967849, -1.500000000000002220 ) ) ;
#29086 = CARTESIAN_POINT ( 'NONE',  ( -13.01863397230089170, 17.21462230531794901, 11.49999999999999645 ) ) ;
#29087 = ORIENTED_EDGE ( 'NONE', *, *, #51163, .F. ) ;
#29088 = CARTESIAN_POINT ( 'NONE',  ( -99.36517007105946675, -25.30168654129753136, 4.687587830358475038 ) ) ;
#29089 = DIRECTION ( 'NONE',  ( 0.000000000000000000, 2.173523156925980399E-06, -0.9999999999976378895 ) ) ;
#29090 = CARTESIAN_POINT ( 'NONE',  ( 17.53502452033532677, 13.85421504792973479, 11.49999999999998934 ) ) ;
#29091 = CARTESIAN_POINT ( 'NONE',  ( -48.52287095715006160, -23.48786465467241769, 11.44779295918255002 ) ) ;
#29092 = DIRECTION ( 'NONE',  ( 9.210644184508402939E-16, 0.5747471426738538502, 0.8183310589170136318 ) ) ;
#29093 = ORIENTED_EDGE ( 'NONE', *, *, #73110, .F. ) ;
#29094 = CARTESIAN_POINT ( 'NONE',  ( -50.55620429048339304, -25.00182538069145011, 7.747789668545099317 ) ) ;
#29095 = CARTESIAN_POINT ( 'NONE',  ( 6.666194146093591399, -5.876774720514413630, 19.75460921626947908 ) ) ;
#29096 = CARTESIAN_POINT ( 'NONE',  ( 20.36350155627077640, -4.707376482769925374, -1.500000000000002220 ) ) ;
#29097 = VERTEX_POINT ( 'NONE', #36267 ) ;
#29098 = AXIS2_PLACEMENT_3D ( 'NONE', #66230, #64741, #90043 ) ;
#29100 = ORIENTED_EDGE ( 'NONE', *, *, #49221, .F. ) ;
#29099 = CARTESIAN_POINT ( 'NONE',  ( -39.44687923781921057, -25.28830591450888221, 4.188173661249233959 ) ) ;
#29101 = EDGE_LOOP ( 'NONE', ( #6608, #14611, #18711, #23861 ) ) ;
#29102 = EDGE_CURVE ( 'NONE', #64035, #40077, #98272, .T. ) ;
#29103 = CARTESIAN_POINT ( 'NONE',  ( -50.49632248188068928, -25.30259173606348000, 4.732524148509932083 ) ) ;
#29104 = CARTESIAN_POINT ( 'NONE',  ( 17.50165659415881336, 11.77592616506222711, -1.500000000000002220 ) ) ;
#29105 = EDGE_LOOP ( 'NONE', ( #7739, #67498, #100047, #47308 ) ) ;
#29106 = CARTESIAN_POINT ( 'NONE',  ( -117.6260434375350172, -24.15543982623907837, -0.2315651400026547124 ) ) ;
#29107 = CARTESIAN_POINT ( 'NONE',  ( -100.1979988280279201, -25.12215671659214777, 7.085055038744845213 ) ) ;
#29108 = CARTESIAN_POINT ( 'NONE',  ( 20.45693200876408469, 7.529271608661172621, -1.500000000000002220 ) ) ;
#29109 = CARTESIAN_POINT ( 'NONE',  ( -6.775140224358976226, -6.376774720514408301, 19.14743589743590846 ) ) ;
#29110 = VECTOR ( 'NONE', #79736, 1000.000000000000000 ) ;
#29111 = DIRECTION ( 'NONE',  ( 1.000000000000000000, 0.000000000000000000, -1.257682986112628908E-16 ) ) ;
#29112 = CARTESIAN_POINT ( 'NONE',  ( 0.000000000000000000, 1.530000000000000027, 0.3849999999999992872 ) ) ;
#29113 = CARTESIAN_POINT ( 'NONE',  ( 18.07971092720299922, 12.08445254275838465, -1.500000000000002220 ) ) ;
#29114 = CARTESIAN_POINT ( 'NONE',  ( -71.68214140181162009, -25.24674281957223343, 5.908703891276553044 ) ) ;
#29116 = ORIENTED_EDGE ( 'NONE', *, *, #93536, .F. ) ;
#29115 = CARTESIAN_POINT ( 'NONE',  ( -22.28969446433750434, -1.297463027894488086, 11.49999999999999645 ) ) ;
#29117 = DIRECTION ( 'NONE',  ( 0.000000000000000000, 0.9999999999976377785, 2.173523156925979975E-06 ) ) ;
#29118 = CARTESIAN_POINT ( 'NONE',  ( 0.000000000000000000, -2.056774720514426669, 0.000000000000000000 ) ) ;
#29119 = CARTESIAN_POINT ( 'NONE',  ( -106.6228709571500559, -29.50250243563736774, 8.947779886222136270 ) ) ;
#29120 = ORIENTED_EDGE ( 'NONE', *, *, #3081, .T. ) ;
#29121 = VECTOR ( 'NONE', #44364, 1000.000000000000000 ) ;
#29122 = ORIENTED_EDGE ( 'NONE', *, *, #3628, .T. ) ;
#29123 = VECTOR ( 'NONE', #35090, 1000.000000000000000 ) ;
#29124 = ORIENTED_EDGE ( 'NONE', *, *, #15511, .T. ) ;
#29125 = CIRCLE ( 'NONE', #22660, 25.90800000000000125 ) ;
#29126 = CARTESIAN_POINT ( 'NONE',  ( -82.62287095715005592, -24.64898659630367916, 1.056161002820826145 ) ) ;
#29127 = CARTESIAN_POINT ( 'NONE',  ( -87.62287095715004170, -29.50247984919015209, -1.443849546365051806 ) ) ;
#29128 = CARTESIAN_POINT ( 'NONE',  ( 30.62555539057593634, -4.734697315945937568, 27.74929510164747981 ) ) ;
#29129 = CARTESIAN_POINT ( 'NONE',  ( 6.499999999999992895, -2.035296314119462445E-15, 3.499999999999998224 ) ) ;
#29130 = EDGE_CURVE ( 'NONE', #15603, #46174, #69162, .T. ) ;
#29131 = AXIS2_PLACEMENT_3D ( 'NONE', #42256, #74665, #97508 ) ;
#29132 = CARTESIAN_POINT ( 'NONE',  ( -17.02366064725396555, -9.230830265533395362, -1.500000000000002220 ) ) ;
#29133 = DIRECTION ( 'NONE',  ( -0.000000000000000000, -0.000000000000000000, -1.000000000000000000 ) ) ;
#29134 = ORIENTED_EDGE ( 'NONE', *, *, #50945, .T. ) ;
#29135 = ADVANCED_FACE ( 'NONE', ( #90051 ), #97166, .F. ) ;
#29136 = CARTESIAN_POINT ( 'NONE',  ( 13.32768686175602646, -14.16729652289716057, 11.49999999999999645 ) ) ;
#29137 = CARTESIAN_POINT ( 'NONE',  ( -81.62287095715008434, -23.47596703998600631, 11.44779298504227860 ) ) ;
#29138 = ORIENTED_EDGE ( 'NONE', *, *, #415, .F. ) ;
#29139 = CARTESIAN_POINT ( 'NONE',  ( 3.749014282529493869, -6.376774720514404748, 18.52125941707705792 ) ) ;
#29140 = DIRECTION ( 'NONE',  ( 0.000000000000000000, 0.9999999999976377785, 2.173523156925979128E-06 ) ) ;
#29141 = ADVANCED_FACE ( 'NONE', ( #74811 ), #21514, .F. ) ;
#29142 = CARTESIAN_POINT ( 'NONE',  ( -109.8650282762807393, -29.50249556043354460, 5.784618828537300139 ) ) ;
#29143 = ADVANCED_FACE ( 'NONE', ( #13908 ), #82920, .T. ) ;
#29144 = CARTESIAN_POINT ( 'NONE',  ( -97.26334014122947735, -23.47596703998600631, 11.44779298504227860 ) ) ;
#29145 = CARTESIAN_POINT ( 'NONE',  ( 5.117700956428186565, 18.95590836763280862, -1.500000000000002220 ) ) ;
#29146 = CARTESIAN_POINT ( 'NONE',  ( -37.58953762381673869, -24.64898659630367206, 1.056161002820379169 ) ) ;
#29148 = EDGE_CURVE ( 'NONE', #78994, #404, #42889, .T. ) ;
#29147 = ORIENTED_EDGE ( 'NONE', *, *, #33917, .F. ) ;
#29149 = CARTESIAN_POINT ( 'NONE',  ( 14.33184905138074683, -16.10332302735202958, -1.500000000000002220 ) ) ;
#29150 = LINE ( 'NONE', #59618, #64160 ) ;
#29151 = DIRECTION ( 'NONE',  ( -2.352173255807804438E-16, 2.352173255807796056E-16, 1.000000000000000000 ) ) ;
#29152 = CARTESIAN_POINT ( 'NONE',  ( -40.66404017723625941, -23.85016227208580730, -0.8807180028928393023 ) ) ;
#29153 = CARTESIAN_POINT ( 'NONE',  ( -99.52764846858842418, -25.18439489159435496, 3.999772444794112314 ) ) ;
#29154 = CARTESIAN_POINT ( 'NONE',  ( -22.87025945403008365, 2.249016246415321163, -1.500000000000002220 ) ) ;
#29155 = B_SPLINE_CURVE_WITH_KNOTS ( 'NONE', 3,
 ( #83914, #51979, #59102, #74313 ),
 .UNSPECIFIED., .F., .F.,
 ( 4, 4 ),
 ( 0.9704789197191771022, 0.9794853509912926359 ),
 .UNSPECIFIED. ) ;
#29156 = CALENDAR_DATE ( 2026, 9, 10 ) ;
#29157 = CARTESIAN_POINT ( 'NONE',  ( -0.02075734969026423599, 6.376774720514426953, -29.05397719988137339 ) ) ;
#29158 = CARTESIAN_POINT ( 'NONE',  ( -49.50018282194935182, -25.18370859199909972, 3.285367768258824483 ) ) ;
#29159 = CARTESIAN_POINT ( 'NONE',  ( -15.75104486599040321, 12.61009050114280861, 11.49999999999999645 ) ) ;
#29160 = CARTESIAN_POINT ( 'NONE',  ( -101.5228709571500758, -24.64898659630368627, 1.056161002820829697 ) ) ;
#29161 = CARTESIAN_POINT ( 'NONE',  ( 13.91401389203221406, 5.965225279485572685, 158.0376437107427137 ) ) ;
#29162 = DIRECTION ( 'NONE',  ( 0.000000000000000000, -1.000000000000000000, 0.000000000000000000 ) ) ;
#29163 = CARTESIAN_POINT ( 'NONE',  ( -50.62287095715005592, -23.47596703998600631, 11.44779298504227505 ) ) ;
#29164 = CARTESIAN_POINT ( 'NONE',  ( 27.53860345374808105, 5.356774720496559894, -0.3523920347467610070 ) ) ;
#29166 = ADVANCED_FACE ( 'NONE', ( #51495 ), #27660, .F. ) ;
#29165 = CARTESIAN_POINT ( 'NONE',  ( 8.615496892348360802, 17.92367856960711947, -1.500000000000002220 ) ) ;
#29167 = CARTESIAN_POINT ( 'NONE',  ( -65.05438548721848235, -5.356774720514425603, 0.7300228001186309656 ) ) ;
#29168 = CARTESIAN_POINT ( 'NONE',  ( 19.18382676146983457, -4.683391092530263755, -1.500000000000002220 ) ) ;
#29169 = CARTESIAN_POINT ( 'NONE',  ( -126.5909419807629490, -23.48786465467241769, 11.44779295918253759 ) ) ;
#29170 = CARTESIAN_POINT ( 'NONE',  ( -0.02075734969026423599, -6.475225279485573360, -0.08597719988137648983 ) ) ;
#29171 = CARTESIAN_POINT ( 'NONE',  ( -37.52287095715008292, -23.48783264083359512, -1.443836473376374885 ) ) ;
#29172 = CARTESIAN_POINT ( 'NONE',  ( 1.453578435135240321, -20.60874541997745268, 11.49999999999999645 ) ) ;
#29173 = CARTESIAN_POINT ( 'NONE',  ( -111.5228709571500616, -24.64965694238407323, 8.947790433994192938 ) ) ;
#29174 = B_SPLINE_CURVE_WITH_KNOTS ( 'NONE', 3,
 ( #62711, #100224, #15502, #55093, #39850, #46469 ),
 .UNSPECIFIED., .F., .F.,
 ( 4, 2, 4 ),
 ( 1.570755371634072366E-05, 0.001396183895866090138, 0.002776660238015839482 ),
 .UNSPECIFIED. ) ;
#29175 = AXIS2_PLACEMENT_3D ( 'NONE', #74755, #81880, #73765 ) ;
#29176 = ADVANCED_FACE ( 'NONE', ( #89552 ), #44383, .T. ) ;
#29177 = DIRECTION ( 'NONE',  ( 3.773278334444166432E-23, -1.000000000000000000, 0.000000000000000000 ) ) ;
#29178 = CARTESIAN_POINT ( 'NONE',  ( -9.471985145535571249, 20.67137392225973258, 11.49999999999999645 ) ) ;
#29179 = VERTEX_POINT ( 'NONE', #43388 ) ;
#29180 = CARTESIAN_POINT ( 'NONE',  ( -46.62287095715004881, -23.48786465467241058, 11.44779295918255180 ) ) ;
#29181 = ADVANCED_FACE ( 'NONE', ( #74326 ), #35771, .T. ) ;
#29182 = CARTESIAN_POINT ( 'NONE',  ( 30.59070867143730155, 4.540774708561928108, 26.30292506078689385 ) ) ;
#29183 = AXIS2_PLACEMENT_3D ( 'NONE', #62043, #52935, #30580 ) ;
#29184 = CARTESIAN_POINT ( 'NONE',  ( -8.513533612778267923, 18.29693335657625042, -1.500000000000002220 ) ) ;
#29185 = PLANE ( 'NONE',  #64667 ) ;
#29186 = ADVANCED_FACE ( 'NONE', ( #5806 ), #61614, .T. ) ;
#29187 = CYLINDRICAL_SURFACE ( 'NONE', #9094, 0.3000000000000016542 ) ;
#29188 = VECTOR ( 'NONE', #50430, 1000.000000000000000 ) ;
#29189 = ORIENTED_EDGE ( 'NONE', *, *, #49224, .F. ) ;
#29190 = EDGE_CURVE ( 'NONE', #76875, #48556, #52284, .T. ) ;
#29191 = EDGE_LOOP ( 'NONE', ( #85723, #57669, #26496, #83490 ) ) ;
#29192 = DIRECTION ( 'NONE',  ( -0.4009304992412300317, 6.845827386180410961E-16, -0.9161084732596779245 ) ) ;
#29194 = CARTESIAN_POINT ( 'NONE',  ( 22.22072617242880455, -5.352622178732230118, 11.49999999999998934 ) ) ;
#29193 = B_SPLINE_CURVE_WITH_KNOTS ( 'NONE', 3,
 ( #24511, #79799, #55480, #32628 ),
 .UNSPECIFIED., .F., .F.,
 ( 4, 4 ),
 ( 0.000000000000000000, 9.999999999993347544E-05 ),
 .UNSPECIFIED. ) ;
#29196 = EDGE_CURVE ( 'NONE', #39424, #85639, #51423, .T. ) ;
#29195 = CARTESIAN_POINT ( 'NONE',  ( -29.62374991441511440, -24.58397407072015639, 1.056161296257513982 ) ) ;
#29197 = AXIS2_PLACEMENT_3D ( 'NONE', #85637, #85134, #1417 ) ;
#29198 = CARTESIAN_POINT ( 'NONE',  ( -20.54952838774410750, 6.582847151591199264, -1.500000000000002220 ) ) ;
#29199 = DIRECTION ( 'NONE',  ( -3.773278334453079030E-23, 0.9999999999976377785, 2.173523156925979128E-06 ) ) ;
#29200 = FACE_OUTER_BOUND ( 'NONE', #34241, .T. ) ;
#29201 = CARTESIAN_POINT ( 'NONE',  ( 16.93931825803137414, 14.88162037096512158, 11.49999999999999645 ) ) ;
#29202 = EDGE_LOOP ( 'NONE', ( #19025, #39102, #57087, #95517, #75275 ) ) ;
#29203 = CIRCLE ( 'NONE', #92418, 1.500000000000000666 ) ;
#29204 = CARTESIAN_POINT ( 'NONE',  ( -43.52287095715008292, -24.51283580621452529, 0.6167428607045876143 ) ) ;
#29205 = CARTESIAN_POINT ( 'NONE',  ( 19.49364837986538745, 10.19379059548657551, -1.500000000000002220 ) ) ;
#29207 = CARTESIAN_POINT ( 'NONE',  ( -105.5090414728886117, -24.83644354573579349, 8.397322867130096569 ) ) ;
#29206 = TOROIDAL_SURFACE ( 'NONE', #1621, 2.000000000000000000, 1.000000000000000000 ) ;
#29208 = CARTESIAN_POINT ( 'NONE',  ( -41.16467076663393243, -25.29087073963488663, 3.014415608521074486 ) ) ;
#29209 = ORIENTED_EDGE ( 'NONE', *, *, #15700, .F. ) ;
#29210 = CARTESIAN_POINT ( 'NONE',  ( -73.55620429048340725, -23.47593901973091235, -1.443836447539006196 ) ) ;
#29211 = CARTESIAN_POINT ( 'NONE',  ( -90.54765750514137324, -24.52399227489126687, 9.353111116836531735 ) ) ;
#29212 = ORIENTED_EDGE ( 'NONE', *, *, #86808, .T. ) ;
#29213 = DIRECTION ( 'NONE',  ( 1.000000000000000000, 3.773278334444166432E-23, 8.201307841325785021E-29 ) ) ;
#29214 = VERTEX_POINT ( 'NONE', #32135 ) ;
#29215 = ORIENTED_EDGE ( 'NONE', *, *, #95018, .F. ) ;
#29216 = CARTESIAN_POINT ( 'NONE',  ( -49.27764846858840997, -25.26180677598144086, 6.145204968850301874 ) ) ;
#29217 = CARTESIAN_POINT ( 'NONE',  ( 32.45853543194704116, -0.3587747205144265483, 9.169203677920338080 ) ) ;
#29218 = CARTESIAN_POINT ( 'NONE',  ( -57.55991777488805639, -23.73766607897670866, -1.055555164236458454 ) ) ;
#29219 = CARTESIAN_POINT ( 'NONE',  ( -13.80512455850298714, -15.04058748057734896, -1.500000000000002220 ) ) ;
#29220 = EDGE_LOOP ( 'NONE', ( #87765, #98833, #29826, #37258 ) ) ;
#29221 = CARTESIAN_POINT ( 'NONE',  ( -3.035630128403670192, -6.376774720514413630, 19.71630089903357685 ) ) ;
#29222 = LINE ( 'NONE', #75885, #91925 ) ;
#29223 = CARTESIAN_POINT ( 'NONE',  ( -4.635780534842457001, -6.376774720514410077, 19.53657742262743113 ) ) ;
#29224 = CARTESIAN_POINT ( 'NONE',  ( -25.53323730411857895, -24.91674856234845592, 5.128073852591860771 ) ) ;
#29225 = ORIENTED_EDGE ( 'NONE', *, *, #10549, .T. ) ;
#29226 = CARTESIAN_POINT ( 'NONE',  ( 10.24059822343757808, -5.876774720514426953, 17.91871304725684766 ) ) ;
#29227 = DIRECTION ( 'NONE',  ( 0.000000000000000000, -2.173523156925979552E-06, 0.9999999999976378895 ) ) ;
#29228 = CARTESIAN_POINT ( 'NONE',  ( 7.312689604342500260, -19.48077458720139532, 11.49999999999998934 ) ) ;
#29229 = VERTEX_POINT ( 'NONE', #30638 ) ;
#29231 = ORIENTED_EDGE ( 'NONE', *, *, #60045, .F. ) ;
#29230 = CARTESIAN_POINT ( 'NONE',  ( 6.499999999999992895, 3.983606557377048052, 3.319672131147540561 ) ) ;
#29232 = DIRECTION ( 'NONE',  ( 0.000000000000000000, 0.9999999999976377785, 2.173523156925979128E-06 ) ) ;
#29233 = ORIENTED_EDGE ( 'NONE', *, *, #43319, .F. ) ;
#29234 = ORIENTED_EDGE ( 'NONE', *, *, #31399, .T. ) ;
#29235 = FACE_OUTER_BOUND ( 'NONE', #19389, .T. ) ;
#29236 = CARTESIAN_POINT ( 'NONE',  ( -120.6228709571500417, -23.47593901973091235, -1.443836447538997536 ) ) ;
#29237 = CARTESIAN_POINT ( 'NONE',  ( -80.55620429048339304, -25.00158670708909625, 2.256160236439166855 ) ) ;
#29238 = CARTESIAN_POINT ( 'NONE',  ( -82.52287095715006160, -29.50247984919015209, -1.443849546365053582 ) ) ;
#29240 = VERTEX_POINT ( 'NONE', #54483 ) ;
#29239 = CARTESIAN_POINT ( 'NONE',  ( -4.051365815588555463, -21.74199345402511696, 11.49999999999999645 ) ) ;
#29241 = CARTESIAN_POINT ( 'NONE',  ( 7.749999999999998224, 24.84999999999999787, 2.100000000000000089 ) ) ;
#29242 = CARTESIAN_POINT ( 'NONE',  ( 8.854694546379761277, 20.84150027139232364, 11.49999999999998934 ) ) ;
#29244 = ORIENTED_EDGE ( 'NONE', *, *, #44154, .T. ) ;
#29243 = CARTESIAN_POINT ( 'NONE',  ( -115.5868009550897000, -25.00182538069147142, 7.747789668545041586 ) ) ;
#29245 = ORIENTED_EDGE ( 'NONE', *, *, #99760, .F. ) ;
#29246 = FACE_OUTER_BOUND ( 'NONE', #7395, .T. ) ;
#29247 = AXIS2_PLACEMENT_3D ( 'NONE', #2925, #26246, #40474 ) ;
#29248 = EDGE_CURVE ( 'NONE', #75484, #27205, #11127, .T. ) ;
#29249 = CARTESIAN_POINT ( 'NONE',  ( -16.19606052442943067, -11.93128464602566474, -1.500000000000002220 ) ) ;
#29250 = CARTESIAN_POINT ( 'NONE',  ( -27.15721599100127648, -6.376774720514425177, -10.22292133548837256 ) ) ;
#29251 = ORIENTED_EDGE ( 'NONE', *, *, #29018, .F. ) ;
#29252 = EDGE_CURVE ( 'NONE', #21619, #86369, #151, .T. ) ;
#29253 = CARTESIAN_POINT ( 'NONE',  ( -40.09822460666767086, -25.29345413520112018, 5.519450583125844467 ) ) ;
#29254 = CARTESIAN_POINT ( 'NONE',  ( 14.50327815619135308, -17.01817589256642194, -1.500000000000002220 ) ) ;
#29255 = EDGE_CURVE ( 'NONE', #3834, #49731, #85421, .T. ) ;
#29256 = ORIENTED_EDGE ( 'NONE', *, *, #30517, .T. ) ;
#29257 = ORIENTED_EDGE ( 'NONE', *, *, #25712, .F. ) ;
#29258 = CARTESIAN_POINT ( 'NONE',  ( 0.000000000000000000, -5.876774720514426953, 15.00000000000000178 ) ) ;
#29259 = CARTESIAN_POINT ( 'NONE',  ( -5.837039262820512775, -5.876774720514413630, 19.76512419871795245 ) ) ;
#29260 = CARTESIAN_POINT ( 'NONE',  ( -26.36280243631113507, -24.64751895363565737, 2.181899612272915956 ) ) ;
#29261 = EDGE_CURVE ( 'NONE', #10349, #55337, #84922, .T. ) ;
#29262 = CARTESIAN_POINT ( 'NONE',  ( -0.7638880233336636794, -9.374108182320437521, 9.000000000000000000 ) ) ;
#29263 = EDGE_CURVE ( 'NONE', #45940, #98622, #2840, .T. ) ;
#29264 = DIRECTION ( 'NONE',  ( 0.000000000000000000, 1.000000000000000000, -0.000000000000000000 ) ) ;
#29265 = VECTOR ( 'NONE', #5678, 1000.000000000000114 ) ;
#29266 = CARTESIAN_POINT ( 'NONE',  ( 14.28107258077893604, -13.35224110012613963, -1.500000000000002220 ) ) ;
#29267 = DIRECTION ( 'NONE',  ( -3.773278334453079618E-23, 0.9999999999976377785, 2.173523156925979975E-06 ) ) ;
#29269 = ADVANCED_FACE ( 'NONE', ( #76301 ), #70705, .T. ) ;
#29268 = AXIS2_PLACEMENT_3D ( 'NONE', #99466, #60934, #69543 ) ;
#29270 = CARTESIAN_POINT ( 'NONE',  ( -20.40864349294084334, -6.676163967499375573, 11.49999999999998934 ) ) ;
#29271 = CARTESIAN_POINT ( 'NONE',  ( -25.74893805332498076, -24.92775014605368256, 3.231001575389719882 ) ) ;
#29272 = FACE_OUTER_BOUND ( 'NONE', #86641, .T. ) ;
#29273 = DIRECTION ( 'NONE',  ( 0.000000000000000000, -1.000000000000000000, 1.571307496355802463E-16 ) ) ;
#29274 = CARTESIAN_POINT ( 'NONE',  ( 22.73759373355791169, -1.750760473330008171, -1.500000000000002220 ) ) ;
#29275 = AXIS2_PLACEMENT_3D ( 'NONE', #27287, #97782, #66364 ) ;
#29276 =( NAMED_UNIT ( * ) SI_UNIT ( $, .STERADIAN. ) SOLID_ANGLE_UNIT ( ) );
#29277 = CARTESIAN_POINT ( 'NONE',  ( -96.58867564644825165, -24.35071581493543391, 9.817618358456023486 ) ) ;
#29278 = DIRECTION ( 'NONE',  ( -0.1875268396392987258, 0.000000000000000000, -0.9822594791677485837 ) ) ;
#29279 = CARTESIAN_POINT ( 'NONE',  ( -4.495603250223349612, -19.44740727768710187, 11.49999999999999645 ) ) ;
#29280 = CARTESIAN_POINT ( 'NONE',  ( -64.52287095715006160, -24.64898659630528854, 1.056161002820822592 ) ) ;
#29281 = CARTESIAN_POINT ( 'NONE',  ( -74.50753224588216028, -24.15620529776628800, 10.23563542870659937 ) ) ;
#29282 = DIRECTION ( 'NONE',  ( 7.960204194457801640E-17, 1.000000000000000000, 0.000000000000000000 ) ) ;
#29283 = VERTEX_POINT ( 'NONE', #92036 ) ;
#29284 = CARTESIAN_POINT ( 'NONE',  ( -8.160000000000000142, 7.891155995661682354, 6.788828319098143993 ) ) ;
#29285 = ADVANCED_FACE ( 'NONE', ( #84425 ), #15405, .T. ) ;
#29286 = DIRECTION ( 'NONE',  ( -1.000000000000000000, -3.773278334444167608E-23, -8.201307833595939069E-29 ) ) ;
#29287 = CARTESIAN_POINT ( 'NONE',  ( -18.42844947050907578, 11.51566461966115540, -1.500000000000002220 ) ) ;
#29288 = DIRECTION ( 'NONE',  ( 0.000000000000000000, 0.000000000000000000, -1.000000000000000000 ) ) ;
#29289 = CARTESIAN_POINT ( 'NONE',  ( 12.01011565470214393, -15.49198969801113890, -1.500000000000002220 ) ) ;
#29290 = FACE_OUTER_BOUND ( 'NONE', #76033, .T. ) ;
#29291 = ADVANCED_FACE ( 'NONE', ( #69712 ), #99630, .F. ) ;
#29292 = EDGE_LOOP ( 'NONE', ( #97479, #70769, #79988, #56412 ) ) ;
#29293 = CARTESIAN_POINT ( 'NONE',  ( -108.8968792378191779, -25.11711062963908603, 7.140618811323130366 ) ) ;
#29294 = CARTESIAN_POINT ( 'NONE',  ( -0.02075734969026423599, 0.3587747205144213303, -0.08597719988137648983 ) ) ;
#29295 = CARTESIAN_POINT ( 'NONE',  ( -15.50425215161893355, 13.37805140191733777, 11.49999999999999645 ) ) ;
#29296 = PLANE ( 'NONE',  #36000 ) ;
#29297 = ADVANCED_FACE ( 'NONE', ( #53500 ), #46366, .T. ) ;
#29298 = CARTESIAN_POINT ( 'NONE',  ( 22.62151214508649844, 3.791242534904204664E-15, -2.299999999999999822 ) ) ;
#29299 = ORIENTED_EDGE ( 'NONE', *, *, #46001, .F. ) ;
#29300 = CARTESIAN_POINT ( 'NONE',  ( -109.4921708791334396, -25.30340751872594396, 4.738595968073344267 ) ) ;
#29301 = CARTESIAN_POINT ( 'NONE',  ( -40.06853693287165186, -25.28892436075654970, 3.358277935517027135 ) ) ;
#29302 = DIRECTION ( 'NONE',  ( 1.000000000000000000, -7.960204194457801640E-17, 0.000000000000000000 ) ) ;
#29303 = CARTESIAN_POINT ( 'NONE',  ( -4.141025641025638748, -6.376774720514427841, 21.75000000000000355 ) ) ;
#29304 = VERTEX_POINT ( 'NONE', #30134 ) ;
#29305 = CARTESIAN_POINT ( 'NONE',  ( 32.51008598047019404, 5.548342165039966467, -1.163674249303449315 ) ) ;
#29306 = B_SPLINE_CURVE_WITH_KNOTS ( 'NONE', 3,
 ( #31221, #62190, #93115, #21601, #85505, #76388, #44469, #5890, #54083, #68797, #67815, #75894, #61201, #98738, #91127, #92614, #53084, #45964, #69291, #22591, #52574, #84511, #83509 ),
 .UNSPECIFIED., .F., .F.,
 ( 4, 1, 1, 1, 1, 1, 1, 1, 1, 1, 1, 1, 1, 1, 1, 1, 1, 1, 1, 1, 4 ),
 ( 0.000000000000000000, 0.06038661931106227565, 0.1208832485859964029, 0.1827546186251403082, 0.2478110297583512034, 0.2812991000432494282, 0.3150876241506579412, 0.3497023955502757131, 0.3848565811185565289, 0.4209661972261032892, 0.4585111882611391243, 0.4971747221273126183, 0.5376020478662695279, 0.5805030184200120624, 0.6274675400267057945, 0.6783882095592440598, 0.7339832205925608255, 0.7937467045508355135, 0.8577136721607333536, 0.9266978643613864586, 1.000000000000000000 ),
 .UNSPECIFIED. ) ;
#29307 = EDGE_CURVE ( 'NONE', #78121, #37899, #77299, .T. ) ;
#29308 = CARTESIAN_POINT ( 'NONE',  ( -0.3492834940180428727, 22.98956000712751546, 11.49999999999999645 ) ) ;
#29309 = CARTESIAN_POINT ( 'NONE',  ( -22.16177213047534877, -5.259615592301647879, -1.500000000000002220 ) ) ;
#29310 = CARTESIAN_POINT ( 'NONE',  ( -34.52287095715006160, -23.47596703998600631, 11.44779298504229459 ) ) ;
#29311 = CARTESIAN_POINT ( 'NONE',  ( 7.166666666666668739, -5.876774720514419847, 20.78665865384614975 ) ) ;
#29312 = PLANE ( 'NONE',  #87341 ) ;
#29313 = CARTESIAN_POINT ( 'NONE',  ( -115.5228709571500332, -23.85196035786900026, -0.8779234886475116850 ) ) ;
#29314 = CARTESIAN_POINT ( 'NONE',  ( -69.62287095715005592, -24.64898659630528854, 1.056161002820824368 ) ) ;
#29316 = EDGE_CURVE ( 'NONE', #54573, #31114, #76793, .T. ) ;
#29315 = AXIS2_PLACEMENT_3D ( 'NONE', #1707, #25025, #63112 ) ;
#29317 = CARTESIAN_POINT ( 'NONE',  ( 15.10893391618534665, -15.86458014800626692, 11.49999999999998934 ) ) ;
#29318 = CARTESIAN_POINT ( 'NONE',  ( -97.62287095715005592, -29.50250243563736774, 8.947779886222138046 ) ) ;
#29319 = DIRECTION ( 'NONE',  ( 0.6599726524652352877, 0.000000000000000000, -0.7512896232465891000 ) ) ;
#29320 = CARTESIAN_POINT ( 'NONE',  ( -40.73160982624488469, -25.31552648564060348, 5.045570495695059776 ) ) ;
#29321 = CARTESIAN_POINT ( 'NONE',  ( -125.5895376238167529, -24.99156044556120904, 7.747789690856343725 ) ) ;
#29322 = CARTESIAN_POINT ( 'NONE',  ( -117.6228709571500701, -24.50216790748100237, 0.6166512839513771382 ) ) ;
#29323 = CARTESIAN_POINT ( 'NONE',  ( -4.401146115524053215, -5.876774720514411854, 19.34190049657481936 ) ) ;
#29324 = ORIENTED_EDGE ( 'NONE', *, *, #8701, .T. ) ;
#29325 = CARTESIAN_POINT ( 'NONE',  ( 19.09590870110849181, 7.302211495713927469, 11.49999999999998934 ) ) ;
#29326 = ORIENTED_EDGE ( 'NONE', *, *, #99941, .F. ) ;
#29327 = ORIENTED_EDGE ( 'NONE', *, *, #86332, .F. ) ;
#29328 = ORIENTED_EDGE ( 'NONE', *, *, #62272, .T. ) ;
#29329 = ORIENTED_EDGE ( 'NONE', *, *, #38891, .T. ) ;
#29330 = EDGE_CURVE ( 'NONE', #71528, #51268, #93027, .T. ) ;
#29331 = CARTESIAN_POINT ( 'NONE',  ( 6.753845092018655016, 22.03294598498517232, 11.49999999999998934 ) ) ;
#29332 = CARTESIAN_POINT ( 'NONE',  ( -61.64837733756440485, -23.73766607897669800, -1.055555164236459120 ) ) ;
#29333 = CARTESIAN_POINT ( 'NONE',  ( -9.470923242388245455, -17.85692771776473364, -1.500000000000002220 ) ) ;
#29334 = EDGE_LOOP ( 'NONE', ( #4641, #96936, #89489, #24614 ) ) ;
#29335 = CARTESIAN_POINT ( 'NONE',  ( -35.62287095715005592, -25.00182538069145011, 7.747789668545097541 ) ) ;
#29336 = DIRECTION ( 'NONE',  ( -3.773278334453079030E-23, 0.9999999999976377785, 2.173523156925979128E-06 ) ) ;
#29338 = PLANE ( 'NONE',  #82127 ) ;
#29337 = VECTOR ( 'NONE', #11935, 1000.000000000000227 ) ;
#29339 = CARTESIAN_POINT ( 'NONE',  ( -99.59615874627706944, -23.73791477778911840, 11.05961554403170410 ) ) ;
#29341 = EDGE_LOOP ( 'NONE', ( #2312, #99931, #67838, #76522 ) ) ;
#29340 = CARTESIAN_POINT ( 'NONE',  ( 15.25824911148008844, 15.06768998368162471, 11.49999999999999645 ) ) ;
#29342 = DIRECTION ( 'NONE',  ( 0.000000000000000000, -2.173523156925980399E-06, 0.9999999999976378895 ) ) ;
#29343 = CARTESIAN_POINT ( 'NONE',  ( -91.62287095715004170, -23.47596703998600631, 11.44779298504227860 ) ) ;
#29344 = VERTEX_POINT ( 'NONE', #87935 ) ;
#29345 = CARTESIAN_POINT ( 'NONE',  ( -1.843323519027639357, -20.62917239659568835, 11.49999999999998934 ) ) ;
#29347 = ORIENTED_EDGE ( 'NONE', *, *, #64133, .T. ) ;
#29346 = CYLINDRICAL_SURFACE ( 'NONE', #34508, 8.452410033082760066 ) ;
#29348 = B_SPLINE_CURVE_WITH_KNOTS ( 'NONE', 3,
 ( #45479, #82524, #51589, #52085, #22109, #43481 ),
 .UNSPECIFIED., .F., .F.,
 ( 4, 2, 4 ),
 ( 0.000000000000000000, 0.001380901958385387894, 0.002761803916770775788 ),
 .UNSPECIFIED. ) ;
#29349 = CARTESIAN_POINT ( 'NONE',  ( -91.52287095715010423, -24.66019654487199730, 8.947790411086115725 ) ) ;
#29350 = ORIENTED_EDGE ( 'NONE', *, *, #34030, .T. ) ;
#29351 = CARTESIAN_POINT ( 'NONE',  ( 4.588387839717440464, -5.876774720514399419, 18.52756237589653665 ) ) ;
#29352 = ORIENTED_EDGE ( 'NONE', *, *, #5711, .T. ) ;
#29353 = CARTESIAN_POINT ( 'NONE',  ( 18.73254098450790295, -9.497730595714260815, -1.500000000000002220 ) ) ;
#29354 = CARTESIAN_POINT ( 'NONE',  ( 18.29167757401336303, -12.14499471347784798, 11.49999999999999645 ) ) ;
#29355 = CARTESIAN_POINT ( 'NONE',  ( -37.47956771133813447, -24.66019654487199730, 8.947790411086113949 ) ) ;
#29356 = CARTESIAN_POINT ( 'NONE',  ( 3.584315319034878211, 22.25550262085195286, 11.49999999999998934 ) ) ;
#29357 = CARTESIAN_POINT ( 'NONE',  ( -11.48448384864204996, -17.54081393385053644, -1.500000000000002220 ) ) ;
#29358 = CARTESIAN_POINT ( 'NONE',  ( -89.62287095715004170, -23.47593901973091235, -1.443836447539002865 ) ) ;
#29359 = FACE_BOUND ( 'NONE', #35980, .T. ) ;
#29360 = CARTESIAN_POINT ( 'NONE',  ( 6.044119082205957838, -6.376774720514424288, 21.40268112089023589 ) ) ;
#29361 = ORIENTED_EDGE ( 'NONE', *, *, #90543, .T. ) ;
#29362 = ORIENTED_EDGE ( 'NONE', *, *, #44216, .T. ) ;
#29363 = ORIENTED_EDGE ( 'NONE', *, *, #86675, .F. ) ;
#29364 = DIRECTION ( 'NONE',  ( -1.000000000000000000, 7.960204194457801640E-17, 0.000000000000000000 ) ) ;
#29365 = B_SPLINE_CURVE_WITH_KNOTS ( 'NONE', 3,
 ( #1172, #71186, #94007, #93001, #32614, #31106, #23476, #32108 ),
 .UNSPECIFIED., .F., .F.,
 ( 4, 2, 2, 4 ),
 ( 6.384118678617666368E-06, 0.002007151183507260590, 0.003007534715921582075, 0.004007918248335903995 ),
 .UNSPECIFIED. ) ;
#29366 = CARTESIAN_POINT ( 'NONE',  ( 7.253797376210795456, 20.28272692992397808, -1.500000000000002220 ) ) ;
#29367 = EDGE_CURVE ( 'NONE', #50535, #93762, #3705, .T. ) ;
#29368 = DIRECTION ( 'NONE',  ( -1.000000000000000000, 1.232047923278981953E-16, 0.000000000000000000 ) ) ;
#29369 = VERTEX_POINT ( 'NONE', #63615 ) ;
#29370 = CARTESIAN_POINT ( 'NONE',  ( -4.502559807402421121, -20.62786074129878955, 11.49999999999998934 ) ) ;
#29371 = CARTESIAN_POINT ( 'NONE',  ( -7.160000000000000142, 8.793627758918228565, -2.994553991265763049 ) ) ;
#29372 = EDGE_CURVE ( 'NONE', #27253, #81452, #43656, .T. ) ;
#29373 = FACE_OUTER_BOUND ( 'NONE', #77475, .T. ) ;
#29374 = CARTESIAN_POINT ( 'NONE',  ( -83.51346219904408485, -23.96169478059713143, 10.65365249895718058 ) ) ;
#29375 = LINE ( 'NONE', #98379, #88031 ) ;
#29376 = CARTESIAN_POINT ( 'NONE',  ( -70.52287095715007581, -24.99132157543166599, 2.256160258750667502 ) ) ;
#29377 = CARTESIAN_POINT ( 'NONE',  ( -17.20036718215007099, 13.84871166177648583, -1.500000000000002220 ) ) ;
#29378 = ADVANCED_FACE ( 'NONE', ( #87426 ), #11833, .T. ) ;
#29379 = DIRECTION ( 'NONE',  ( -0.000000000000000000, -1.000000000000000000, -0.000000000000000000 ) ) ;
#29380 = ADVANCED_FACE ( 'NONE', ( #10808 ), #95543, .T. ) ;
#29381 = ORIENTED_EDGE ( 'NONE', *, *, #52998, .F. ) ;
#29382 = CARTESIAN_POINT ( 'NONE',  ( -109.6485756676466252, -25.29374954521688679, 5.552272408820409844 ) ) ;
#29383 = CARTESIAN_POINT ( 'NONE',  ( -79.62287095715005592, -24.64898659630528854, 1.056161002820826145 ) ) ;
#29384 = CARTESIAN_POINT ( 'NONE',  ( -83.55620429048339304, -23.47593901973091235, -1.443836447539004642 ) ) ;
#29385 = EDGE_CURVE ( 'NONE', #85000, #27060, #95773, .T. ) ;
#29386 = DIRECTION ( 'NONE',  ( -3.773278334453080206E-23, 0.9999999999976377785, 2.173523156925979975E-06 ) ) ;
#29387 = CARTESIAN_POINT ( 'NONE',  ( -5.694372300836820777, 18.57635362771370424, 11.49999999999998934 ) ) ;
#29388 = CARTESIAN_POINT ( 'NONE',  ( -17.73838780825237649, 11.93509662624355450, 11.49999999999998934 ) ) ;
#29389 = CARTESIAN_POINT ( 'NONE',  ( 2.589743589743596086, -6.376774720514415407, 20.00140224358974095 ) ) ;
#29390 = CARTESIAN_POINT ( 'NONE',  ( -81.55620429048339304, -23.48786465467241413, 11.44779295918255180 ) ) ;
#29391 = AXIS2_PLACEMENT_3D ( 'NONE', #81081, #20167, #11557 ) ;
#29392 = CARTESIAN_POINT ( 'NONE',  ( -123.5228709571500474, -23.47593901973090524, -1.443836447538996204 ) ) ;
#29393 = FACE_OUTER_BOUND ( 'NONE', #69981, .T. ) ;
#29394 = CARTESIAN_POINT ( 'NONE',  ( 12.64511023617726160, -18.80563239904246231, -1.500000000000002220 ) ) ;
#29395 = ORIENTED_EDGE ( 'NONE', *, *, #1936, .T. ) ;
#29396 = CARTESIAN_POINT ( 'NONE',  ( 282.9764569301858046, 0.3587747205144265483, 20.79159422840526616 ) ) ;
#29397 = DIRECTION ( 'NONE',  ( 0.000000000000000000, 0.000000000000000000, -1.000000000000000000 ) ) ;
#29398 = CARTESIAN_POINT ( 'NONE',  ( -3.504374479207110316, 19.46862825742285708, 11.49999999999999645 ) ) ;
#29399 = CARTESIAN_POINT ( 'NONE',  ( -76.52287095715011844, -23.48783264082477373, -1.443836473390087694 ) ) ;
#29400 = ORIENTED_EDGE ( 'NONE', *, *, #92519, .F. ) ;
#29401 = DIRECTION ( 'NONE',  ( -3.773278334453079618E-23, 0.9999999999976377785, 2.173523156925979975E-06 ) ) ;
#29402 = CARTESIAN_POINT ( 'NONE',  ( -93.62287095715005592, -29.50248528299804818, 1.056150453629040253 ) ) ;
#29403 = CARTESIAN_POINT ( 'NONE',  ( 14.58690015069645263, 15.99052346098381250, -1.500000000000002220 ) ) ;
#29404 = CARTESIAN_POINT ( 'NONE',  ( -49.27110903475092130, -25.27518005823318958, 3.423268546580319871 ) ) ;
#29405 = CARTESIAN_POINT ( 'NONE',  ( -2.795030477444873540, 19.22867370847827573, -1.500000000000002220 ) ) ;
#29406 = CARTESIAN_POINT ( 'NONE',  ( -129.6228709571500133, -23.96177878511308634, 10.65340807706329507 ) ) ;
#29407 = DIRECTION ( 'NONE',  ( -3.773278334453079618E-23, 0.9999999999976377785, 2.173523156925979975E-06 ) ) ;
#29408 = CARTESIAN_POINT ( 'NONE',  ( 19.51516567812286596, -3.327523070855789911, 11.49999999999998934 ) ) ;
#29409 = VECTOR ( 'NONE', #65628, 1000.000000000000114 ) ;
#29410 = ORIENTED_EDGE ( 'NONE', *, *, #1162, .F. ) ;
#29411 = LOCAL_TIME ( 0, 54, 15.00000000000000000, #7429 ) ;
#29412 = CARTESIAN_POINT ( 'NONE',  ( 6.737473828552405841, -19.20966278261563076, 11.49999999999999645 ) ) ;
#29413 = DIRECTION ( 'NONE',  ( -0.000000000000000000, -1.000000000000000000, -0.000000000000000000 ) ) ;
#29414 = CARTESIAN_POINT ( 'NONE',  ( 33.61752870511802627, -3.456547803086310378, -11.38123630260490948 ) ) ;
#29415 = ORIENTED_EDGE ( 'NONE', *, *, #55916, .T. ) ;
#29416 = CARTESIAN_POINT ( 'NONE',  ( -102.5093980281331483, -24.66019654487200086, 8.947790411086115725 ) ) ;
#29417 = CARTESIAN_POINT ( 'NONE',  ( -27.70544111104076990, -29.50250092294406912, 8.251816161026548357 ) ) ;
#29418 = DIRECTION ( 'NONE',  ( -0.000000000000000000, 1.000000000000000000, -0.000000000000000000 ) ) ;
#29419 = CARTESIAN_POINT ( 'NONE',  ( -77.62287095715005592, -24.64965695001468404, 8.947790433994182280 ) ) ;
#29420 = CARTESIAN_POINT ( 'NONE',  ( -51.36280043207702306, -25.18807129067230832, 6.689554096649111159 ) ) ;
#29421 = CARTESIAN_POINT ( 'NONE',  ( -14.05898297266747221, -14.31596314050798568, -1.500000000000002220 ) ) ;
#29422 = DIRECTION ( 'NONE',  ( 0.000000000000000000, 0.000000000000000000, -1.000000000000000000 ) ) ;
#29423 = VERTEX_POINT ( 'NONE', #42288 ) ;
#29424 = LINE ( 'NONE', #91327, #52780 ) ;
#29425 = CARTESIAN_POINT ( 'NONE',  ( -22.75767140345847750, 1.815691853630000629, 11.49999999999999645 ) ) ;
#29426 = CARTESIAN_POINT ( 'NONE',  ( -30.47287095715006799, -24.66342764659571074, 1.121861807716615145 ) ) ;
#29427 = CARTESIAN_POINT ( 'NONE',  ( -96.52287095715006160, -29.50250243563736774, 8.947779886222138046 ) ) ;
#29428 = CARTESIAN_POINT ( 'NONE',  ( 2.903846153846159517, -6.376774720514415407, 19.99999999999999289 ) ) ;
#29429 = CARTESIAN_POINT ( 'NONE',  ( -89.62287095715004170, -23.47593901973091235, -1.443836447539002865 ) ) ;
#29430 = EDGE_CURVE ( 'NONE', #62504, #18736, #84789, .T. ) ;
#29431 = ADVANCED_BREP_SHAPE_REPRESENTATION ( '', ( #43720, #37391 ), #45585 ) ;
#29432 = CARTESIAN_POINT ( 'NONE',  ( -117.5895376238167245, -23.47596703998600631, 11.44779298504227683 ) ) ;
#29433 = AXIS2_PLACEMENT_3D ( 'NONE', #74790, #4301, #51973 ) ;
#29434 = ADVANCED_FACE ( 'NONE', ( #56000 ), #64123, .F. ) ;
#29435 = CARTESIAN_POINT ( 'NONE',  ( 22.02124265030973760, -4.543225279485573864, 13.95402280011862395 ) ) ;
#29436 = VERTEX_POINT ( 'NONE', #17924 ) ;
#29437 = CARTESIAN_POINT ( 'NONE',  ( -17.59887021274124663, -10.25344800880639262, 11.49999999999998934 ) ) ;
#29438 = EDGE_LOOP ( 'NONE', ( #88141, #99458, #97049, #49400 ) ) ;
#29439 = CARTESIAN_POINT ( 'NONE',  ( 22.74528686061176685, 3.085755641335488964, -1.500000000000002220 ) ) ;
#29440 = DIRECTION ( 'NONE',  ( -3.773278334453079618E-23, 0.9999999999976377785, 2.173523156925979975E-06 ) ) ;
#29441 = ORIENTED_EDGE ( 'NONE', *, *, #78387, .F. ) ;
#29442 = DIRECTION ( 'NONE',  ( 3.773278334444166432E-23, -1.000000000000000000, 0.000000000000000000 ) ) ;
#29443 = CARTESIAN_POINT ( 'NONE',  ( -77.50430339230356935, -24.35071581493544102, 9.817618358456021710 ) ) ;
#29444 = CARTESIAN_POINT ( 'NONE',  ( -80.96226385320382235, -25.13069340115295702, 2.947789388436138580 ) ) ;
#29446 = ORIENTED_EDGE ( 'NONE', *, *, #56732, .F. ) ;
#29445 = CARTESIAN_POINT ( 'NONE',  ( 21.11169859150035677, 2.410084449224629832, 11.49999999999999645 ) ) ;
#29447 = ORIENTED_EDGE ( 'NONE', *, *, #85284, .T. ) ;
#29448 = CARTESIAN_POINT ( 'NONE',  ( -7.477829544921322125, 20.88912457518834742, 11.49999999999998934 ) ) ;
#29449 = CIRCLE ( 'NONE', #53808, 84.48086791635431325 ) ;
#29450 = CARTESIAN_POINT ( 'NONE',  ( -15.40095275084150117, -13.70674696055758801, 11.49999999999998934 ) ) ;
#29451 = B_SPLINE_CURVE_WITH_KNOTS ( 'NONE', 3,
 ( #41136, #1064, #56371, #49259, #87291, #8675 ),
 .UNSPECIFIED., .F., .F.,
 ( 4, 2, 4 ),
 ( 6.384118678621234070E-06, 0.001386860460828383441, 0.002767336802978145362 ),
 .UNSPECIFIED. ) ;
#29452 = VERTEX_POINT ( 'NONE', #51371 ) ;
#29453 = ORIENTED_EDGE ( 'NONE', *, *, #83778, .T. ) ;
#29454 = DIRECTION ( 'NONE',  ( 0.000000000000000000, 0.9999999999976377785, 2.173523156925979975E-06 ) ) ;
#29455 = CARTESIAN_POINT ( 'NONE',  ( -54.62287095715004170, -23.47596703998600631, 11.44779298504227505 ) ) ;
#29456 = ORIENTED_EDGE ( 'NONE', *, *, #14840, .F. ) ;
#29457 = ORIENTED_EDGE ( 'NONE', *, *, #31082, .F. ) ;
#29458 = DIRECTION ( 'NONE',  ( -1.000000000000000000, 0.000000000000000000, 0.000000000000000000 ) ) ;
#29459 = CARTESIAN_POINT ( 'NONE',  ( -111.6286693378537507, -23.96169478059714564, 10.65365249895717348 ) ) ;
#29460 = CARTESIAN_POINT ( 'NONE',  ( -48.52287095715007581, -23.72747288104470087, -1.053458166803227458 ) ) ;
#29461 = CARTESIAN_POINT ( 'NONE',  ( 11.56195852851363526, -17.29799701895051811, -1.500000000000002220 ) ) ;
#29462 = CARTESIAN_POINT ( 'NONE',  ( 4.771108217193557266, 21.26182814020628697, 11.49999999999999645 ) ) ;
#29463 = CARTESIAN_POINT ( 'NONE',  ( -39.66923462213467388, -25.22668475970086988, 3.617326360174414113 ) ) ;
#29464 = DIRECTION ( 'NONE',  ( 0.000000000000000000, 0.000000000000000000, 1.000000000000000000 ) ) ;
#29465 = CARTESIAN_POINT ( 'NONE',  ( -0.1411031551986380028, 22.44022050402121948, 11.49999999999998934 ) ) ;
#29466 = CARTESIAN_POINT ( 'NONE',  ( -51.28074245548943111, -25.26334620367392247, 4.131999547932733385 ) ) ;
#29467 = EDGE_CURVE ( 'NONE', #74882, #18460, #81217, .T. ) ;
#29468 = VERTEX_POINT ( 'NONE', #66621 ) ;
#29469 = CARTESIAN_POINT ( 'NONE',  ( -75.52287095715013265, -24.91544648472621049, 1.928969306349232582 ) ) ;
#29470 = AXIS2_PLACEMENT_3D ( 'NONE', #60519, #43786, #51398 ) ;
#29471 = CARTESIAN_POINT ( 'NONE',  ( -69.52287095715010423, -24.33927499327855770, 9.819080762295813614 ) ) ;
#29472 = SECURITY_CLASSIFICATION ( '', '', #46886 ) ;
#29473 = ORIENTED_EDGE ( 'NONE', *, *, #91163, .T. ) ;
#29474 = ORIENTED_EDGE ( 'NONE', *, *, #32480, .T. ) ;
#29475 = DIRECTION ( 'NONE',  ( 2.352173255807804438E-16, -2.352173255807796056E-16, -1.000000000000000000 ) ) ;
#29476 = VERTEX_POINT ( 'NONE', #81318 ) ;
#29477 = CARTESIAN_POINT ( 'NONE',  ( -18.64022381217131397, 10.26305532446727753, -1.500000000000002220 ) ) ;
#29478 = ORIENTED_EDGE ( 'NONE', *, *, #2896, .T. ) ;
#29479 = DIRECTION ( 'NONE',  ( 0.000000000000000000, 0.000000000000000000, -1.000000000000000000 ) ) ;
#29480 = CARTESIAN_POINT ( 'NONE',  ( -20.98013922110768448, -1.350454208470041273, 11.49999999999998934 ) ) ;
#29481 = CARTESIAN_POINT ( 'NONE',  ( -125.5228709571500616, -23.48783264083375144, -1.443836473376139740 ) ) ;
#29482 = EDGE_CURVE ( 'NONE', #59175, #86526, #75086, .T. ) ;
#29483 = CARTESIAN_POINT ( 'NONE',  ( 14.64534568429317218, -3.754078354150065522, -27.31564152833324499 ) ) ;
#29484 = PLANE ( 'NONE',  #12584 ) ;
#29485 = CARTESIAN_POINT ( 'NONE',  ( 1.548332177993611225, -21.85883989728069565, -1.500000000000002220 ) ) ;
#29486 = CARTESIAN_POINT ( 'NONE',  ( -87.54287996507414960, -24.65952944569304606, 1.056160979905703678 ) ) ;
#29487 = ORIENTED_EDGE ( 'NONE', *, *, #88267, .F. ) ;
#29488 = CARTESIAN_POINT ( 'NONE',  ( 29.61836285113398048, -5.182350003425200136, 28.59212231372686119 ) ) ;
#29489 = EDGE_CURVE ( 'NONE', #49712, #90366, #74209, .T. ) ;
#29490 = EDGE_CURVE ( 'NONE', #35863, #54059, #44759, .T. ) ;
#29491 = B_SPLINE_CURVE_WITH_KNOTS ( 'NONE', 3,
 ( #78195, #62494, #16306, #15803, #63008, #54886 ),
 .UNSPECIFIED., .F., .F.,
 ( 4, 2, 4 ),
 ( 0.000000000000000000, 0.001380764517853245565, 0.002761529035706491129 ),
 .UNSPECIFIED. ) ;
#29492 = CARTESIAN_POINT ( 'NONE',  ( -84.50113732502067876, -24.66019654487200441, 8.947790411086115725 ) ) ;
#29493 = EDGE_CURVE ( 'NONE', #45709, #65428, #75521, .T. ) ;
#29494 = CARTESIAN_POINT ( 'NONE',  ( -130.5728709571500588, -24.66513809378597344, 8.909134979017292011 ) ) ;
#29495 = CARTESIAN_POINT ( 'NONE',  ( -39.52287095715006870, -29.50248528299804818, 1.056150453629031594 ) ) ;
#29496 = CARTESIAN_POINT ( 'NONE',  ( 20.93798385506118365, 3.901641247904229282, -1.500000000000002220 ) ) ;
#29497 = CARTESIAN_POINT ( 'NONE',  ( -112.5222218763195912, -23.48783264082478794, -1.443836473390061270 ) ) ;
#29498 = EDGE_CURVE ( 'NONE', #12184, #53220, #1234, .T. ) ;
#29499 = CARTESIAN_POINT ( 'NONE',  ( -107.5572310827927396, -23.73791477778912551, 11.05961554403170055 ) ) ;
#29500 = CARTESIAN_POINT ( 'NONE',  ( -60.92287095715005307, -23.47596703998600631, 11.44779298504227683 ) ) ;
#29501 = CARTESIAN_POINT ( 'NONE',  ( -27.25988310792305214, -0.3587747205144265483, 30.32664379231667695 ) ) ;
#29502 = CARTESIAN_POINT ( 'NONE',  ( 14.18375884139645215, 17.39688726336347102, -1.500000000000002220 ) ) ;
#29503 = VECTOR ( 'NONE', #49497, 1000.000000000000000 ) ;
#29504 = B_SPLINE_SURFACE_WITH_KNOTS ( 'NONE', 3, 3, ( 
 ( #63943, #87751, #78109, #18235 ),
 ( #64940, #57323, #16227, #70521 ),
 ( #1011, #55310, #35957, #65936 ),
 ( #49705, #82131, #57815, #19227 ),
 ( #13106, #80635, #5007, #4520 ),
 ( #66926, #88757, #50192, #73526 ),
 ( #96359, #98341, #51690, #11119 ) ),
 .UNSPECIFIED., .F., .F., .F.,
 ( 4, 3, 4 ),
 ( 4, 4 ),
 ( 0.7945040050992245861, 0.8970133687736505657, 0.9995227324480766562 ),
 ( 0.7696895860335216666, 0.7710576503773675094 ),
 .UNSPECIFIED. ) ;
#29505 = DIRECTION ( 'NONE',  ( 0.8246584009594635223, 1.154631945610162960E-14, -0.5656310827093757876 ) ) ;
#29506 = ORIENTED_EDGE ( 'NONE', *, *, #75083, .F. ) ;
#29507 = CARTESIAN_POINT ( 'NONE',  ( -72.62287095715005592, -23.48783264082478084, -1.443836473390067265 ) ) ;
#29508 = CARTESIAN_POINT ( 'NONE',  ( -19.57149217635686966, 1.386223266712492297, 11.49999999999999645 ) ) ;
#29509 = CARTESIAN_POINT ( 'NONE',  ( -42.62287095715004881, -23.47593901973091235, -1.443836447539011525 ) ) ;
#29510 = CARTESIAN_POINT ( 'NONE',  ( -119.5562042904833930, -23.47593901973091235, -1.443836447538997536 ) ) ;
#29511 = EDGE_CURVE ( 'NONE', #79117, #83628, #52100, .T. ) ;
#29512 = ORIENTED_EDGE ( 'NONE', *, *, #56915, .F. ) ;
#29513 = CARTESIAN_POINT ( 'NONE',  ( -88.55825211740739178, -23.73791477778912196, 11.05961554403170588 ) ) ;
#29514 = CARTESIAN_POINT ( 'NONE',  ( -108.5228709571501042, -24.66019654487200441, 8.947790411086113949 ) ) ;
#29515 = CARTESIAN_POINT ( 'NONE',  ( -90.93551152535891902, -25.12049752546737480, 2.832404795212227100 ) ) ;
#29516 = CARTESIAN_POINT ( 'NONE',  ( -26.73206948527849747, -24.64631784552947380, 7.985388846607621716 ) ) ;
#29517 = CARTESIAN_POINT ( 'NONE',  ( -14.27994306655487300, -13.59162091658854798, -1.500000000000002220 ) ) ;
#29518 = EDGE_LOOP ( 'NONE', ( #30417, #70643, #4524, #17903 ) ) ;
#29519 = VECTOR ( 'NONE', #45402, 1000.000000000000000 ) ;
#29520 = AXIS2_PLACEMENT_3D ( 'NONE', #41550, #94821, #57777 ) ;
#29521 = LINE ( 'NONE', #60500, #31054 ) ;
#29522 = CYLINDRICAL_SURFACE ( 'NONE', #33422, 0.8500000000000017542 ) ;
#29523 = APPROVAL_ROLE ( '' ) ;
#29524 = ORIENTED_EDGE ( 'NONE', *, *, #95888, .T. ) ;
#29525 = DIRECTION ( 'NONE',  ( 0.000000000000000000, 0.000000000000000000, -1.000000000000000000 ) ) ;
#29526 = CARTESIAN_POINT ( 'NONE',  ( -45.62287095715005592, -23.48786465467240703, 11.44779295918255002 ) ) ;
#29527 = CARTESIAN_POINT ( 'NONE',  ( -55.59975228423683546, -24.15503026093915295, -0.2815557561904505901 ) ) ;
#29528 = CARTESIAN_POINT ( 'NONE',  ( -50.62287095715005592, -24.99156045073392463, 7.747789690856161648 ) ) ;
#29529 = CARTESIAN_POINT ( 'NONE',  ( -49.52287095715006160, -24.64965694238406613, 8.947790433994203596 ) ) ;
#29530 = B_SPLINE_CURVE_WITH_KNOTS ( 'NONE', 3,
 ( #85055, #17047, #2848, #3844 ),
 .UNSPECIFIED., .F., .F.,
 ( 4, 4 ),
 ( 0.4508219208986671278, 0.4598283521707824950 ),
 .UNSPECIFIED. ) ;
#29531 = DIRECTION ( 'NONE',  ( 0.000000000000000000, 1.000000000000000000, 0.000000000000000000 ) ) ;
#29532 = DIRECTION ( 'NONE',  ( -0.000000000000000000, -0.000000000000000000, -1.000000000000000000 ) ) ;
#29533 = CARTESIAN_POINT ( 'NONE',  ( -0.003041637939312698616, 19.98351707251910980, 11.49999999999998934 ) ) ;
#29534 = ADVANCED_FACE ( 'NONE', ( #97535 ), #5400, .T. ) ;
#29535 = B_SPLINE_CURVE_WITH_KNOTS ( 'NONE', 3,
 ( #29509, #4694, #27533, #74203 ),
 .UNSPECIFIED., .F., .F.,
 ( 4, 4 ),
 ( 0.1198715217971635938, 0.1288779530692791553 ),
 .UNSPECIFIED. ) ;
#29536 = CARTESIAN_POINT ( 'NONE',  ( -123.5228709571501184, -24.66019654487200441, 8.947790411086105067 ) ) ;
#29537 = CARTESIAN_POINT ( 'NONE',  ( -51.69697151907276123, -25.28137579932158729, 4.089352667124304119 ) ) ;
#29538 = VERTEX_POINT ( 'NONE', #38632 ) ;
#29539 = DIRECTION ( 'NONE',  ( -0.000000000000000000, 0.000000000000000000, -1.000000000000000000 ) ) ;
#29540 = ADVANCED_FACE ( 'NONE', ( #54373, #75 ), #80692, .T. ) ;
#29541 = AXIS2_PLACEMENT_3D ( 'NONE', #45006, #75925, #38869 ) ;
#29543 = CARTESIAN_POINT ( 'NONE',  ( -15.82668884360736961, -6.475225279485576024, 42.07822029717483758 ) ) ;
#29542 = LOCAL_TIME ( 0, 54, 15.00000000000000000, #80588 ) ;
#29544 = CARTESIAN_POINT ( 'NONE',  ( -80.49583835628830286, -24.83644354573579349, 8.397322867130094792 ) ) ;
#29545 = CARTESIAN_POINT ( 'NONE',  ( -81.55620429048337883, -23.48783264082478084, -1.443836473390065933 ) ) ;
#29546 = CARTESIAN_POINT ( 'NONE',  ( -114.5228709571500616, -29.50250243563736774, 8.947779886222136270 ) ) ;
#29547 = ADVANCED_FACE ( 'NONE', ( #54875 ), #7521, .T. ) ;
#29548 = CARTESIAN_POINT ( 'NONE',  ( 0.1645010273463760886, 1.417169167140627906, 0.3687607960183699740 ) ) ;
#29549 = CARTESIAN_POINT ( 'NONE',  ( -1.456683411003494966, -6.376774720514415407, 19.95737465391042775 ) ) ;
#29550 = LINE ( 'NONE', #53407, #90037 ) ;
#29551 = ADVANCED_FACE ( 'NONE', ( #21889 ), #36180, .T. ) ;
#29552 = CARTESIAN_POINT ( 'NONE',  ( 5.328346181807287252, -6.376774720514418959, 20.81670806933143680 ) ) ;
#29553 = VERTEX_POINT ( 'NONE', #78185 ) ;
#29554 = CARTESIAN_POINT ( 'NONE',  ( -13.42616926349082895, -15.17935092467416069, -1.500000000000002220 ) ) ;
#29555 = VECTOR ( 'NONE', #61570, 1000.000000000000114 ) ;
#29556 = CARTESIAN_POINT ( 'NONE',  ( -122.6271156531370394, -23.48783264082477373, -1.443836473390087471 ) ) ;
#29557 = PLANE ( 'NONE',  #7970 ) ;
#29558 = CYLINDRICAL_SURFACE ( 'NONE', #73572, 251.9358649670780892 ) ;
#29559 = VERTEX_POINT ( 'NONE', #94926 ) ;
#29560 = CARTESIAN_POINT ( 'NONE',  ( 8.500000000000000000, -0.9000000000000000222, 3.750000000000000000 ) ) ;
#29561 = CARTESIAN_POINT ( 'NONE',  ( -63.62287095715002749, -23.94994826722514958, -0.6494450866351725304 ) ) ;
#29562 = CARTESIAN_POINT ( 'NONE',  ( 9.271505649751263789, 17.87650053469100087, -1.500000000000002220 ) ) ;
#29563 = CARTESIAN_POINT ( 'NONE',  ( -5.931750313267273533, -20.21149935180699231, 11.49999999999999645 ) ) ;
#29564 = B_SPLINE_CURVE_WITH_KNOTS ( 'NONE', 3,
 ( #10493, #49575, #41453, #33834 ),
 .UNSPECIFIED., .F., .F.,
 ( 4, 4 ),
 ( 0.4100787516764388130, 0.4190851829485544022 ),
 .UNSPECIFIED. ) ;
#29566 = CARTESIAN_POINT ( 'NONE',  ( -0.02075734969026423599, 6.475225279485573360, -0.08597719988137648983 ) ) ;
#29565 = SHELL_BASED_SURFACE_MODEL ( 'NONE', ( #77601, #64681 ) );
#29567 = CARTESIAN_POINT ( 'NONE',  ( -19.11006845027251799, 11.06304553819242642, -1.500000000000002220 ) ) ;
#29569 = CARTESIAN_POINT ( 'NONE',  ( -1.764913036440812322, 20.45846032914734280, 11.49999999999998934 ) ) ;
#29568 = PRODUCT_DEFINITION ( 'UNKNOWN', '', #55421, #14436 ) ;
#29570 = DIRECTION ( 'NONE',  ( -0.000000000000000000, -1.000000000000000000, -0.000000000000000000 ) ) ;
#29571 = VECTOR ( 'NONE', #29133, 1000.000000000000000 ) ;
#29572 = CARTESIAN_POINT ( 'NONE',  ( -59.52287095715006160, -24.64898659630528854, 1.056161002820822592 ) ) ;
#29573 = ORIENTED_EDGE ( 'NONE', *, *, #96413, .F. ) ;
#29574 = CARTESIAN_POINT ( 'NONE',  ( -123.6228709571500559, -29.50250243563736774, 8.947779886222134493 ) ) ;
#29575 = EDGE_LOOP ( 'NONE', ( #84246, #87085, #72816, #19842 ) ) ;
#29576 = CARTESIAN_POINT ( 'NONE',  ( -83.52287095715006160, -23.47596703998600631, 11.44779298504228571 ) ) ;
#29577 = CARTESIAN_POINT ( 'NONE',  ( -64.58953762381672448, -24.64965694238407323, 8.947790433994656567 ) ) ;
#29578 = ORIENTED_EDGE ( 'NONE', *, *, #4094, .T. ) ;
#29579 = EDGE_LOOP ( 'NONE', ( #71040, #97651, #21496, #5904 ) ) ;
#29580 = CARTESIAN_POINT ( 'NONE',  ( -118.6228709571500701, -23.94994826722515668, -0.6494450866351694218 ) ) ;
#29581 = FACE_OUTER_BOUND ( 'NONE', #49974, .T. ) ;
#29582 = CARTESIAN_POINT ( 'NONE',  ( -76.52212344122790455, -23.48783264082477373, -1.443836473390089026 ) ) ;
#29583 = CARTESIAN_POINT ( 'NONE',  ( 11.79242832063081892, -16.95861370568002613, -1.500000000000002220 ) ) ;
#29584 = CARTESIAN_POINT ( 'NONE',  ( 5.819084965910729323, 20.79142713412266730, 11.49999999999999645 ) ) ;
#29585 = ORIENTED_EDGE ( 'NONE', *, *, #13711, .T. ) ;
#29586 = DIRECTION ( 'NONE',  ( 4.015954566446630556E-15, -1.000000000000000000, 1.297050502119899750E-15 ) ) ;
#29587 = CARTESIAN_POINT ( 'NONE',  ( -56.62287095715005592, -23.47593901973091235, -1.443836447539007972 ) ) ;
#29588 = CARTESIAN_POINT ( 'NONE',  ( 13.91197278145025074, 17.48688927191260234, -1.500000000000002220 ) ) ;
#29589 = CARTESIAN_POINT ( 'NONE',  ( -48.58953762381672448, -23.48786465467241058, 11.44779295918254824 ) ) ;
#29590 = CARTESIAN_POINT ( 'NONE',  ( 0.3910256410256394144, -6.376774720514411854, 19.63681891025641235 ) ) ;
#29591 = ORIENTED_EDGE ( 'NONE', *, *, #58050, .T. ) ;
#29592 = CARTESIAN_POINT ( 'NONE',  ( -104.6228709571500559, -29.50250786944525672, 11.44777988621623166 ) ) ;
#29593 = CARTESIAN_POINT ( 'NONE',  ( -49.62827599070762830, -24.51419770103158413, 9.386484678747189392 ) ) ;
#29594 = AXIS2_PLACEMENT_3D ( 'NONE', #2721, #33661, #95557 ) ;
#29595 = CARTESIAN_POINT ( 'NONE',  ( 20.89859092893058801, 0.06103081833375877813, 11.49999999999998934 ) ) ;
#29596 = ORIENTED_EDGE ( 'NONE', *, *, #32113, .F. ) ;
#29598 = VERTEX_POINT ( 'NONE', #72107 ) ;
#29597 = CARTESIAN_POINT ( 'NONE',  ( -67.62720759924459912, -24.51419770103159124, 9.386484678747168076 ) ) ;
#29599 = ORIENTED_EDGE ( 'NONE', *, *, #77885, .F. ) ;
#29600 = CARTESIAN_POINT ( 'NONE',  ( -109.5138029155384203, -24.51419770103157347, 9.386484678747171628 ) ) ;
#29601 = CARTESIAN_POINT ( 'NONE',  ( -0.2625952501129409367, 21.13516572482953748, -1.500000000000002220 ) ) ;
#29602 = ORIENTED_EDGE ( 'NONE', *, *, #62396, .F. ) ;
#29603 = CARTESIAN_POINT ( 'NONE',  ( -123.2228709571500502, -23.47596703998600631, 11.44779298504227860 ) ) ;
#29604 = CARTESIAN_POINT ( 'NONE',  ( -99.69221343823950576, -25.26221271103905153, 6.884718109595215019 ) ) ;
#29605 = CARTESIAN_POINT ( 'NONE',  ( 21.63681353182189682, 2.665401433100548889, -1.500000000000002220 ) ) ;
#29606 = DIRECTION ( 'NONE',  ( -0.000000000000000000, 2.173523156925979552E-06, -0.9999999999976378895 ) ) ;
#29607 = CARTESIAN_POINT ( 'NONE',  ( -86.52287095715006160, -29.50250786944525672, 11.44777988621623344 ) ) ;
#29608 = CARTESIAN_POINT ( 'NONE',  ( 7.433267315672343223, -6.376774720514418959, 20.43888261666079842 ) ) ;
#29609 = CARTESIAN_POINT ( 'NONE',  ( 14.84582651547613352, 15.88809324551894520, -1.500000000000002220 ) ) ;
#29610 = CARTESIAN_POINT ( 'NONE',  ( -79.53598664403750718, -25.10472966370973325, 7.258571028815275383 ) ) ;
#29611 = EDGE_CURVE ( 'NONE', #46585, #34762, #64515, .T. ) ;
#29613 = VERTEX_POINT ( 'NONE', #95429 ) ;
#29612 = CARTESIAN_POINT ( 'NONE',  ( -21.16112330106665240, 7.131417522999676351, 11.49999999999999645 ) ) ;
#29614 = CARTESIAN_POINT ( 'NONE',  ( -116.5562042904834215, -23.47593901973091235, -1.443836447538997536 ) ) ;
#29615 = DIRECTION ( 'NONE',  ( 1.000000000000000000, -0.000000000000000000, -0.000000000000000000 ) ) ;
#29616 = CARTESIAN_POINT ( 'NONE',  ( 31.16918082143019220, -5.911085521256299380, -1.357342440710215481 ) ) ;
#29617 = ORIENTED_EDGE ( 'NONE', *, *, #30266, .F. ) ;
#29618 = ORIENTED_EDGE ( 'NONE', *, *, #63106, .F. ) ;
#29619 = VECTOR ( 'NONE', #47271, 1000.000000000000000 ) ;
#29620 = B_SPLINE_CURVE_WITH_KNOTS ( 'NONE', 3,
 ( #68943, #74558, #28883, #6547, #68446, #84158, #59847, #66967, #97879, #14649, #37993, #82665, #44115, #75043, #5539 ),
 .UNSPECIFIED., .F., .F.,
 ( 4, 1, 1, 1, 1, 1, 1, 1, 1, 1, 1, 1, 4 ),
 ( 0.000000000000000000, 0.08415201884431637580, 0.1665323202984579920, 0.2488363311465297822, 0.3312461454872601685, 0.4129571090216147544, 0.4904942776695643825, 0.5661557919819225626, 0.6399873346864677348, 0.7167654882718510478, 0.8021439047100968889, 0.8958332007101900141, 1.000000000000000000 ),
 .UNSPECIFIED. ) ;
#29621 = ORIENTED_EDGE ( 'NONE', *, *, #18044, .F. ) ;
#29622 = CARTESIAN_POINT ( 'NONE',  ( 15.88337727998148985, 12.78846505907953279, -1.500000000000002220 ) ) ;
#29623 = EDGE_CURVE ( 'NONE', #73093, #58493, #60546, .T. ) ;
#29624 = CARTESIAN_POINT ( 'NONE',  ( -120.6228709571500417, -24.99156045073393528, 7.747789690856161648 ) ) ;
#29625 = CARTESIAN_POINT ( 'NONE',  ( 15.88363568188429653, -14.04911357082368006, 11.49999999999998934 ) ) ;
#29626 = DIRECTION ( 'NONE',  ( 0.000000000000000000, 0.000000000000000000, -1.000000000000000000 ) ) ;
#29627 = ADVANCED_FACE ( 'NONE', ( #10697 ), #16798, .F. ) ;
#29628 = CARTESIAN_POINT ( 'NONE',  ( -80.40044610398997804, -25.27791972731367309, 7.562158963542455758 ) ) ;
#29629 = CARTESIAN_POINT ( 'NONE',  ( -99.58953762381672448, -24.64898659630367916, 1.056161002820388717 ) ) ;
#29630 = CARTESIAN_POINT ( 'NONE',  ( 5.864177746775673050, -5.876774720514425177, 21.69926562011473337 ) ) ;
#29632 = CARTESIAN_POINT ( 'NONE',  ( -37.62287095715007013, -24.51387760970723662, 9.387446482453421837 ) ) ;
#29631 = AXIS2_PLACEMENT_3D ( 'NONE', #90816, #75574, #5576 ) ;
#29633 = CARTESIAN_POINT ( 'NONE',  ( -38.52287095715006870, -23.47593901973090169, -1.443836447538997092 ) ) ;
#29634 = ORIENTED_EDGE ( 'NONE', *, *, #4149, .F. ) ;
#29635 = CARTESIAN_POINT ( 'NONE',  ( 16.20606029192996900, -10.75321813762353251, 11.49999999999999645 ) ) ;
#29636 = CARTESIAN_POINT ( 'NONE',  ( -60.52287095715006160, -24.99132157543083821, 2.256160258750667502 ) ) ;
#29637 = AXIS2_PLACEMENT_3D ( 'NONE', #19117, #27246, #35362 ) ;
#29638 = EDGE_CURVE ( 'NONE', #67705, #43651, #96831, .T. ) ;
#29639 = ORIENTED_EDGE ( 'NONE', *, *, #66242, .F. ) ;
#29640 = CARTESIAN_POINT ( 'NONE',  ( 2.949406532984364393, -6.376774720514410077, 19.42899254576129664 ) ) ;
#29641 = DIRECTION ( 'NONE',  ( 0.000000000000000000, -1.000000000000000000, 0.000000000000000000 ) ) ;
#29642 = DIRECTION ( 'NONE',  ( -0.6837407958605439262, 0.000000000000000000, 0.7297249646791521549 ) ) ;
#29643 = DIRECTION ( 'NONE',  ( -0.000000000000000000, 0.5420701495772373146, 0.8403332392196035672 ) ) ;
#29644 = CARTESIAN_POINT ( 'NONE',  ( -15.21066300689680872, 12.40131300380995860, -1.500000000000002220 ) ) ;
#29645 = B_SPLINE_SURFACE_WITH_KNOTS ( 'NONE', 3, 3, ( 
 ( #88806, #73083, #65988, #66490 ),
 ( #26399, #49754, #19271, #81685 ),
 ( #3074, #88301, #4064, #50243 ),
 ( #87798, #18772, #3569, #17787 ),
 ( #56867, #12158, #34013, #42640 ),
 ( #72580, #2568, #41132, #64989 ),
 ( #18284, #48750, #11171, #79673 ) ),
 .UNSPECIFIED., .F., .F., .F.,
 ( 4, 3, 4 ),
 ( 4, 4 ),
 ( 0.2469299128580444980, 0.4952425859456087709, 0.7435552590331729883 ),
 ( 0.02428983952429602036, 0.1659897170784108700 ),
 .UNSPECIFIED. ) ;
#29646 = DIRECTION ( 'NONE',  ( 0.000000000000000000, -2.173523156925980399E-06, 0.9999999999976378895 ) ) ;
#29647 = ORIENTED_EDGE ( 'NONE', *, *, #67688, .T. ) ;
#29648 = CARTESIAN_POINT ( 'NONE',  ( 20.54099941694853726, 6.510794959084822864, 11.49999999999998934 ) ) ;
#29649 = CARTESIAN_POINT ( 'NONE',  ( -33.49675094381932894, -24.15620529776627379, 10.23563542870661536 ) ) ;
#29650 = CARTESIAN_POINT ( 'NONE',  ( -96.52287095715010423, -23.48783264082477018, -1.443836473390086139 ) ) ;
#29651 = CARTESIAN_POINT ( 'NONE',  ( 282.9764569301858046, 0.3587747205144265483, 20.79159422840526616 ) ) ;
#29652 = CARTESIAN_POINT ( 'NONE',  ( -99.84936175820153892, -25.27473256197501783, 3.453118245436027856 ) ) ;
#29653 = CARTESIAN_POINT ( 'NONE',  ( -8.820007276677138464, 21.28423624206370945, -1.500000000000002220 ) ) ;
#29654 = DATE_AND_TIME ( #93537, #89460 ) ;
#29655 = CARTESIAN_POINT ( 'NONE',  ( -93.55476215406292795, -23.96119346886881019, -0.6495511937832080251 ) ) ;
#29656 = CARTESIAN_POINT ( 'NONE',  ( -129.5228709571500758, -29.50250243563736774, 8.947779886222132717 ) ) ;
#29657 = CARTESIAN_POINT ( 'NONE',  ( 20.05498121024909253, 1.910150955369836812, 11.49999999999999645 ) ) ;
#29658 = CARTESIAN_POINT ( 'NONE',  ( -8.499999999999987566, 19.99999999999999289, 2.100000000000000089 ) ) ;
#29659 = CARTESIAN_POINT ( 'NONE',  ( -91.52287095715013265, -23.96127896941632685, -0.6493128931038013585 ) ) ;
#29660 = CARTESIAN_POINT ( 'NONE',  ( -82.62287095715005592, -29.50250243563736774, 8.947779886222141599 ) ) ;
#29661 = CARTESIAN_POINT ( 'NONE',  ( -2.499999999999993339, 4.999999999999997335, 0.000000000000000000 ) ) ;
#29662 = CARTESIAN_POINT ( 'NONE',  ( -110.3346797185884327, -25.29779155363456056, 3.293942871399098138 ) ) ;
#29663 = EDGE_CURVE ( 'NONE', #83541, #39939, #57393, .T. ) ;
#29664 = CARTESIAN_POINT ( 'NONE',  ( 0.1862606309321278575, -19.90735222434816976, 11.49999999999998934 ) ) ;
#29665 = AXIS2_PLACEMENT_3D ( 'NONE', #49232, #3049, #64470 ) ;
#29666 = CARTESIAN_POINT ( 'NONE',  ( -97.52287095715006160, -23.48786465467241769, 11.44779295918254114 ) ) ;
#29667 = CARTESIAN_POINT ( 'NONE',  ( 19.60560811685724403, 2.727087469661350738, -1.500000000000002220 ) ) ;
#29668 = CARTESIAN_POINT ( 'NONE',  ( -126.6242556467910845, -24.15620529776629510, 10.23563542870658871 ) ) ;
#29669 = EDGE_CURVE ( 'NONE', #58438, #4006, #83529, .T. ) ;
#29670 = VECTOR ( 'NONE', #44915, 1000.000000000000000 ) ;
#29671 = UNCERTAINTY_MEASURE_WITH_UNIT (LENGTH_MEASURE( 1.000000000000000082E-05 ), #46529, 'distance_accuracy_value', 'NONE');
#29672 = CARTESIAN_POINT ( 'NONE',  ( -110.5228709571500616, -23.84081130425355610, 10.88220057483161440 ) ) ;
#29673 = CARTESIAN_POINT ( 'NONE',  ( -1.967852706420949005, -6.376774720514408301, 19.18381548539530357 ) ) ;
#29674 = CARTESIAN_POINT ( 'NONE',  ( -20.26430336558559020, 4.098603726722801710, 11.49999999999999645 ) ) ;
#29675 = CARTESIAN_POINT ( 'NONE',  ( -98.52287095715006160, -24.64898659630368272, 1.056161002820829697 ) ) ;
#29676 = EDGE_CURVE ( 'NONE', #44716, #12095, #8696, .T. ) ;
#29677 = CARTESIAN_POINT ( 'NONE',  ( 30.46555845599590029, 5.356774720514427379, 2.040766579062852415 ) ) ;
#29678 = CARTESIAN_POINT ( 'NONE',  ( -49.59985430115347071, -25.25138735060574646, 5.484775612577745818 ) ) ;
#29680 = ADVANCED_FACE ( 'NONE', ( #55377 ), #32527, .F. ) ;
#29679 = CARTESIAN_POINT ( 'NONE',  ( 4.564784964189898098, -22.25151590922551748, 11.49999999999999645 ) ) ;
#29681 = VERTEX_POINT ( 'NONE', #10194 ) ;
#29682 = CARTESIAN_POINT ( 'NONE',  ( -78.62287095715004170, -24.65952944569304606, 1.056160979905698349 ) ) ;
#29683 = CARTESIAN_POINT ( 'NONE',  ( 30.63256949310621735, 4.401217678701063285, 28.01131607762999565 ) ) ;
#29684 = CARTESIAN_POINT ( 'NONE',  ( -15.75104486599040321, 12.61009050114280861, 11.49999999999998934 ) ) ;
#29685 = CARTESIAN_POINT ( 'NONE',  ( -63.55959536319858927, -23.73766607897669445, -1.055555164236456900 ) ) ;
#29686 = FACE_OUTER_BOUND ( 'NONE', #71253, .T. ) ;
#29687 = ORIENTED_EDGE ( 'NONE', *, *, #54019, .F. ) ;
#29688 = ORIENTED_EDGE ( 'NONE', *, *, #45875, .F. ) ;
#29689 = AXIS2_PLACEMENT_3D ( 'NONE', #97797, #45029, #75948 ) ;
#29690 = CARTESIAN_POINT ( 'NONE',  ( 0.3180806761505774460, -6.376774720514415407, 20.02963804100705403 ) ) ;
#29691 = CARTESIAN_POINT ( 'NONE',  ( 22.85676281555306844, 1.471244944367766649, -1.500000000000002220 ) ) ;
#29692 = PLANE ( 'NONE',  #24346 ) ;
#29693 = CARTESIAN_POINT ( 'NONE',  ( -10.14273968512601520, 19.10955606681249463, -1.500000000000002220 ) ) ;
#29694 = LINE ( 'NONE', #75359, #17190 ) ;
#29695 = CARTESIAN_POINT ( 'NONE',  ( -112.6228709571500559, -23.47596703998600631, 11.44779298504227860 ) ) ;
#29696 = CARTESIAN_POINT ( 'NONE',  ( -8.531171415479239073, -19.09552649099111221, 11.49999999999999645 ) ) ;
#29697 = ORIENTED_EDGE ( 'NONE', *, *, #92934, .F. ) ;
#29698 = CARTESIAN_POINT ( 'NONE',  ( -28.04192716165177401, -24.82017564189413861, 2.322794568040253083 ) ) ;
#29699 = CARTESIAN_POINT ( 'NONE',  ( 0.3405503412851532130, 21.98688381012616233, -1.500000000000002220 ) ) ;
#29700 = EDGE_CURVE ( 'NONE', #14119, #6499, #95019, .T. ) ;
#29701 = CARTESIAN_POINT ( 'NONE',  ( -105.5874363681110140, -24.73531770709095312, 8.716586749053508498 ) ) ;
#29702 = CARTESIAN_POINT ( 'NONE',  ( -27.68651082257923335, -25.21724994476180015, 7.605671628963411202 ) ) ;
#29703 = VECTOR ( 'NONE', #48907, 1000.000000000000114 ) ;
#29704 = VERTEX_POINT ( 'NONE', #90811 ) ;
#29705 = FACE_OUTER_BOUND ( 'NONE', #98713, .T. ) ;
#29706 = CARTESIAN_POINT ( 'NONE',  ( -90.50111960292845481, -24.83644354573578994, 8.397322867130100121 ) ) ;
#29707 = ORIENTED_EDGE ( 'NONE', *, *, #32939, .T. ) ;
#29708 = DIRECTION ( 'NONE',  ( 1.000000000000000000, 0.000000000000000000, 0.000000000000000000 ) ) ;
#29709 = EDGE_CURVE ( 'NONE', #15989, #64340, #66509, .T. ) ;
#29710 = VERTEX_POINT ( 'NONE', #58379 ) ;
#29711 = AXIS2_PLACEMENT_3D ( 'NONE', #64998, #4071, #42151 ) ;
#29712 = ORIENTED_EDGE ( 'NONE', *, *, #71467, .T. ) ;
#29713 = CARTESIAN_POINT ( 'NONE',  ( -71.63517953107638903, -24.15620529776628445, 10.23563542870660115 ) ) ;
#29714 = CARTESIAN_POINT ( 'NONE',  ( -101.6521089408578007, -25.27404798564288058, 3.606142184538064566 ) ) ;
#29715 = CARTESIAN_POINT ( 'NONE',  ( -104.5599248761161562, -23.48786465467241413, 11.44779295918254469 ) ) ;
#29716 = CARTESIAN_POINT ( 'NONE',  ( 20.39576089869593289, -0.2533167397448486957, -1.500000000000002220 ) ) ;
#29717 = ORIENTED_EDGE ( 'NONE', *, *, #19127, .T. ) ;
#29718 = FACE_OUTER_BOUND ( 'NONE', #3641, .T. ) ;
#29719 = EDGE_CURVE ( 'NONE', #18192, #36941, #59877, .T. ) ;
#29720 = DIRECTION ( 'NONE',  ( 0.5656310827093757876, 0.8246584009594636333, 1.161164194647626634E-16 ) ) ;
#29721 = ADVANCED_FACE ( 'NONE', ( #5571 ), #96916, .T. ) ;
#29722 = CARTESIAN_POINT ( 'NONE',  ( -4.243469080022288509, -6.376774720514411854, 19.94806476610987644 ) ) ;
#29723 = CARTESIAN_POINT ( 'NONE',  ( -91.52287095715004739, -24.50216790748205042, 0.6166512839542547253 ) ) ;
#29724 = ORIENTED_EDGE ( 'NONE', *, *, #64631, .F. ) ;
#29725 = CARTESIAN_POINT ( 'NONE',  ( 3.509873074917118085, 0.3587747205144265483, 29.15869884040363758 ) ) ;
#29726 = CARTESIAN_POINT ( 'NONE',  ( -29.74590468580106872, -25.26247595756167286, 6.038516002892558632 ) ) ;
#29727 = CARTESIAN_POINT ( 'NONE',  ( 6.705275102110877405, 19.67741782454948662, -1.500000000000002220 ) ) ;
#29728 = ORIENTED_EDGE ( 'NONE', *, *, #96526, .F. ) ;
#29730 = ORIENTED_EDGE ( 'NONE', *, *, #2474, .F. ) ;
#29729 = CARTESIAN_POINT ( 'NONE',  ( -54.62287095715005592, -23.47593901973091235, -1.443836447539009749 ) ) ;
#29731 = B_SPLINE_SURFACE_WITH_KNOTS ( 'NONE', 3, 3, ( 
 ( #78423, #77416, #23128, #54117 ),
 ( #7920, #62226, #23631, #54605 ),
 ( #811, #8920, #78922, #85540 ),
 ( #70830, #32258, #63228, #55616 ),
 ( #16024, #94150, #86544, #17031 ),
 ( #47997, #9415, #26656, #87551 ),
 ( #89056, #42887, #49503, #40875 ) ),
 .UNSPECIFIED., .F., .F., .F.,
 ( 4, 3, 4 ),
 ( 4, 4 ),
 ( 0.7945040050992246972, 0.8970133687736503436, 0.9995227324480758790 ),
 ( 0.3595853728713703235, 0.3607641058962429148 ),
 .UNSPECIFIED. ) ;
#29732 = CARTESIAN_POINT ( 'NONE',  ( -68.52287095715011844, -24.33927499327855060, 9.819080762295813614 ) ) ;
#29733 = VERTEX_POINT ( 'NONE', #73103 ) ;
#29734 = ORIENTED_EDGE ( 'NONE', *, *, #23637, .T. ) ;
#29735 = DIRECTION ( 'NONE',  ( 0.000000000000000000, 0.000000000000000000, 1.000000000000000000 ) ) ;
#29736 = CARTESIAN_POINT ( 'NONE',  ( -92.62287095715005592, -24.66019654487199730, 8.947790411086124607 ) ) ;
#29737 = B_SPLINE_CURVE_WITH_KNOTS ( 'NONE', 3,
 ( #30909, #46651, #60875, #69478 ),
 .UNSPECIFIED., .F., .F.,
 ( 4, 4 ),
 ( 0.000000000000000000, 9.999999999998897304E-05 ),
 .UNSPECIFIED. ) ;
#29738 = CARTESIAN_POINT ( 'NONE',  ( -64.52287095715007581, -23.96177878511308279, 10.65340807706329684 ) ) ;
#29739 = CARTESIAN_POINT ( 'NONE',  ( -100.4498239493576506, -25.25419554228399832, 7.563173735396891750 ) ) ;
#29740 = DIRECTION ( 'NONE',  ( 3.773278334444167608E-23, -1.000000000000000000, 0.000000000000000000 ) ) ;
#29741 = LINE ( 'NONE', #62202, #5963 ) ;
#29742 = EDGE_CURVE ( 'NONE', #28007, #58159, #36516, .T. ) ;
#29744 = ORIENTED_EDGE ( 'NONE', *, *, #98722, .F. ) ;
#29743 = CARTESIAN_POINT ( 'NONE',  ( -11.88820881604258339, -18.65297325734525913, 11.49999999999999645 ) ) ;
#29745 = CARTESIAN_POINT ( 'NONE',  ( -44.62287095715004881, -24.66019654487198665, 8.947790411086135265 ) ) ;
#29746 = VECTOR ( 'NONE', #18888, 1000.000000000000114 ) ;
#29747 = CARTESIAN_POINT ( 'NONE',  ( 22.64978874513612439, 0.4204215919581203442, -1.500000000000002220 ) ) ;
#29749 = ORIENTED_EDGE ( 'NONE', *, *, #1248, .F. ) ;
#29748 = DIRECTION ( 'NONE',  ( 0.000000000000000000, -1.000000000000000000, 0.000000000000000000 ) ) ;
#29750 = CIRCLE ( 'NONE', #23286, 252.4458649670781085 ) ;
#29751 = VERTEX_POINT ( 'NONE', #89812 ) ;
#29752 = DIRECTION ( 'NONE',  ( 0.000000000000000000, 0.000000000000000000, 1.000000000000000000 ) ) ;
#29753 = EDGE_CURVE ( 'NONE', #98936, #50456, #28909, .T. ) ;
#29754 = CARTESIAN_POINT ( 'NONE',  ( -11.28321777122536140, 16.66956161807075887, -1.500000000000002220 ) ) ;
#29755 = EDGE_CURVE ( 'NONE', #55213, #89773, #51255, .T. ) ;
#29756 = CARTESIAN_POINT ( 'NONE',  ( -19.06493965993949402, -22.58124009362228435, -1.443836447538997536 ) ) ;
#29757 = VERTEX_POINT ( 'NONE', #19787 ) ;
#29758 = CARTESIAN_POINT ( 'NONE',  ( -24.90875734969025501, -6.376774720514426953, 26.43402280011862615 ) ) ;
#29759 = CARTESIAN_POINT ( 'NONE',  ( -0.4079105510268487000, 22.33655531192813370, -1.500000000000002220 ) ) ;
#29760 = EDGE_CURVE ( 'NONE', #95000, #7634, #53358, .T. ) ;
#29761 = ORIENTED_EDGE ( 'NONE', *, *, #37889, .T. ) ;
#29762 = VERTEX_POINT ( 'NONE', #12177 ) ;
#29763 = LINE ( 'NONE', #68829, #28697 ) ;
#29764 = CARTESIAN_POINT ( 'NONE',  ( -81.67164698139400514, -25.15124539077181609, 6.939751081170221880 ) ) ;
#29765 = CARTESIAN_POINT ( 'NONE',  ( -49.74369414166532977, -29.50249372652338664, 4.940868828539293212 ) ) ;
#29766 = DIRECTION ( 'NONE',  ( 0.000000000000000000, 0.000000000000000000, 1.000000000000000000 ) ) ;
#29767 = EDGE_CURVE ( 'NONE', #95664, #56245, #30176, .T. ) ;
#29768 = CARTESIAN_POINT ( 'NONE',  ( -80.55620429048337883, -24.99156044556201905, 7.747789690856173195 ) ) ;
#29769 = CARTESIAN_POINT ( 'NONE',  ( 11.58774116221665729, 15.72987433093905096, -1.500000000000002220 ) ) ;
#29770 = CARTESIAN_POINT ( 'NONE',  ( -47.52287095715003318, -23.73907113217730469, -1.053371485780176142 ) ) ;
#29771 = CARTESIAN_POINT ( 'NONE',  ( -16.68621059303058018, 13.52761613308161870, -1.500000000000002220 ) ) ;
#29772 = CARTESIAN_POINT ( 'NONE',  ( -25.64067666839992299, -24.92775104721833657, 3.645611680657319109 ) ) ;
#29773 = CARTESIAN_POINT ( 'NONE',  ( -8.160000000000000142, 9.789768006247301813, -0.8564937190954607926 ) ) ;
#29774 = CARTESIAN_POINT ( 'NONE',  ( -34.52287095715008292, -23.94994826722564696, -0.6494450866342749151 ) ) ;
#29775 = CARTESIAN_POINT ( 'NONE',  ( -22.64140897529919272, -3.284158816904186651, -1.500000000000002220 ) ) ;
#29776 = AXIS2_PLACEMENT_3D ( 'NONE', #41025, #32405, #63880 ) ;
#29777 = PLANE ( 'NONE',  #38543 ) ;
#29778 = CARTESIAN_POINT ( 'NONE',  ( 3.509873074917118085, -0.3587747205144265483, 29.15869884040363758 ) ) ;
#29779 = CARTESIAN_POINT ( 'NONE',  ( 16.76344175524385705, -10.90933549886441156, 11.49999999999999645 ) ) ;
#29780 = CARTESIAN_POINT ( 'NONE',  ( -50.52287095715008292, -23.85196035786900026, -0.8779234886475190125 ) ) ;
#29781 = VECTOR ( 'NONE', #67238, 1000.000000000000114 ) ;
#29782 = CARTESIAN_POINT ( 'NONE',  ( -74.55412444941374872, -23.96169478059713498, 10.65365249895717881 ) ) ;
#29783 = CARTESIAN_POINT ( 'NONE',  ( -37.62287095715005592, -24.64898659630367206, 1.056161002820819261 ) ) ;
#29784 = ORIENTED_EDGE ( 'NONE', *, *, #47369, .T. ) ;
#29785 = CARTESIAN_POINT ( 'NONE',  ( -26.57207785542718170, -24.62921250442780874, 2.000914044556121762 ) ) ;
#29786 = CARTESIAN_POINT ( 'NONE',  ( -65.52287095715007581, -24.52323809116984066, 9.355190652339423707 ) ) ;
#29787 = CARTESIAN_POINT ( 'NONE',  ( -20.31635052000798325, -7.690577546848336610, -1.500000000000002220 ) ) ;
#29788 = CARTESIAN_POINT ( 'NONE',  ( -77.58953762381672448, -24.66019654487199730, 8.947790411086112172 ) ) ;
#29789 = CARTESIAN_POINT ( 'NONE',  ( 15.22544387773384500, -12.34335808662847178, -1.500000000000002220 ) ) ;
#29790 = CARTESIAN_POINT ( 'NONE',  ( -100.0958943179937961, -25.13913306373530077, 7.067219463468185303 ) ) ;
#29791 = ADVANCED_FACE ( 'NONE', ( #96928 ), #5071, .F. ) ;
#29792 = ORIENTED_EDGE ( 'NONE', *, *, #58936, .T. ) ;
#29793 = DATE_AND_TIME ( #5457, #86339 ) ;
#29794 = DIRECTION ( 'NONE',  ( -0.04174795870516300605, 0.5404601326709027598, 0.8403332392195981271 ) ) ;
#29795 = CARTESIAN_POINT ( 'NONE',  ( -47.52287095715006160, -23.47596703998600631, 11.44779298504229104 ) ) ;
#29796 = CARTESIAN_POINT ( 'NONE',  ( -20.35906544237474236, -2.577633573104691322, 11.49999999999999645 ) ) ;
#29797 = CARTESIAN_POINT ( 'NONE',  ( -23.31187512739357359, 5.965225279485572685, -17.31005501743528185 ) ) ;
#29798 = CYLINDRICAL_SURFACE ( 'NONE', #26984, 130.2784398600581710 ) ;
#29799 = ORIENTED_EDGE ( 'NONE', *, *, #3044, .T. ) ;
#29800 = LINE ( 'NONE', #99308, #83213 ) ;
#29801 = CARTESIAN_POINT ( 'NONE',  ( -39.89668141102733756, -25.28892453938336615, 3.440461006402131705 ) ) ;
#29802 = CARTESIAN_POINT ( 'NONE',  ( -101.5228709571500900, -23.48783264082477018, -1.443836473390087249 ) ) ;
#29803 = CARTESIAN_POINT ( 'NONE',  ( -4.621320343559254695, 11.49999999999999645, 0.000000000000000000 ) ) ;
#29804 = AXIS2_PLACEMENT_3D ( 'NONE', #86354, #70627, #16837 ) ;
#29805 = CARTESIAN_POINT ( 'NONE',  ( 8.971512145086524725, -7.528487854913504584, -6.499999999999999112 ) ) ;
#29806 = CARTESIAN_POINT ( 'NONE',  ( -5.338719972479099241, 22.46511350730333589, 11.49999999999999645 ) ) ;
#29807 = CARTESIAN_POINT ( 'NONE',  ( 22.80427751693360960, 0.003464389817739472934, 11.49999999999998934 ) ) ;
#29808 = CARTESIAN_POINT ( 'NONE',  ( -110.5598947927333739, -23.48786465467241413, 11.44779295918253581 ) ) ;
#29809 = VECTOR ( 'NONE', #27091, 1000.000000000000000 ) ;
#29810 = CARTESIAN_POINT ( 'NONE',  ( 26.73860345374794178, -1.682774720514426114, -1.272392034746785860 ) ) ;
#29811 = CARTESIAN_POINT ( 'NONE',  ( 1.949999999999999956, -0.1925000000000001155, -0.1925000000000000600 ) ) ;
#29812 = CARTESIAN_POINT ( 'NONE',  ( -115.5228709571500616, -25.00158670708909625, 2.256160236439166411 ) ) ;
#29813 = CARTESIAN_POINT ( 'NONE',  ( -110.5493975497841461, -24.83618233451450763, 1.606449574219537935 ) ) ;
#29814 = CARTESIAN_POINT ( 'NONE',  ( -14.06357901826416068, -16.81340526219955933, 11.49999999999998934 ) ) ;
#29815 = DIRECTION ( 'NONE',  ( 0.9940716917543757081, 0.000000000000000000, -0.1087265912856348465 ) ) ;
#29816 = EDGE_CURVE ( 'NONE', #94137, #76027, #11679, .T. ) ;
#29817 = B_SPLINE_CURVE_WITH_KNOTS ( 'NONE', 3,
 ( #66430, #51181, #27837, #88247, #87745, #18716 ),
 .UNSPECIFIED., .F., .F.,
 ( 4, 2, 4 ),
 ( 0.000000000000000000, 0.0005107898210030667376, 0.001021579642006133475 ),
 .UNSPECIFIED. ) ;
#29818 = CARTESIAN_POINT ( 'NONE',  ( -87.50769031727142533, -24.35071581493543391, 9.817618358456025263 ) ) ;
#29819 = CARTESIAN_POINT ( 'NONE',  ( -34.62287095715005592, -24.66019654487199020, 8.947790411086137041 ) ) ;
#29820 = CARTESIAN_POINT ( 'NONE',  ( -78.59205981310179823, -24.15543982623907127, -0.2315651400026641771 ) ) ;
#29821 = CARTESIAN_POINT ( 'NONE',  ( -79.62287095715005592, -23.48786465467241058, 11.44779295918254469 ) ) ;
#29822 = CARTESIAN_POINT ( 'NONE',  ( -73.62287095715005592, -23.48786465467241058, 11.44779295918254469 ) ) ;
#29823 = EDGE_LOOP ( 'NONE', ( #75131, #19746, #29212, #2816 ) ) ;
#29824 = CARTESIAN_POINT ( 'NONE',  ( 20.41236503877875563, 1.188189311754236144, -1.500000000000002220 ) ) ;
#29825 = EDGE_LOOP ( 'NONE', ( #24879, #42857, #22105, #87753 ) ) ;
#29826 = ORIENTED_EDGE ( 'NONE', *, *, #76437, .T. ) ;
#29827 = EDGE_LOOP ( 'NONE', ( #90988, #30742, #26265, #27500 ) ) ;
#29828 = B_SPLINE_CURVE_WITH_KNOTS ( 'NONE', 3,
 ( #50412, #27576, #74239, #10342, #35186, #65657, #4734, #58526 ),
 .UNSPECIFIED., .F., .F.,
 ( 4, 2, 2, 4 ),
 ( 0.09426293957327776252, 0.09592851477271921445, 0.09759408997216065251, 0.1009252403710435564 ),
 .UNSPECIFIED. ) ;
#29829 = ORIENTED_EDGE ( 'NONE', *, *, #49224, .T. ) ;
#29830 = CARTESIAN_POINT ( 'NONE',  ( 19.44587849558928738, -12.39355811350142922, -1.500000000000002220 ) ) ;
#29831 = LINE ( 'NONE', #84117, #76188 ) ;
#29832 = CARTESIAN_POINT ( 'NONE',  ( 9.769481717609929561, -17.74358427669893956, -1.500000000000002220 ) ) ;
#29833 = ORIENTED_EDGE ( 'NONE', *, *, #19167, .F. ) ;
#29834 = EDGE_CURVE ( 'NONE', #40387, #11406, #10943, .T. ) ;
#29835 = CARTESIAN_POINT ( 'NONE',  ( -29.62287096154833677, -23.39681786206389447, 11.44779298504227860 ) ) ;
#29836 = EDGE_CURVE ( 'NONE', #48360, #28254, #38518, .T. ) ;
#29837 = CARTESIAN_POINT ( 'NONE',  ( -40.67072903602026201, -25.30386692762919409, 5.536616400695820950 ) ) ;
#29838 = EDGE_CURVE ( 'NONE', #62214, #65103, #52256, .T. ) ;
#29839 = CARTESIAN_POINT ( 'NONE',  ( -115.6228709571500559, -29.50249982740957577, 7.747779886224967605 ) ) ;
#29840 = CARTESIAN_POINT ( 'NONE',  ( -99.55026156597334364, -24.35071581493543746, 9.817618358456025263 ) ) ;
#29842 = ORIENTED_EDGE ( 'NONE', *, *, #84391, .T. ) ;
#29841 = CARTESIAN_POINT ( 'NONE',  ( 6.977786103627443559, 20.27319509581574408, 11.49999999999999645 ) ) ;
#29843 = PLANE ( 'NONE',  #35515 ) ;
#29844 = CARTESIAN_POINT ( 'NONE',  ( -61.58320691632388133, -24.51419770103157347, 9.386484678747178734 ) ) ;
#29845 = ADVANCED_FACE ( 'NONE', ( #44640 ), #62367, .F. ) ;
#29846 = ORIENTED_EDGE ( 'NONE', *, *, #50529, .F. ) ;
#29847 = CARTESIAN_POINT ( 'NONE',  ( 12.98984941077313415, -16.12360325096057423, 11.49999999999998934 ) ) ;
#29849 = ORIENTED_EDGE ( 'NONE', *, *, #55639, .F. ) ;
#29848 = CARTESIAN_POINT ( 'NONE',  ( -80.55620429048339304, -23.48783264082478084, -1.443836473390065045 ) ) ;
#29850 = CARTESIAN_POINT ( 'NONE',  ( -28.52992191804173316, -24.35265584445642517, 0.6176551810875480220 ) ) ;
#29851 = ORIENTED_EDGE ( 'NONE', *, *, #9450, .T. ) ;
#29852 = CARTESIAN_POINT ( 'NONE',  ( 4.740341618695937065, -6.376774720514404748, 18.75174579344860248 ) ) ;
#29853 = VERTEX_POINT ( 'NONE', #60871 ) ;
#29854 = EDGE_CURVE ( 'NONE', #22734, #35967, #29903, .T. ) ;
#29855 = CARTESIAN_POINT ( 'NONE',  ( 21.59112034314636119, 3.954845139028329015, 11.49999999999999645 ) ) ;
#29856 = CARTESIAN_POINT ( 'NONE',  ( -91.52287095715006160, -24.65952944569304606, 1.056160979905700570 ) ) ;
#29857 = CARTESIAN_POINT ( 'NONE',  ( 8.566404662457630437, 20.85315857434707709, -1.500000000000002220 ) ) ;
#29858 = CARTESIAN_POINT ( 'NONE',  ( -5.413507703253908510, 20.27406835261982465, 11.49999999999998934 ) ) ;
#29859 = CARTESIAN_POINT ( 'NONE',  ( -78.52287095715006160, -29.50248528299804818, 1.056150453629038477 ) ) ;
#29860 = DIRECTION ( 'NONE',  ( -0.000000000000000000, 0.000000000000000000, 1.000000000000000000 ) ) ;
#29862 = EDGE_CURVE ( 'NONE', #62319, #27239, #31793, .T. ) ;
#29861 = ORIENTED_EDGE ( 'NONE', *, *, #1330, .T. ) ;
#29863 = EDGE_LOOP ( 'NONE', ( #95270, #25746, #96570, #47813 ) ) ;
#29864 = ORIENTED_EDGE ( 'NONE', *, *, #86761, .F. ) ;
#29865 = B_SPLINE_CURVE_WITH_KNOTS ( 'NONE', 3,
 ( #91587, #23057, #2137, #46418, #22067, #99194 ),
 .UNSPECIFIED., .F., .F.,
 ( 4, 2, 4 ),
 ( 0.000000000000000000, 0.001380764517854766267, 0.002761529035709532533 ),
 .UNSPECIFIED. ) ;
#29866 = CARTESIAN_POINT ( 'NONE',  ( -66.58369449947565499, -24.51314013834316441, 0.6176544820404136216 ) ) ;
#29867 = AXIS2_PLACEMENT_3D ( 'NONE', #87718, #975, #86704 ) ;
#29868 = EDGE_CURVE ( 'NONE', #29958, #24375, #99893, .T. ) ;
#29869 = CARTESIAN_POINT ( 'NONE',  ( 13.04721882220160012, 17.14300067834640373, -1.500000000000002220 ) ) ;
#29870 = CARTESIAN_POINT ( 'NONE',  ( -121.5562042904833930, -24.66019654487199730, 8.947790411086121054 ) ) ;
#29871 = ORIENTED_EDGE ( 'NONE', *, *, #38839, .T. ) ;
#29872 = CARTESIAN_POINT ( 'NONE',  ( 9.660767377612277329, -18.76748907076374095, 11.49999999999998934 ) ) ;
#29873 = CARTESIAN_POINT ( 'NONE',  ( 14.76093561896379214, -5.965225279485572685, -28.39148769130089889 ) ) ;
#29874 = DIRECTION ( 'NONE',  ( 0.000000000000000000, 1.000000000000000000, -0.000000000000000000 ) ) ;
#29875 = CARTESIAN_POINT ( 'NONE',  ( -83.63279613814142976, -24.15620529776628089, 10.23563542870660470 ) ) ;
#29876 = CARTESIAN_POINT ( 'NONE',  ( 5.550000000000004263, 0.000000000000000000, 0.000000000000000000 ) ) ;
#29877 = CARTESIAN_POINT ( 'NONE',  ( 8.160000000000000142, -6.446506136384787311, 8.876977486517731109 ) ) ;
#29878 = CARTESIAN_POINT ( 'NONE',  ( 21.58644828898399481, -4.983269013152989757, -1.500000000000002220 ) ) ;
#29879 = FACE_OUTER_BOUND ( 'NONE', #5911, .T. ) ;
#29880 = EDGE_CURVE ( 'NONE', #34688, #11149, #40060, .T. ) ;
#29881 = VECTOR ( 'NONE', #9999, 1000.000000000000000 ) ;
#29882 = ORIENTED_EDGE ( 'NONE', *, *, #75688, .T. ) ;
#29883 = CARTESIAN_POINT ( 'NONE',  ( -51.93075163254042792, -25.31633345791246725, 6.142474900134158311 ) ) ;
#29884 = CARTESIAN_POINT ( 'NONE',  ( -67.52287095715006160, -24.64898659630528854, 1.056161002820824368 ) ) ;
#29885 = DIRECTION ( 'NONE',  ( 0.000000000000000000, 0.9961946980917453232, -0.08715574274766167695 ) ) ;
#29886 = EDGE_CURVE ( 'NONE', #88628, #4409, #70238, .T. ) ;
#29887 = CARTESIAN_POINT ( 'NONE',  ( -58.55620429048337883, -23.47593901973091235, -1.443836447539007972 ) ) ;
#29888 = B_SPLINE_CURVE_WITH_KNOTS ( 'NONE', 3,
 ( #94794, #25787, #47639, #9062, #79066, #2460, #56762, #62360 ),
 .UNSPECIFIED., .F., .F.,
 ( 4, 2, 2, 4 ),
 ( -0.001240666984355838671, -0.0002401179793394966292, 0.0007604310256768454131, 0.002761529035709529498 ),
 .UNSPECIFIED. ) ;
#29889 = CARTESIAN_POINT ( 'NONE',  ( -17.22176335520693158, -9.073154711715998744, -1.500000000000002220 ) ) ;
#29890 = CARTESIAN_POINT ( 'NONE',  ( 8.370372042246325250, 19.68514866842044242, 11.49999999999998934 ) ) ;
#29891 = CARTESIAN_POINT ( 'NONE',  ( -62.63696836751751817, -24.15543982623907482, -0.2315651400026649265 ) ) ;
#29892 = FACE_OUTER_BOUND ( 'NONE', #20025, .T. ) ;
#29893 = PLANE ( 'NONE',  #6537 ) ;
#29894 = CARTESIAN_POINT ( 'NONE',  ( -0.02075734969026423599, 6.376774720514426953, -0.08597719988137648983 ) ) ;
#29895 = CARTESIAN_POINT ( 'NONE',  ( 18.72737137862276313, -12.84423604280260278, -1.500000000000002220 ) ) ;
#29896 = EDGE_LOOP ( 'NONE', ( #57078, #29916, #26662, #99937 ) ) ;
#29897 = DIRECTION ( 'NONE',  ( -3.773278334453079030E-23, 0.9999999999976377785, 2.173523156925979128E-06 ) ) ;
#29898 = CARTESIAN_POINT ( 'NONE',  ( -62.62287095715002039, -23.96177878511307568, 10.65340807706330573 ) ) ;
#29899 = CARTESIAN_POINT ( 'NONE',  ( 1.944447714513537262, -19.71154682592685958, 11.49999999999999645 ) ) ;
#29900 = FACE_OUTER_BOUND ( 'NONE', #2753, .T. ) ;
#29901 = ORIENTED_EDGE ( 'NONE', *, *, #32641, .T. ) ;
#29902 = CARTESIAN_POINT ( 'NONE',  ( -5.891303133519534718, -5.876774720514419847, 20.71116975788854475 ) ) ;
#29903 = LINE ( 'NONE', #15176, #51277 ) ;
#29904 = CARTESIAN_POINT ( 'NONE',  ( 21.43499300031224664, 3.042053824063517542, -1.500000000000002220 ) ) ;
#29905 = CARTESIAN_POINT ( 'NONE',  ( -99.62287095715005592, -24.65952944569304961, 1.056160979905702124 ) ) ;
#29906 = CARTESIAN_POINT ( 'NONE',  ( -18.22486019313910077, 6.713856318530649681, -1.500000000000002220 ) ) ;
#29907 = CARTESIAN_POINT ( 'NONE',  ( -61.62287095715004881, -24.65952944569304606, 1.056160979905695907 ) ) ;
#29908 = B_SPLINE_CURVE_WITH_KNOTS ( 'NONE', 3,
 ( #47410, #1240, #55025, #78337, #31169, #78831 ),
 .UNSPECIFIED., .F., .F.,
 ( 4, 2, 4 ),
 ( 1.570887131794176733E-05, 0.001396322306279758037, 0.002776935741241574537 ),
 .UNSPECIFIED. ) ;
#29909 = CARTESIAN_POINT ( 'NONE',  ( -129.5228709571500758, -23.47596703998600631, 11.44779298504227683 ) ) ;
#29910 = CARTESIAN_POINT ( 'NONE',  ( 10.49454761162020588, -16.79419365751139637, -1.500000000000002220 ) ) ;
#29911 = VERTEX_POINT ( 'NONE', #21282 ) ;
#29912 = AXIS2_PLACEMENT_3D ( 'NONE', #5943, #98787, #23150 ) ;
#29913 = CARTESIAN_POINT ( 'NONE',  ( -19.79944955726156763, -4.570829099900970860, 11.49999999999999645 ) ) ;
#29914 = CARTESIAN_POINT ( 'NONE',  ( -80.54148221499259819, -24.73486907724918282, 1.287355809206963908 ) ) ;
#29915 = CARTESIAN_POINT ( 'NONE',  ( 33.41145047975789595, -4.538943570064395416, -12.61568413423384172 ) ) ;
#29916 = ORIENTED_EDGE ( 'NONE', *, *, #25519, .F. ) ;
#29917 = B_SPLINE_SURFACE_WITH_KNOTS ( 'NONE', 3, 3, ( 
 ( #27375, #27866, #50216, #50711 ),
 ( #43104, #36475, #89771, #81158 ),
 ( #51709, #52209, #44096, #6024 ),
 ( #81661, #75023, #82648, #12133 ),
 ( #74048, #5030, #4547, #5522 ),
 ( #57839, #58334, #35491, #51211 ),
 ( #67438, #97382, #58824, #90267 ) ),
 .UNSPECIFIED., .F., .F., .F.,
 ( 4, 3, 4 ),
 ( 4, 4 ),
 ( 0.7945040050992233649, 0.8970133687736494554, 0.9995227324480754350 ),
 ( 0.1095218282603019622, 0.1105851153589713504 ),
 .UNSPECIFIED. ) ;
#29918 = CARTESIAN_POINT ( 'NONE',  ( -102.5109869284088120, -24.51419770103155926, 9.386484678747178734 ) ) ;
#29919 = CARTESIAN_POINT ( 'NONE',  ( -95.52287095715009002, -24.51254535375847965, 9.355368624242132114 ) ) ;
#29920 = CARTESIAN_POINT ( 'NONE',  ( -49.27237840819080361, -25.25214495137587178, 5.251752546777291641 ) ) ;
#29921 = B_SPLINE_CURVE_WITH_KNOTS ( 'NONE', 3,
 ( #93326, #77595, #16206, #1997 ),
 .UNSPECIFIED., .F., .F.,
 ( 4, 4 ),
 ( 1.392605083940956291E-05, 0.002317294749888688596 ),
 .UNSPECIFIED. ) ;
#29922 = CARTESIAN_POINT ( 'NONE',  ( -54.62287095715005592, -23.47593901973091235, -1.443836447539009749 ) ) ;
#29923 = B_SPLINE_CURVE_WITH_KNOTS ( 'NONE', 3,
 ( #57206, #893, #1903, #47079 ),
 .UNSPECIFIED., .F., .F.,
 ( 4, 4 ),
 ( 0.9011434845044391517, 0.9101499157765544634 ),
 .UNSPECIFIED. ) ;
#29924 = CARTESIAN_POINT ( 'NONE',  ( -1.001577508147789342, -5.876774720514411854, 19.87297243748311004 ) ) ;
#29925 = CARTESIAN_POINT ( 'NONE',  ( -4.751880754313710042, -19.48972053015312866, -1.500000000000002220 ) ) ;
#29926 = CARTESIAN_POINT ( 'NONE',  ( -28.58953762381673513, -23.32889918787351036, -1.443835802988293171 ) ) ;
#29927 = ORIENTED_EDGE ( 'NONE', *, *, #38650, .F. ) ;
#29928 = CARTESIAN_POINT ( 'NONE',  ( -36.52287095715006870, -24.64898659630367916, 1.056161002820819261 ) ) ;
#29929 = CARTESIAN_POINT ( 'NONE',  ( 12.20170062390598709, -19.39347807479101249, 11.49999999999999645 ) ) ;
#29930 = FACE_OUTER_BOUND ( 'NONE', #88653, .T. ) ;
#29931 = DIRECTION ( 'NONE',  ( -3.773278334444167020E-23, 1.000000000000000000, 0.000000000000000000 ) ) ;
#29932 = LINE ( 'NONE', #83217, #3061 ) ;
#29933 = CARTESIAN_POINT ( 'NONE',  ( 5.727631217150810805, -5.876774720514421624, 21.11407618546790133 ) ) ;
#29934 = AXIS2_PLACEMENT_3D ( 'NONE', #34427, #43046, #97322 ) ;
#29935 = CARTESIAN_POINT ( 'NONE',  ( -99.52764846858842418, -25.27419814425944011, 3.999772249604663710 ) ) ;
#29936 = DIRECTION ( 'NONE',  ( 3.773278334444167608E-23, -1.000000000000000000, 0.000000000000000000 ) ) ;
#29937 = EDGE_LOOP ( 'NONE', ( #5505, #38209, #46457, #68260 ) ) ;
#29938 = EDGE_CURVE ( 'NONE', #41839, #61801, #88397, .T. ) ;
#29939 = CARTESIAN_POINT ( 'NONE',  ( -20.32544160278596834, -1.370942541838689799, 11.49999999999998934 ) ) ;
#29941 = EDGE_CURVE ( 'NONE', #55186, #52365, #58222, .T. ) ;
#29940 = EDGE_LOOP ( 'NONE', ( #46807, #42177, #39094, #11299 ) ) ;
#29942 = CARTESIAN_POINT ( 'NONE',  ( 20.38051395842347802, -10.57019977742728578, 11.49999999999998934 ) ) ;
#29943 = CARTESIAN_POINT ( 'NONE',  ( -22.05275734969026047, 5.965225279485572685, 30.51402280011862089 ) ) ;
#29944 = AXIS2_PLACEMENT_3D ( 'NONE', #4912, #43969, #41992 ) ;
#29945 = ADVANCED_FACE ( 'NONE', ( #69969 ), #92301, .T. ) ;
#29946 = ORIENTED_EDGE ( 'NONE', *, *, #55967, .F. ) ;
#29947 = CARTESIAN_POINT ( 'NONE',  ( -38.62287095715005592, -24.50216790748097750, 0.6166512839513631494 ) ) ;
#29948 = EDGE_CURVE ( 'NONE', #73248, #3648, #61814, .T. ) ;
#29950 = EDGE_CURVE ( 'NONE', #89333, #62223, #83689, .T. ) ;
#29949 = CARTESIAN_POINT ( 'NONE',  ( -116.5228709571500474, -23.96177878511309345, 10.65340807706329507 ) ) ;
#29951 = CARTESIAN_POINT ( 'NONE',  ( -40.62287095715004170, -24.51163499207175178, 0.6490370598554262571 ) ) ;
#29953 = ORIENTED_EDGE ( 'NONE', *, *, #3420, .F. ) ;
#29952 = CARTESIAN_POINT ( 'NONE',  ( -20.53569570583907122, -5.550916044964551155, 11.49999999999999645 ) ) ;
#29954 = ORIENTED_EDGE ( 'NONE', *, *, #11638, .T. ) ;
#29955 = CARTESIAN_POINT ( 'NONE',  ( 8.998109643811913472, -20.30750954041392120, 11.49999999999998934 ) ) ;
#29956 = B_SPLINE_CURVE_WITH_KNOTS ( 'NONE', 3,
 ( #70680, #84402, #1174, #53968, #55466, #78771 ),
 .UNSPECIFIED., .F., .F.,
 ( 4, 2, 4 ),
 ( 0.000000000000000000, 0.001380764517854762580, 0.002761529035709525161 ),
 .UNSPECIFIED. ) ;
#29957 = CARTESIAN_POINT ( 'NONE',  ( 6.296002175621457475, 19.65409743616946514, -1.500000000000002220 ) ) ;
#29958 = VERTEX_POINT ( 'NONE', #76072 ) ;
#29959 = VERTEX_POINT ( 'NONE', #22771 ) ;
#29960 = CARTESIAN_POINT ( 'NONE',  ( -4.495793269230770939, -5.876774720514410077, 19.27714342948718595 ) ) ;
#29961 = CARTESIAN_POINT ( 'NONE',  ( 2.933277810221831761, -5.876774720514424288, 21.39432064584807947 ) ) ;
#29962 = VERTEX_POINT ( 'NONE', #53257 ) ;
#29963 = ORIENTED_EDGE ( 'NONE', *, *, #12883, .F. ) ;
#29964 = CARTESIAN_POINT ( 'NONE',  ( -127.1722388760373690, -25.27126041720325844, 4.079010001960287291 ) ) ;
#29965 = CARTESIAN_POINT ( 'NONE',  ( -2.499999999999993339, 4.999999999999997335, 2.100000000000000089 ) ) ;
#29966 = CARTESIAN_POINT ( 'NONE',  ( 12.46380520747237419, 16.70348211664046900, -1.500000000000002220 ) ) ;
#29967 = CARTESIAN_POINT ( 'NONE',  ( -8.041798833237560729, -20.28069125152608976, 11.49999999999999645 ) ) ;
#29968 = CARTESIAN_POINT ( 'NONE',  ( 22.81105451610979173, 1.684774720501991396, -18.46691820600746681 ) ) ;
#29969 = DIRECTION ( 'NONE',  ( 0.000000000000000000, -1.000000000000000000, -0.000000000000000000 ) ) ;
#29970 = CARTESIAN_POINT ( 'NONE',  ( -11.43049785330379997, -19.34545768653811493, -1.500000000000002220 ) ) ;
#29971 = DIRECTION ( 'NONE',  ( -0.000000000000000000, -1.000000000000000000, 0.000000000000000000 ) ) ;
#29972 = ORIENTED_EDGE ( 'NONE', *, *, #57170, .T. ) ;
#29973 = FACE_OUTER_BOUND ( 'NONE', #62481, .T. ) ;
#29974 = CARTESIAN_POINT ( 'NONE',  ( -57.55620429048338593, -24.65952944569304606, 1.056160979905696573 ) ) ;
#29975 = EDGE_CURVE ( 'NONE', #34855, #58437, #68476, .T. ) ;
#29976 = AXIS2_PLACEMENT_3D ( 'NONE', #15550, #25164, #31279 ) ;
#29977 = ORIENTED_EDGE ( 'NONE', *, *, #16319, .F. ) ;
#29978 = ORIENTED_EDGE ( 'NONE', *, *, #33624, .F. ) ;
#29979 = PLANE ( 'NONE',  #71734 ) ;
#29980 = VERTEX_POINT ( 'NONE', #14676 ) ;
#29981 = CARTESIAN_POINT ( 'NONE',  ( 13.79380260783658407, 16.28676726024703214, -1.500000000000002220 ) ) ;
#29982 = ORIENTED_EDGE ( 'NONE', *, *, #66132, .F. ) ;
#29983 = CARTESIAN_POINT ( 'NONE',  ( -5.895658455092926076, -5.876774720514418071, 20.50445910983877340 ) ) ;
#29984 = CARTESIAN_POINT ( 'NONE',  ( -13.78326148797977169, 15.88460234914768421, -1.500000000000002220 ) ) ;
#29985 = CARTESIAN_POINT ( 'NONE',  ( -30.59476385451626257, -24.83983788297006612, 1.633466014234818076 ) ) ;
#29986 = CARTESIAN_POINT ( 'NONE',  ( -55.62287095715005592, -23.47593901973091235, -1.443836447539007972 ) ) ;
#29987 = CARTESIAN_POINT ( 'NONE',  ( -56.52287095715006870, -29.50250786944525672, 11.44777988621623876 ) ) ;
#29988 = CARTESIAN_POINT ( 'NONE',  ( -21.97012646571106842, -0.5360883523215664859, -1.500000000000002220 ) ) ;
#29989 = CARTESIAN_POINT ( 'NONE',  ( -87.54805663165109308, -24.34968618360934656, 0.1864209137778970737 ) ) ;
#29990 = VERTEX_POINT ( 'NONE', #76563 ) ;
#29991 = CARTESIAN_POINT ( 'NONE',  ( -74.52287095715007581, -24.64965694238408034, 8.947790433994200043 ) ) ;
#29992 = EDGE_CURVE ( 'NONE', #55686, #79917, #30343, .T. ) ;
#29993 = CARTESIAN_POINT ( 'NONE',  ( -116.6228709571500559, -24.64898659630368627, 1.056161002820833028 ) ) ;
#29994 = LINE ( 'NONE', #92392, #91118 ) ;
#29995 = CARTESIAN_POINT ( 'NONE',  ( -20.41826355431054907, -23.96543168844442562, 8.640809912072075605 ) ) ;
#29996 = CARTESIAN_POINT ( 'NONE',  ( 17.78463046036513617, -11.72987588014745342, 11.49999999999998934 ) ) ;
#29997 = CARTESIAN_POINT ( 'NONE',  ( -75.52287095715007581, -29.50250243563736774, 8.947779886222141599 ) ) ;
#29998 = CARTESIAN_POINT ( 'NONE',  ( -52.22287095715005734, -23.47596703998600276, 11.44779298504227683 ) ) ;
#29999 = EDGE_CURVE ( 'NONE', #35212, #12246, #79947, .T. ) ;
#30000 = VECTOR ( 'NONE', #94836, 1000.000000000000114 ) ;
#30001 = CARTESIAN_POINT ( 'NONE',  ( -90.62287095715004170, -24.99132157543084531, 2.256160258750667502 ) ) ;
#30002 = CARTESIAN_POINT ( 'NONE',  ( -33.60141147702453424, -23.96119346886880308, -0.6495511937832006977 ) ) ;
#30003 = CARTESIAN_POINT ( 'NONE',  ( 15.63351008929417318, -16.12541905121107177, -1.500000000000002220 ) ) ;
#30004 = CARTESIAN_POINT ( 'NONE',  ( -110.9395699835130813, -25.31476271379807841, 5.144092056987718209 ) ) ;
#30005 = ORIENTED_EDGE ( 'NONE', *, *, #40993, .T. ) ;
#30006 = CARTESIAN_POINT ( 'NONE',  ( -99.43243614344049774, -25.11009041281529974, 7.230259461350549088 ) ) ;
#30007 = CARTESIAN_POINT ( 'NONE',  ( 8.161054176536994831, -17.82452852192863091, 11.49999999999999645 ) ) ;
#30008 = FACE_OUTER_BOUND ( 'NONE', #83795, .T. ) ;
#30009 = DIRECTION ( 'NONE',  ( 0.000000000000000000, 0.000000000000000000, 1.000000000000000000 ) ) ;
#30010 = ORIENTED_EDGE ( 'NONE', *, *, #67672, .T. ) ;
#30011 = CIRCLE ( 'NONE', #85141, 19.30000000000000071 ) ;
#30012 = CARTESIAN_POINT ( 'NONE',  ( -79.62287095715005592, -29.50250243563736774, 8.947779886222141599 ) ) ;
#30013 = PLANE ( 'NONE',  #18846 ) ;
#30014 = CARTESIAN_POINT ( 'NONE',  ( -90.93251974643131064, -25.31476272485208412, 5.144091107239472827 ) ) ;
#30015 = VECTOR ( 'NONE', #96719, 1000.000000000000000 ) ;
#30016 = DIRECTION ( 'NONE',  ( 0.000000000000000000, 0.000000000000000000, 1.000000000000000000 ) ) ;
#30017 = CARTESIAN_POINT ( 'NONE',  ( -18.32884136524465291, -7.267937366463995907, 11.49999999999998934 ) ) ;
#30018 = ORIENTED_EDGE ( 'NONE', *, *, #50288, .T. ) ;
#30019 = CARTESIAN_POINT ( 'NONE',  ( -110.2103586364410290, -25.19572374053056407, 3.298817077610923132 ) ) ;
#30020 = DIRECTION ( 'NONE',  ( -0.7071067811865474617, 0.000000000000000000, -0.7071067811865476838 ) ) ;
#30021 = COORDINATED_UNIVERSAL_TIME_OFFSET ( 0, 0, .AHEAD. ) ;
#30022 = EDGE_LOOP ( 'NONE', ( #5021, #49349, #45687, #54336 ) ) ;
#30023 = DIRECTION ( 'NONE',  ( 0.000000000000000000, 0.000000000000000000, -1.000000000000000000 ) ) ;
#30024 = CARTESIAN_POINT ( 'NONE',  ( -1.358974358974357921, -6.376774720514420736, 20.75510817307693046 ) ) ;
#30025 = CARTESIAN_POINT ( 'NONE',  ( -55.63150118323845561, -24.73486907724917572, 1.287355809206962798 ) ) ;
#30026 = CARTESIAN_POINT ( 'NONE',  ( -99.48801098274306298, -25.03145115913622121, 7.273530651135964753 ) ) ;
#30027 = LINE ( 'NONE', #38644, #22541 ) ;
#30028 = CARTESIAN_POINT ( 'NONE',  ( -70.74026866089610621, -25.31511106678998502, 4.894904372220056921 ) ) ;
#30029 = CARTESIAN_POINT ( 'NONE',  ( -107.6339924380179980, -23.48783264082479505, -1.443836473390060826 ) ) ;
#30030 = CARTESIAN_POINT ( 'NONE',  ( -19.61284664649099696, 3.773188449817356904, -1.500000000000002220 ) ) ;
#30031 = CARTESIAN_POINT ( 'NONE',  ( -125.6228709571500559, -24.63345952396256422, 9.038047939301492306 ) ) ;
#30032 = CARTESIAN_POINT ( 'NONE',  ( -45.55045081875104529, -24.15602025860896163, 10.28564288303535434 ) ) ;
#30033 = ORIENTED_EDGE ( 'NONE', *, *, #10061, .T. ) ;
#30034 = LINE ( 'NONE', #83331, #14563 ) ;
#30035 = VECTOR ( 'NONE', #17825, 1000.000000000000000 ) ;
#30036 = LINE ( 'NONE', #61012, #58881 ) ;
#30037 = LINE ( 'NONE', #39158, #38049 ) ;
#30038 = CARTESIAN_POINT ( 'NONE',  ( -81.54383403257651253, -24.51314013834316796, 0.6176544820404249458 ) ) ;
#30039 = B_SPLINE_CURVE_WITH_KNOTS ( 'NONE', 3,
 ( #90221, #51665, #82602, #44045 ),
 .UNSPECIFIED., .F., .F.,
 ( 4, 4 ),
 ( 0.000000000000000000, 0.002769230769239627420 ),
 .UNSPECIFIED. ) ;
#30040 = CARTESIAN_POINT ( 'NONE',  ( -27.70544111104076990, -24.60093890412679229, 1.628749891592534693 ) ) ;
#30041 = CARTESIAN_POINT ( 'NONE',  ( -1.743696941008423984, -5.876774720514413630, 19.59984006504825160 ) ) ;
#30042 = B_SPLINE_CURVE_WITH_KNOTS ( 'NONE', 3,
 ( #69259, #16456, #68764, #47928 ),
 .UNSPECIFIED., .F., .F.,
 ( 4, 4 ),
 ( 0.1506075451614858618, 0.1596139764336012845 ),
 .UNSPECIFIED. ) ;
#30043 = CARTESIAN_POINT ( 'NONE',  ( -79.62287095715005592, -23.48786465467241058, 11.44779295918254469 ) ) ;
#30044 = CARTESIAN_POINT ( 'NONE',  ( 5.331146515430939203, -6.376774720514420736, 20.91308853528358469 ) ) ;
#30045 = VERTEX_POINT ( 'NONE', #17179 ) ;
#30046 = ADVANCED_FACE ( 'NONE', ( #41034 ), #23789, .T. ) ;
#30047 = CARTESIAN_POINT ( 'NONE',  ( -9.609455416251792670, -17.83980533922896683, -1.500000000000002220 ) ) ;
#30048 = CARTESIAN_POINT ( 'NONE',  ( -76.62287095715007013, -23.48786465467241058, 11.44779295918254469 ) ) ;
#30049 = CARTESIAN_POINT ( 'NONE',  ( 21.89332223281681067, 4.278632354317016606, -16.39935597170616788 ) ) ;
#30050 = EDGE_CURVE ( 'NONE', #12135, #5267, #2469, .T. ) ;
#30051 = CARTESIAN_POINT ( 'NONE',  ( -90.52287095715007581, -24.82558206586149652, 1.605769216559628010 ) ) ;
#30052 = EDGE_CURVE ( 'NONE', #24726, #81664, #38781, .T. ) ;
#30053 = ORIENTED_EDGE ( 'NONE', *, *, #90033, .F. ) ;
#30054 = CARTESIAN_POINT ( 'NONE',  ( 16.00000000000000000, 0.000000000000000000, 21.89999999999999858 ) ) ;
#30055 = B_SPLINE_CURVE_WITH_KNOTS ( 'NONE', 3,
 ( #88462, #10331, #63640, #10835 ),
 .UNSPECIFIED., .F., .F.,
 ( 4, 4 ),
 ( 1.422342543128534982E-05, 0.002384588281187964391 ),
 .UNSPECIFIED. ) ;
#30056 = CARTESIAN_POINT ( 'NONE',  ( -1.488488975859286523, -5.876774720514410966, 19.49847411603315095 ) ) ;
#30057 = CARTESIAN_POINT ( 'NONE',  ( 19.44710440357065551, 5.058846670610233076, -1.500000000000002220 ) ) ;
#30058 = EDGE_CURVE ( 'NONE', #31628, #43602, #78776, .T. ) ;
#30059 = CARTESIAN_POINT ( 'NONE',  ( 15.50021099394596646, 14.30638080151107694, 11.49999999999999645 ) ) ;
#30060 = CARTESIAN_POINT ( 'NONE',  ( -22.05275734969026047, 0.3587747205144262708, 30.51402280011862089 ) ) ;
#30061 = CARTESIAN_POINT ( 'NONE',  ( 19.10104996495751450, -11.12853483292915691, -1.500000000000002220 ) ) ;
#30062 = EDGE_CURVE ( 'NONE', #26538, #85004, #2317, .T. ) ;
#30063 = CARTESIAN_POINT ( 'NONE',  ( 12.93548710985481698, 15.95582723538240266, -1.500000000000002220 ) ) ;
#30064 = CARTESIAN_POINT ( 'NONE',  ( -47.52287095715006160, -23.47596703998600631, 11.44779298504229104 ) ) ;
#30065 = VECTOR ( 'NONE', #13341, 1000.000000000000227 ) ;
#30066 = CARTESIAN_POINT ( 'NONE',  ( -60.55145188000605572, -24.15503026093916006, -0.2815557561904390993 ) ) ;
#30067 = ORIENTED_EDGE ( 'NONE', *, *, #12659, .T. ) ;
#30068 = DIRECTION ( 'NONE',  ( 0.000000000000000000, -2.173523156925980399E-06, 0.9999999999976378895 ) ) ;
#30069 = VERTEX_POINT ( 'NONE', #70477 ) ;
#30070 = CARTESIAN_POINT ( 'NONE',  ( -100.3561995057198288, -25.12094576395124790, 2.834877649516965636 ) ) ;
#30071 = CARTESIAN_POINT ( 'NONE',  ( -87.62287095715004170, -24.66019654487199020, 8.947790411086129936 ) ) ;
#30072 = ORIENTED_EDGE ( 'NONE', *, *, #57570, .T. ) ;
#30073 = VERTEX_POINT ( 'NONE', #24298 ) ;
#30074 = AXIS2_PLACEMENT_3D ( 'NONE', #8289, #39235, #60603 ) ;
#30075 = ORIENTED_EDGE ( 'NONE', *, *, #45836, .F. ) ;
#30076 = CARTESIAN_POINT ( 'NONE',  ( -80.72727431975152967, -25.25269385731764160, 3.802325930818207134 ) ) ;
#30077 = LINE ( 'NONE', #99082, #81048 ) ;
#30079 = ADVANCED_FACE ( 'NONE', ( #961 ), #65340, .T. ) ;
#30078 = FACE_OUTER_BOUND ( 'NONE', #83765, .T. ) ;
#30080 = CARTESIAN_POINT ( 'NONE',  ( 15.34805171112899203, -13.82090413600154299, -1.500000000000002220 ) ) ;
#30081 = CIRCLE ( 'NONE', #20376, 6.099999999999999645 ) ;
#30082 = CARTESIAN_POINT ( 'NONE',  ( -12.93760099376155104, 17.33828479246177423, 11.49999999999999645 ) ) ;
#30083 = ORIENTED_EDGE ( 'NONE', *, *, #23881, .T. ) ;
#30084 = DIRECTION ( 'NONE',  ( -3.773278334453079618E-23, 0.9999999999976377785, 2.173523156925979975E-06 ) ) ;
#30085 = CARTESIAN_POINT ( 'NONE',  ( -96.62287095715005592, -24.64965695001468404, 8.947790433994178727 ) ) ;
#30086 = CARTESIAN_POINT ( 'NONE',  ( -20.28323820415832657, -9.445149539555593776, 11.49999999999998934 ) ) ;
#30087 = AXIS2_PLACEMENT_3D ( 'NONE', #26569, #19439, #73242 ) ;
#30088 = CARTESIAN_POINT ( 'NONE',  ( -62.52287095715006160, -23.73907113216987952, -1.053371485793251461 ) ) ;
#30089 = CARTESIAN_POINT ( 'NONE',  ( -82.52287095715006160, -23.47593901973090169, -1.443836447538996648 ) ) ;
#30090 = ORIENTED_EDGE ( 'NONE', *, *, #92299, .T. ) ;
#30091 = CARTESIAN_POINT ( 'NONE',  ( 32.87794144969610244, -3.622774687813811845, -13.08434676285136256 ) ) ;
#30092 = CARTESIAN_POINT ( 'NONE',  ( 27.53860345374808105, -5.356774720514425603, -6.982392034745776854 ) ) ;
#30093 = CARTESIAN_POINT ( 'NONE',  ( -12.66259425867894350, -16.64798919286708667, -1.500000000000002220 ) ) ;
#30094 = ORIENTED_EDGE ( 'NONE', *, *, #27326, .T. ) ;
#30096 = EDGE_LOOP ( 'NONE', ( #98184, #57163, #33085, #59770 ) ) ;
#30095 = CARTESIAN_POINT ( 'NONE',  ( -67.51046660421201295, -23.96169478059713853, 10.65365249895717881 ) ) ;
#30097 = EDGE_LOOP ( 'NONE', ( #63445, #86635, #25019, #82163 ) ) ;
#30098 = CARTESIAN_POINT ( 'NONE',  ( -109.6310424504063974, -23.73791477778912551, 11.05961554403169878 ) ) ;
#30099 = CARTESIAN_POINT ( 'NONE',  ( 16.79009078985406234, 12.93418496121567252, -1.500000000000002220 ) ) ;
#30100 = EDGE_LOOP ( 'NONE', ( #91952, #99901, #17869, #22880 ) ) ;
#30101 = DIRECTION ( 'NONE',  ( 0.000000000000000000, 0.000000000000000000, 1.000000000000000000 ) ) ;
#30102 = CARTESIAN_POINT ( 'NONE',  ( -99.97649549088345111, -25.12215660189515631, 7.032284957836063555 ) ) ;
#30103 = CARTESIAN_POINT ( 'NONE',  ( 13.71991279636371175, 16.93377936151356877, 11.49999999999998934 ) ) ;
#30104 = CARTESIAN_POINT ( 'NONE',  ( -7.627782137226129855, -6.376774720514413630, 20.04377961306771994 ) ) ;
#30105 = CARTESIAN_POINT ( 'NONE',  ( -35.58953762381672448, -24.99156044556202616, 7.747789690856173195 ) ) ;
#30106 = LINE ( 'NONE', #83899, #22205 ) ;
#30107 = CARTESIAN_POINT ( 'NONE',  ( 21.40858030128615397, -3.853468400179685727, -1.500000000000002220 ) ) ;
#30108 = CARTESIAN_POINT ( 'NONE',  ( -0.7614568544629641833, -6.376774720514408301, 19.18727597066020962 ) ) ;
#30110 = EDGE_LOOP ( 'NONE', ( #8918, #96239, #42220 ) ) ;
#30109 = CARTESIAN_POINT ( 'NONE',  ( -18.48265707593502327, -12.51853143457666562, 11.49999999999999645 ) ) ;
#30111 = CARTESIAN_POINT ( 'NONE',  ( 7.160000000000000142, 8.793627758918228565, -2.994553991265763049 ) ) ;
#30112 = CARTESIAN_POINT ( 'NONE',  ( 23.50000000000000000, -0.9000000000000000222, -1.103411337323757957 ) ) ;
#30113 = ADVANCED_FACE ( 'NONE', ( #6404 ), #53593, .T. ) ;
#30114 = CARTESIAN_POINT ( 'NONE',  ( -43.62287095715006302, -24.33832256526967797, 0.1851278514119845120 ) ) ;
#30115 = EDGE_LOOP ( 'NONE', ( #33573, #35870, #97987, #95439 ) ) ;
#30116 = ORIENTED_EDGE ( 'NONE', *, *, #59512, .T. ) ;
#30117 = ORIENTED_EDGE ( 'NONE', *, *, #13464, .T. ) ;
#30118 = CARTESIAN_POINT ( 'NONE',  ( 1.408343819019456028E-16, -6.943225279485572443, 1.149999999999999911 ) ) ;
#30119 = CARTESIAN_POINT ( 'NONE',  ( 21.18767802922067034, -0.7184367399587067160, -1.500000000000002220 ) ) ;
#30120 = CARTESIAN_POINT ( 'NONE',  ( -27.25988310792305214, -5.965225279485572685, 30.32664379231667695 ) ) ;
#30121 = CARTESIAN_POINT ( 'NONE',  ( -80.29067095681661215, -25.03138296994456979, 7.551389794076908579 ) ) ;
#30122 = CARTESIAN_POINT ( 'NONE',  ( 21.29879217689888904, -4.383176333286276538, -16.78405200760721527 ) ) ;
#30123 = LINE ( 'NONE', #97277, #88105 ) ;
#30124 = CARTESIAN_POINT ( 'NONE',  ( -19.24332624019526961, -2.196797614219411443, -1.500000000000002220 ) ) ;
#30125 = ADVANCED_FACE ( 'NONE', ( #69800 ), #100215, .F. ) ;
#30126 = CARTESIAN_POINT ( 'NONE',  ( -45.52197100924568218, -23.48783264082476308, -1.443836473390102793 ) ) ;
#30127 = VERTEX_POINT ( 'NONE', #61700 ) ;
#30128 = CARTESIAN_POINT ( 'NONE',  ( 1.664315604108443925, 19.36118569274438528, 11.49999999999999645 ) ) ;
#30129 = CARTESIAN_POINT ( 'NONE',  ( -107.9228709571500815, -23.47596703998600631, 11.44779298504227860 ) ) ;
#30130 = B_SPLINE_CURVE_WITH_KNOTS ( 'NONE', 3,
 ( #69625, #68127, #99049, #22908 ),
 .UNSPECIFIED., .F., .F.,
 ( 4, 4 ),
 ( 0.000000000000000000, 9.999999999998897304E-05 ),
 .UNSPECIFIED. ) ;
#30131 = EDGE_CURVE ( 'NONE', #94426, #14476, #279, .T. ) ;
#30132 = ORIENTED_EDGE ( 'NONE', *, *, #20604, .T. ) ;
#30133 = CARTESIAN_POINT ( 'NONE',  ( 3.252808283508203058, -5.876774720514403860, 18.30939203766361345 ) ) ;
#30134 = CARTESIAN_POINT ( 'NONE',  ( 0.000000000000000000, -16.94322527948557422, 3.500000000000000000 ) ) ;
#30135 = VECTOR ( 'NONE', #67751, 1000.000000000000114 ) ;
#30136 = CARTESIAN_POINT ( 'NONE',  ( -97.25593102651548350, -24.04668586515358442, 10.47594215909545312 ) ) ;
#30137 = CARTESIAN_POINT ( 'NONE',  ( 18.70796670040472165, 5.986831462552164140, -1.500000000000002220 ) ) ;
#30138 = CARTESIAN_POINT ( 'NONE',  ( -41.23075053442405391, -25.27806068830949116, 4.755616919394483055 ) ) ;
#30139 = ORIENTED_EDGE ( 'NONE', *, *, #50080, .T. ) ;
#30140 = CARTESIAN_POINT ( 'NONE',  ( 20.54099941694853726, 6.510794959084822864, -1.500000000000002220 ) ) ;
#30141 = CARTESIAN_POINT ( 'NONE',  ( 9.950000000000006395, 0.000000000000000000, 19.30000000000000071 ) ) ;
#30142 = CARTESIAN_POINT ( 'NONE',  ( -8.499999999999987566, 18.74999999999999645, 2.100000000000000089 ) ) ;
#30143 = CARTESIAN_POINT ( 'NONE',  ( -99.56269727232219680, -25.27473330506526139, 3.795001076773547144 ) ) ;
#30144 = CARTESIAN_POINT ( 'NONE',  ( -21.01138170180016118, -9.542296329091309204, -1.500000000000002220 ) ) ;
#30145 = CC_DESIGN_PERSON_AND_ORGANIZATION_ASSIGNMENT ( #41926, #73857, ( #3711 ) ) ;
#30146 = VECTOR ( 'NONE', #54046, 1000.000000000000000 ) ;
#30147 = COORDINATED_UNIVERSAL_TIME_OFFSET ( 0, 0, .AHEAD. ) ;
#30148 = CARTESIAN_POINT ( 'NONE',  ( -53.01255352321339842, -2.682774720514426559, 35.59556822165056644 ) ) ;
#30149 = CARTESIAN_POINT ( 'NONE',  ( -89.22287095715005023, -23.47596703998600631, 11.44779298504227860 ) ) ;
#30150 = CARTESIAN_POINT ( 'NONE',  ( 7.037473118728134303, -18.94123407977296480, 11.49999999999999645 ) ) ;
#30151 = CARTESIAN_POINT ( 'NONE',  ( -121.5198912994663232, -24.15620529776628800, 10.23563542870660115 ) ) ;
#30152 = LINE ( 'NONE', #83439, #30599 ) ;
#30153 = VECTOR ( 'NONE', #55971, 1000.000000000000114 ) ;
#30155 = CARTESIAN_POINT ( 'NONE',  ( -111.7788625685672486, -25.29824125544099900, 4.278827553184073373 ) ) ;
#30154 = CIRCLE ( 'NONE', #36606, 12.23252173913042995 ) ;
#30156 = DIRECTION ( 'NONE',  ( -1.000000000000000000, -3.773278334444166432E-23, -8.201307841325785021E-29 ) ) ;
#30157 = CARTESIAN_POINT ( 'NONE',  ( -110.8177083405623478, -25.18425605443559689, 3.398758359099868009 ) ) ;
#30158 = CARTESIAN_POINT ( 'NONE',  ( 19.88832268942539017, -0.5522253751840191516, -1.500000000000002220 ) ) ;
#30159 = VECTOR ( 'NONE', #98015, 1000.000000000000000 ) ;
#30160 = CARTESIAN_POINT ( 'NONE',  ( -79.11611000704996854, -25.19045605819419720, 3.255062319851647956 ) ) ;
#30161 = CARTESIAN_POINT ( 'NONE',  ( 3.553741186906278493, -19.43417129498564577, -1.500000000000002220 ) ) ;
#30162 = AXIS2_PLACEMENT_3D ( 'NONE', #92199, #85587, #16072 ) ;
#30163 = LINE ( 'NONE', #47400, #60503 ) ;
#30164 = CARTESIAN_POINT ( 'NONE',  ( -123.5228709571500616, -23.47596703998600631, 11.44779298504227860 ) ) ;
#30165 = CARTESIAN_POINT ( 'NONE',  ( -42.52287095715005449, -24.64898659630367206, 1.056161002820819261 ) ) ;
#30166 = CARTESIAN_POINT ( 'NONE',  ( -19.97286373971314433, -5.326668811655218327, 11.49999999999999645 ) ) ;
#30167 = CARTESIAN_POINT ( 'NONE',  ( -128.5228709571500758, -24.64965694238575722, 8.947790433994189385 ) ) ;
#30168 = CARTESIAN_POINT ( 'NONE',  ( -49.95596087352405590, -25.25138688028978962, 5.268391457946761669 ) ) ;
#30169 = CARTESIAN_POINT ( 'NONE',  ( -10.65177407370799045, -20.06881281718593613, 11.49999999999999645 ) ) ;
#30170 = ORIENTED_EDGE ( 'NONE', *, *, #43649, .F. ) ;
#30171 = CARTESIAN_POINT ( 'NONE',  ( -39.52287095715006870, -29.50250243563736774, 8.947779886222148704 ) ) ;
#30172 = CARTESIAN_POINT ( 'NONE',  ( -69.34919748320460542, -25.23279835387202397, 6.332189406089158368 ) ) ;
#30173 = CARTESIAN_POINT ( 'NONE',  ( -19.70923665959843873, 4.302044407003456250, 11.49999999999998934 ) ) ;
#30174 = CARTESIAN_POINT ( 'NONE',  ( -63.50973006361228101, -23.96119346886879597, -0.6495511937832106897 ) ) ;
#30175 = CARTESIAN_POINT ( 'NONE',  ( -100.4326965455115044, -29.50249014687182836, 3.293933732389337621 ) ) ;
#30176 = CIRCLE ( 'NONE', #66084, 6.119803529381342422 ) ;
#30177 = ORIENTED_EDGE ( 'NONE', *, *, #26180, .F. ) ;
#30178 = ORIENTED_EDGE ( 'NONE', *, *, #6637, .T. ) ;
#30179 = CARTESIAN_POINT ( 'NONE',  ( -24.97666371003640151, -5.965225279485592225, -15.72894043976419098 ) ) ;
#30180 = CARTESIAN_POINT ( 'NONE',  ( -4.124250913864588419, 22.51598698906299845, 11.49999999999998934 ) ) ;
#30181 = CARTESIAN_POINT ( 'NONE',  ( -50.90914965406638260, -25.18439674812242401, 3.408962482538700378 ) ) ;
#30182 = CARTESIAN_POINT ( 'NONE',  ( -21.34238180412542718, 3.497892552127677135, -1.500000000000002220 ) ) ;
#30183 = CARTESIAN_POINT ( 'NONE',  ( -123.6253769750481837, -23.96119346886881019, -0.6495511937832022520 ) ) ;
#30184 = CARTESIAN_POINT ( 'NONE',  ( -34.66745945777220328, -23.48783264082478084, -1.443836473390076591 ) ) ;
#30185 = EDGE_CURVE ( 'NONE', #67539, #41980, #45478, .T. ) ;
#30186 = CARTESIAN_POINT ( 'NONE',  ( -18.75169668496848985, 9.291489096422434812, 11.49999999999999645 ) ) ;
#30187 = ORIENTED_EDGE ( 'NONE', *, *, #10590, .T. ) ;
#30188 = CARTESIAN_POINT ( 'NONE',  ( -68.96115101070704156, -25.24754476957743066, 5.914983662711241763 ) ) ;
#30189 = CARTESIAN_POINT ( 'NONE',  ( -2.902263480631018577, 21.84654903556016947, -1.500000000000002220 ) ) ;
#30190 = EDGE_CURVE ( 'NONE', #42367, #96258, #39859, .T. ) ;
#30191 = CARTESIAN_POINT ( 'NONE',  ( -61.62287095715004881, -29.50250243563736774, 8.947779886222145151 ) ) ;
#30192 = CARTESIAN_POINT ( 'NONE',  ( -28.29841854899664710, -24.79700284414744615, 7.453535061713724374 ) ) ;
#30193 = ORIENTED_EDGE ( 'NONE', *, *, #48715, .T. ) ;
#30194 = CARTESIAN_POINT ( 'NONE',  ( 4.966983519792414370, -6.376774720514415407, 19.83633487160803099 ) ) ;
#30195 = CARTESIAN_POINT ( 'NONE',  ( -90.54023306201428056, -25.00182538069146787, 7.747789668545043362 ) ) ;
#30196 = ORIENTED_EDGE ( 'NONE', *, *, #98220, .F. ) ;
#30197 = CARTESIAN_POINT ( 'NONE',  ( 13.91401389203221406, 3.316774720514426456, 27.24920385068457662 ) ) ;
#30198 = ORIENTED_EDGE ( 'NONE', *, *, #55648, .T. ) ;
#30199 = ORIENTED_EDGE ( 'NONE', *, *, #15843, .T. ) ;
#30200 = CARTESIAN_POINT ( 'NONE',  ( -71.60197075763308305, -23.73791477778911840, 11.05961554403170766 ) ) ;
#30201 = DIRECTION ( 'NONE',  ( -3.773278334453079030E-23, 0.9999999999976377785, 2.173523156925979128E-06 ) ) ;
#30203 = EDGE_CURVE ( 'NONE', #61556, #42618, #48026, .T. ) ;
#30202 = CARTESIAN_POINT ( 'NONE',  ( -81.62287095715005592, -24.64898659630528854, 1.056161002820826145 ) ) ;
#30204 = CARTESIAN_POINT ( 'NONE',  ( 20.49162120248849561, -0.4999214236376636200, -1.500000000000002220 ) ) ;
#30205 = VERTEX_POINT ( 'NONE', #37362 ) ;
#30206 = CARTESIAN_POINT ( 'NONE',  ( -2.606012662418322634, -6.376774720514410077, 19.21974929698718881 ) ) ;
#30207 = CARTESIAN_POINT ( 'NONE',  ( -30.61275986115374081, -24.37728322581795481, 9.960208392924579712 ) ) ;
#30208 = CARTESIAN_POINT ( 'NONE',  ( -56.62287095715005592, -24.64898659630528499, 1.056161002820822592 ) ) ;
#30209 = CARTESIAN_POINT ( 'NONE',  ( -4.481184387785930312, -21.81124396384582909, -1.500000000000002220 ) ) ;
#30210 = CIRCLE ( 'NONE', #88603, 3.060000000000000053 ) ;
#30211 = CARTESIAN_POINT ( 'NONE',  ( -4.194375271223358403, -6.376774720514417183, 20.09898898868106087 ) ) ;
#30212 = CARTESIAN_POINT ( 'NONE',  ( -88.62287095715005592, -24.35013146730204170, 9.818937971375104823 ) ) ;
#30213 = ORIENTED_EDGE ( 'NONE', *, *, #98736, .T. ) ;
#30214 = CARTESIAN_POINT ( 'NONE',  ( -85.52287095715006160, -29.50248528299804818, 1.056150453629040253 ) ) ;
#30215 = CARTESIAN_POINT ( 'NONE',  ( 33.96422015159436114, 0.3587747205144265483, -7.233236000911337449 ) ) ;
#30216 = CARTESIAN_POINT ( 'NONE',  ( 9.628234360240019996, 18.42577530400075858, -1.500000000000002220 ) ) ;
#30217 = ORIENTED_EDGE ( 'NONE', *, *, #25121, .F. ) ;
#30219 = ORIENTED_EDGE ( 'NONE', *, *, #76107, .T. ) ;
#30218 = CARTESIAN_POINT ( 'NONE',  ( 32.16024265030974050, 0.3587747205144265483, 14.03360796525321774 ) ) ;
#30220 = VECTOR ( 'NONE', #58898, 1000.000000000000114 ) ;
#30221 = CARTESIAN_POINT ( 'NONE',  ( -118.9228709571500673, -23.47596703998600631, 11.44779298504227683 ) ) ;
#30222 = ORIENTED_EDGE ( 'NONE', *, *, #39212, .F. ) ;
#30223 = ORIENTED_EDGE ( 'NONE', *, *, #70633, .F. ) ;
#30224 = CIRCLE ( 'NONE', #91787, 11.85241003308275864 ) ;
#30225 = CARTESIAN_POINT ( 'NONE',  ( -53.62287095715005592, -29.50250243563736774, 8.947779886222146928 ) ) ;
#30226 = DIRECTION ( 'NONE',  ( -0.09824042138329623641, -0.9951627101165078093, -3.504396110891626425E-15 ) ) ;
#30227 = CARTESIAN_POINT ( 'NONE',  ( -59.62287095715006302, -23.48786465467241058, 11.44779295918254824 ) ) ;
#30228 = VECTOR ( 'NONE', #79761, 1000.000000000000114 ) ;
#30229 = DIRECTION ( 'NONE',  ( -0.000000000000000000, 1.000000000000000000, -0.000000000000000000 ) ) ;
#30230 = CARTESIAN_POINT ( 'NONE',  ( -110.5228709571500758, -23.84047902841603772, -0.8780736468305414544 ) ) ;
#30231 = DIRECTION ( 'NONE',  ( 3.773278334444166432E-23, -1.000000000000000000, 0.000000000000000000 ) ) ;
#30233 = ORIENTED_EDGE ( 'NONE', *, *, #88271, .T. ) ;
#30232 = CARTESIAN_POINT ( 'NONE',  ( -0.8124730928778809425, -22.15030348749839817, 11.49999999999999645 ) ) ;
#30234 = FACE_OUTER_BOUND ( 'NONE', #13015, .T. ) ;
#30235 = CARTESIAN_POINT ( 'NONE',  ( 18.27610663105864219, 13.37729726205769154, 11.49999999999998934 ) ) ;
#30236 = CIRCLE ( 'NONE', #35106, 2.899999999999999911 ) ;
#30238 = VERTEX_POINT ( 'NONE', #31735 ) ;
#30237 = CARTESIAN_POINT ( 'NONE',  ( -124.5895376238167245, -23.47593901973091235, -1.443836447538997536 ) ) ;
#30239 = EDGE_CURVE ( 'NONE', #90630, #86027, #93618, .T. ) ;
#30240 = ORIENTED_EDGE ( 'NONE', *, *, #6420, .F. ) ;
#30241 = CARTESIAN_POINT ( 'NONE',  ( -110.5228709571500616, -23.47596703998600631, 11.44779298504228038 ) ) ;
#30242 = EDGE_CURVE ( 'NONE', #88518, #28525, #7386, .T. ) ;
#30243 = CARTESIAN_POINT ( 'NONE',  ( 9.271505649751263789, 17.87650053469100087, 11.49999999999998934 ) ) ;
#30244 = CARTESIAN_POINT ( 'NONE',  ( -99.52287095715006160, -23.47596703998600631, 11.44779298504228215 ) ) ;
#30245 = EDGE_LOOP ( 'NONE', ( #38052, #16095, #68930, #36856 ) ) ;
#30246 = CYLINDRICAL_SURFACE ( 'NONE', #51948, 18.50000000000000000 ) ;
#30247 = CARTESIAN_POINT ( 'NONE',  ( 9.556255610625576935, 20.19728179944524271, -1.500000000000002220 ) ) ;
#30248 = ORIENTED_EDGE ( 'NONE', *, *, #3732, .T. ) ;
#30249 = EDGE_LOOP ( 'NONE', ( #37416, #85241, #28110, #29215 ) ) ;
#30250 = CARTESIAN_POINT ( 'NONE',  ( -44.52287095715006160, -29.50250243563736774, 8.947779886222148704 ) ) ;
#30251 = PLANE ( 'NONE',  #86417 ) ;
#30252 = CARTESIAN_POINT ( 'NONE',  ( -80.35919894935767616, -25.29542306156489673, 4.505481338088394239 ) ) ;
#30253 = VECTOR ( 'NONE', #79884, 1000.000000000000114 ) ;
#30254 = DIRECTION ( 'NONE',  ( 0.000000000000000000, -0.9999999999976377785, -2.173523156925979128E-06 ) ) ;
#30255 = DIRECTION ( 'NONE',  ( -3.773278334453079030E-23, 0.9999999999976377785, 2.173523156925979128E-06 ) ) ;
#30256 = B_SPLINE_CURVE_WITH_KNOTS ( 'NONE', 3,
 ( #99151, #59620, #98151, #4334 ),
 .UNSPECIFIED., .F., .F.,
 ( 4, 4 ),
 ( 0.000000000000000000, 9.999999999997510880E-05 ),
 .UNSPECIFIED. ) ;
#30257 = CARTESIAN_POINT ( 'NONE',  ( 18.72186718581493636, -5.619560887262019300, 11.49999999999998934 ) ) ;
#30258 = CARTESIAN_POINT ( 'NONE',  ( -50.38191529551148307, -25.11033443737753146, 2.832404817301930056 ) ) ;
#30259 = CARTESIAN_POINT ( 'NONE',  ( 2.695732861974529104, -21.29187259674557708, -1.500000000000002220 ) ) ;
#30260 = AXIS2_PLACEMENT_3D ( 'NONE', #176, #62584, #100105 ) ;
#30261 = CARTESIAN_POINT ( 'NONE',  ( -2.283364382221138467, -6.376774720514411854, 19.46427715384223944 ) ) ;
#30262 = CARTESIAN_POINT ( 'NONE',  ( 30.53060340732036693, 4.132774720514426292, -5.153186819891554471 ) ) ;
#30263 = CARTESIAN_POINT ( 'NONE',  ( -129.5228709571500758, -24.35013146730204525, 9.818937971375099494 ) ) ;
#30264 = CARTESIAN_POINT ( 'NONE',  ( 22.79674358141071977, 1.614764915196592598, -1.500000000000002220 ) ) ;
#30265 = EDGE_CURVE ( 'NONE', #37127, #34684, #27824, .T. ) ;
#30266 = EDGE_CURVE ( 'NONE', #52789, #40572, #43177, .T. ) ;
#30267 = DATE_AND_TIME ( #7933, #21355 ) ;
#30268 = CARTESIAN_POINT ( 'NONE',  ( -96.56113353449998726, -23.48786465467241413, 11.44779295918254469 ) ) ;
#30269 = CARTESIAN_POINT ( 'NONE',  ( 9.940598223437577374, -5.876774720514426953, 17.91871304725684766 ) ) ;
#30270 = CARTESIAN_POINT ( 'NONE',  ( 19.27460657395150889, -5.330843762518559181, 11.49999999999999645 ) ) ;
#30271 = LINE ( 'NONE', #99283, #33876 ) ;
#30272 = CARTESIAN_POINT ( 'NONE',  ( 3.879812756903532556, -5.876774720514401196, 18.16163344421570969 ) ) ;
#30273 = CARTESIAN_POINT ( 'NONE',  ( -108.6228709571500701, -24.50216790748099882, 0.6166512839513758060 ) ) ;
#30274 = ORIENTED_EDGE ( 'NONE', *, *, #11053, .T. ) ;
#30275 = CARTESIAN_POINT ( 'NONE',  ( -89.55620429048337883, -24.64898659630528854, 1.056161002820830364 ) ) ;
#30276 = DIRECTION ( 'NONE',  ( 1.000000000000000000, 0.000000000000000000, 0.000000000000000000 ) ) ;
#30277 = CARTESIAN_POINT ( 'NONE',  ( -3.653784360050144286, 21.42803128968991544, 11.49999999999998934 ) ) ;
#30278 = EDGE_CURVE ( 'NONE', #16367, #64045, #7890, .T. ) ;
#30279 = CARTESIAN_POINT ( 'NONE',  ( -34.52287095715004739, -24.66019654487199730, 8.947790411086121054 ) ) ;
#30280 = CARTESIAN_POINT ( 'NONE',  ( 19.59400933563812330, 0.1774559437341752532, -1.500000000000002220 ) ) ;
#30281 = AXIS2_PLACEMENT_3D ( 'NONE', #41633, #57368, #72575 ) ;
#30282 = LINE ( 'NONE', #28293, #89611 ) ;
#30283 = DIRECTION ( 'NONE',  ( 0.000000000000000000, -0.9999999999976377785, -2.173523156925979128E-06 ) ) ;
#30284 = COORDINATED_UNIVERSAL_TIME_OFFSET ( 0, 0, .AHEAD. ) ;
#30285 = DIRECTION ( 'NONE',  ( -3.773278334444167608E-23, 1.000000000000000000, 0.000000000000000000 ) ) ;
#30286 = CARTESIAN_POINT ( 'NONE',  ( 3.251543564379332008, -5.876774720514424288, 21.68810402963413964 ) ) ;
#30287 = CARTESIAN_POINT ( 'NONE',  ( -5.951451697817415010, -19.63005813332872762, 11.49999999999999645 ) ) ;
#30288 = LINE ( 'NONE', #60763, #60280 ) ;
#30289 = CIRCLE ( 'NONE', #46608, 6.119803529381341534 ) ;
#30290 = DIRECTION ( 'NONE',  ( 0.000000000000000000, 1.000000000000000000, 0.000000000000000000 ) ) ;
#30291 = VERTEX_POINT ( 'NONE', #93121 ) ;
#30292 = CARTESIAN_POINT ( 'NONE',  ( -62.52287095715006160, -23.47596703998600631, 11.44779298504228926 ) ) ;
#30293 = DIRECTION ( 'NONE',  ( -3.773278334453079030E-23, 0.9999999999976377785, 2.173523156925979128E-06 ) ) ;
#30294 = VECTOR ( 'NONE', #60709, 1000.000000000000000 ) ;
#30295 = CARTESIAN_POINT ( 'NONE',  ( -125.5215403751119538, -23.85049219812686871, 10.88485053497526778 ) ) ;
#30296 = FACE_OUTER_BOUND ( 'NONE', #56846, .T. ) ;
#30297 = CIRCLE ( 'NONE', #14068, 2.350000000000000089 ) ;
#30298 = EDGE_CURVE ( 'NONE', #21630, #88472, #8412, .T. ) ;
#30299 = EDGE_CURVE ( 'NONE', #41257, #37557, #79743, .T. ) ;
#30300 = DIRECTION ( 'NONE',  ( -1.000000000000000000, 0.000000000000000000, 0.000000000000000000 ) ) ;
#30301 = FACE_OUTER_BOUND ( 'NONE', #41948, .T. ) ;
#30302 = CARTESIAN_POINT ( 'NONE',  ( 14.79121776280621425, -17.69394282334246427, 11.49999999999999645 ) ) ;
#30303 = CARTESIAN_POINT ( 'NONE',  ( 22.80427751693360960, 0.003464389817739472934, -1.500000000000002220 ) ) ;
#30304 = CARTESIAN_POINT ( 'NONE',  ( -104.5228709571500758, -23.72747288104470798, -1.053458166803225460 ) ) ;
#30305 = CARTESIAN_POINT ( 'NONE',  ( -75.52287095715004739, -24.91570333825771399, 8.075032458260347212 ) ) ;
#30306 = CARTESIAN_POINT ( 'NONE',  ( -123.5228709571501469, -23.73907113216990439, -1.053371485793244799 ) ) ;
#30307 = CARTESIAN_POINT ( 'NONE',  ( 1.926536275058113867, -22.33200895297504474, 11.49999999999999645 ) ) ;
#30308 = FACE_OUTER_BOUND ( 'NONE', #23290, .T. ) ;
#30309 = CARTESIAN_POINT ( 'NONE',  ( -99.25999413675920380, -25.31582255457039921, 5.189783737494863658 ) ) ;
#30310 = CARTESIAN_POINT ( 'NONE',  ( -21.91604229967229500, -0.6759211909499470705, -1.500000000000002220 ) ) ;
#30311 = EDGE_CURVE ( 'NONE', #58343, #73040, #26941, .T. ) ;
#30312 = CARTESIAN_POINT ( 'NONE',  ( -5.654682302363691626, -5.876774720514410077, 19.41635569784906323 ) ) ;
#30313 = CARTESIAN_POINT ( 'NONE',  ( -85.52287095715004739, -29.50248789122583659, 2.256150453626215580 ) ) ;
#30314 = CARTESIAN_POINT ( 'NONE',  ( -125.6228709571500559, -29.50250243563736774, 8.947779886222132717 ) ) ;
#30315 = EDGE_CURVE ( 'NONE', #47577, #77487, #75928, .T. ) ;
#30316 = CARTESIAN_POINT ( 'NONE',  ( -48.88075183786669697, -25.23570012922559158, 6.306895103940420633 ) ) ;
#30317 = DIRECTION ( 'NONE',  ( -3.773278334453079030E-23, 0.9999999999976377785, 2.173523156925979128E-06 ) ) ;
#30318 = ORIENTED_EDGE ( 'NONE', *, *, #776, .F. ) ;
#30319 = CARTESIAN_POINT ( 'NONE',  ( 6.539103723289373171, -19.38406401830294712, 11.49999999999998934 ) ) ;
#30320 = ORIENTED_EDGE ( 'NONE', *, *, #23641, .F. ) ;
#30321 = B_SPLINE_CURVE_WITH_KNOTS ( 'NONE', 3,
 ( #55039, #31691, #62659, #94083, #9346, #93574 ),
 .UNSPECIFIED., .F., .F.,
 ( 4, 2, 4 ),
 ( 1.570755371633895505E-05, 0.001396183895866086669, 0.002776660238015834278 ),
 .UNSPECIFIED. ) ;
#30322 = VERTEX_POINT ( 'NONE', #98767 ) ;
#30323 = ORIENTED_EDGE ( 'NONE', *, *, #71144, .F. ) ;
#30324 = VERTEX_POINT ( 'NONE', #6433 ) ;
#30325 = CARTESIAN_POINT ( 'NONE',  ( -23.05830607064937965, -0.9945063503333604338, -1.500000000000002220 ) ) ;
#30327 = ADVANCED_FACE ( 'NONE', ( #37387 ), #14532, .F. ) ;
#30326 = CARTESIAN_POINT ( 'NONE',  ( -61.62365984720521794, -24.65952944569304961, 1.056160979905699682 ) ) ;
#30328 = CARTESIAN_POINT ( 'NONE',  ( -19.75413285895528404, 4.560271753130525241, -1.500000000000002220 ) ) ;
#30329 = VERTEX_POINT ( 'NONE', #60237 ) ;
#30330 = CIRCLE ( 'NONE', #56293, 2.999999999999999112 ) ;
#30331 = CARTESIAN_POINT ( 'NONE',  ( -28.20733355685459642, -25.00894895108924842, 3.118813907533751983 ) ) ;
#30332 = CARTESIAN_POINT ( 'NONE',  ( -87.62287095715007013, -23.73934037231757443, 11.05740245334328797 ) ) ;
#30333 = ADVANCED_FACE ( 'NONE', ( #60733, #36881 ), #67346, .F. ) ;
#30334 = DIRECTION ( 'NONE',  ( -3.773278334453079030E-23, 0.9999999999976377785, 2.173523156925979128E-06 ) ) ;
#30335 = CARTESIAN_POINT ( 'NONE',  ( -70.58916620125799568, -24.52300882791528380, 0.6510814631126248253 ) ) ;
#30337 = VERTEX_POINT ( 'NONE', #68336 ) ;
#30336 = CARTESIAN_POINT ( 'NONE',  ( 18.29419249859179786, 11.19154738541161365, 11.49999999999999645 ) ) ;
#30338 = CARTESIAN_POINT ( 'NONE',  ( -113.6228709571500559, -24.50216790748099527, 0.6166512839513743627 ) ) ;
#30339 = CARTESIAN_POINT ( 'NONE',  ( -110.9228709571500673, -23.47593901973090524, -1.443836447538996426 ) ) ;
#30340 = ORIENTED_EDGE ( 'NONE', *, *, #19140, .T. ) ;
#30341 = AXIS2_PLACEMENT_3D ( 'NONE', #20036, #81935, #12417 ) ;
#30342 = CARTESIAN_POINT ( 'NONE',  ( -14.56105648253378781, -14.73650127990469016, 11.49999999999998934 ) ) ;
#30343 = B_SPLINE_CURVE_WITH_KNOTS ( 'NONE', 3,
 ( #7570, #70982, #16179, #10072, #1472, #32917 ),
 .UNSPECIFIED., .F., .F.,
 ( 4, 2, 4 ),
 ( 0.000000000000000000, 0.001380901958385395483, 0.002761803916770790967 ),
 .UNSPECIFIED. ) ;
#30344 = EDGE_LOOP ( 'NONE', ( #286, #89664, #34830, #6417 ) ) ;
#30346 = ORIENTED_EDGE ( 'NONE', *, *, #54713, .T. ) ;
#30345 = DIRECTION ( 'NONE',  ( 1.000000000000000000, 3.639832272653110612E-15, 0.000000000000000000 ) ) ;
#30347 = B_SPLINE_SURFACE_WITH_KNOTS ( 'NONE', 3, 1, ( 
 ( #54516, #23033 ),
 ( #25052, #15935 ),
 ( #46901, #77824 ),
 ( #8333, #39277 ),
 ( #54028, #93556 ),
 ( #27066, #17950 ),
 ( #97070, #4229 ),
 ( #3248, #73245 ),
 ( #72750, #57532 ),
 ( #18942, #27572 ),
 ( #58030, #80853 ),
 ( #80346, #26059 ),
 ( #48913, #34680 ),
 ( #50906, #57031 ),
 ( #79839, #35182 ),
 ( #33679, #89464 ),
 ( #26572, #65653 ),
 ( #64658, #56529 ),
 ( #96565, #10337 ) ),
 .UNSPECIFIED., .F., .F., .F.,
 ( 4, 1, 1, 1, 1, 1, 1, 1, 1, 1, 1, 1, 1, 1, 1, 1, 4 ),
 ( 2, 2 ),
 ( 0.000000000000000000, 0.06761452606740248061, 0.1311670463014500410, 0.1902933887105124899, 0.2450610151831994488, 0.2960272302790624144, 0.3428447301738887232, 0.3860527037713296084, 0.4255709801320516350, 0.4995034801514134370, 0.5702922612469545349, 0.6402757819125004524, 0.7105295546786234429, 0.7812030014762999519, 0.8520349845172642267, 0.9243956695042543359, 1.000000000000000000 ),
 ( 0.000000000000000000, 1.000000000000000000 ),
 .UNSPECIFIED. ) ;
#30348 = CARTESIAN_POINT ( 'NONE',  ( -80.51244414166535535, -29.50249942614373921, 7.563164501610022405 ) ) ;
#30349 = ORIENTED_EDGE ( 'NONE', *, *, #24946, .T. ) ;
#30350 = ORIENTED_EDGE ( 'NONE', *, *, #21644, .F. ) ;
#30351 = CARTESIAN_POINT ( 'NONE',  ( -55.52287095715004739, -24.51254535375842991, 9.355368624242258235 ) ) ;
#30352 = CARTESIAN_POINT ( 'NONE',  ( -65.54557472772603433, -24.40034930558991277, 0.3402023900116039612 ) ) ;
#30353 = CARTESIAN_POINT ( 'NONE',  ( -20.58003014649542095, 7.718188279156099618, 11.49999999999999645 ) ) ;
#30354 = CARTESIAN_POINT ( 'NONE',  ( 30.53060340732035982, -1.477225279485574028, 19.84760796525321780 ) ) ;
#30355 = CARTESIAN_POINT ( 'NONE',  ( 1.525329354412473970, -22.51392980886878448, -1.500000000000002220 ) ) ;
#30356 = AXIS2_PLACEMENT_3D ( 'NONE', #7919, #53616, #38867 ) ;
#30357 = CARTESIAN_POINT ( 'NONE',  ( 5.724939850241691275, 20.19279902153374096, 11.49999999999998934 ) ) ;
#30358 = DIRECTION ( 'NONE',  ( -1.000000000000000000, -0.000000000000000000, -0.000000000000000000 ) ) ;
#30359 = CARTESIAN_POINT ( 'NONE',  ( 5.864225667603142789, -6.376774720514424288, 21.27837265517432996 ) ) ;
#30360 = ORIENTED_EDGE ( 'NONE', *, *, #69460, .F. ) ;
#30361 = ORIENTED_EDGE ( 'NONE', *, *, #68696, .T. ) ;
#30362 = EDGE_LOOP ( 'NONE', ( #28398, #51088 ) ) ;
#30363 = CARTESIAN_POINT ( 'NONE',  ( 5.250998264632097623, -5.356774720514425603, -25.47015671074452925 ) ) ;
#30364 = CIRCLE ( 'NONE', #72537, 28.96799999999999287 ) ;
#30365 = CARTESIAN_POINT ( 'NONE',  ( -2.374466145016132845, -21.38244973876172494, -1.500000000000002220 ) ) ;
#30366 = ADVANCED_FACE ( 'NONE', ( #28772 ), #38373, .T. ) ;
#30367 = ADVANCED_FACE ( 'NONE', ( #7421 ), #67847, .F. ) ;
#30368 = PLANE ( 'NONE',  #68345 ) ;
#30369 = VERTEX_POINT ( 'NONE', #59734 ) ;
#30370 = CARTESIAN_POINT ( 'NONE',  ( 0.3207198112191017025, -21.10926996749724083, -1.500000000000002220 ) ) ;
#30371 = FACE_OUTER_BOUND ( 'NONE', #40554, .T. ) ;
#30372 = CARTESIAN_POINT ( 'NONE',  ( -64.49992615054290468, -24.34968618360933235, 0.1864209137778785330 ) ) ;
#30373 = CARTESIAN_POINT ( 'NONE',  ( -83.62924211730506840, -24.35071581493543036, 9.817618358456028815 ) ) ;
#30374 = CARTESIAN_POINT ( 'NONE',  ( -104.6228709571500559, -24.64898659630529210, 1.056161002820829697 ) ) ;
#30375 = CARTESIAN_POINT ( 'NONE',  ( -69.94583786925741720, -25.25893427375708455, 3.680069841752215964 ) ) ;
#30376 = CARTESIAN_POINT ( 'NONE',  ( 22.09269804725545683, -1.632937629565654580, -1.500000000000002220 ) ) ;
#30377 = CARTESIAN_POINT ( 'NONE',  ( -71.63963700100102017, -23.96119346886880308, -0.6495511937832095795 ) ) ;
#30378 = B_SPLINE_CURVE_WITH_KNOTS ( 'NONE', 3,
 ( #47234, #71078, #23368, #24884 ),
 .UNSPECIFIED., .F., .F.,
 ( 4, 4 ),
 ( 0.000000000000000000, 0.0001000000000000028644 ),
 .UNSPECIFIED. ) ;
#30379 = ORIENTED_EDGE ( 'NONE', *, *, #48812, .F. ) ;
#30380 = CARTESIAN_POINT ( 'NONE',  ( -51.35838135674943317, -25.24860032974256541, 5.126937756223604481 ) ) ;
#30381 = CARTESIAN_POINT ( 'NONE',  ( -67.58953762381672448, -24.64898659630367916, 1.056161002820384054 ) ) ;
#30382 = DIRECTION ( 'NONE',  ( 0.000000000000000000, 0.000000000000000000, -1.000000000000000000 ) ) ;
#30383 = B_SPLINE_CURVE_WITH_KNOTS ( 'NONE', 3,
 ( #62063, #55450, #70667, #8770, #86886, #39205, #87387, #64084 ),
 .UNSPECIFIED., .F., .F.,
 ( 4, 2, 2, 4 ),
 ( -0.001240355328176889803, -0.0002398155169399719417, 0.0007607242942969459198, 0.002761803916770781860 ),
 .UNSPECIFIED. ) ;
#30384 = CARTESIAN_POINT ( 'NONE',  ( -64.62287095715005592, -24.64965695001468404, 8.947790433994185832 ) ) ;
#30385 = CARTESIAN_POINT ( 'NONE',  ( -15.63568348323273227, -11.59263941501104966, -1.500000000000002220 ) ) ;
#30386 = CARTESIAN_POINT ( 'NONE',  ( -1.242826169824672977, 21.35102975155811222, -1.500000000000002220 ) ) ;
#30387 = DIRECTION ( 'NONE',  ( 0.000000000000000000, 0.000000000000000000, -1.000000000000000000 ) ) ;
#30388 = CARTESIAN_POINT ( 'NONE',  ( -42.52287095715005449, -29.50250786944525672, 11.44777988621624232 ) ) ;
#30389 = CARTESIAN_POINT ( 'NONE',  ( -72.52287095715007581, -23.47596703998600631, 11.44779298504228748 ) ) ;
#30390 = LINE ( 'NONE', #20767, #63626 ) ;
#30391 = CARTESIAN_POINT ( 'NONE',  ( -21.51096707683950626, -7.176001652309477841, -1.500000000000002220 ) ) ;
#30392 = EDGE_CURVE ( 'NONE', #94978, #79832, #74926, .T. ) ;
#30393 = DIRECTION ( 'NONE',  ( 0.6392559695863496705, 0.000000000000000000, 0.7689940216596069522 ) ) ;
#30394 = PLANE ( 'NONE',  #47609 ) ;
#30395 = CARTESIAN_POINT ( 'NONE',  ( 14.45944668481935658, 13.51102189132778442, 11.49999999999999645 ) ) ;
#30396 =( BOUNDED_SURFACE ( )  B_SPLINE_SURFACE ( 3, 2, ( 
 ( #100077, #38200, #91991 ),
 ( #30091, #38702, #22462 ),
 ( #53450, #54945, #85885 ),
 ( #69666, #47830, #93481 ),
 ( #143, #30592, #84378 ),
 ( #85374, #24479, #78752 ) ),
 .UNSPECIFIED., .F., .F., .T. ) 
 B_SPLINE_SURFACE_WITH_KNOTS ( ( 4, 2, 4 ),
 ( 3, 3 ),
 ( 0.001113071882895040263, 0.001219813747004279327, 0.001326555611113518392 ),
 ( 0.000000000000000000, 1.000000000000000000 ),
 .UNSPECIFIED. ) 
 GEOMETRIC_REPRESENTATION_ITEM ( )  RATIONAL_B_SPLINE_SURFACE ( (
 ( 1.000000000000000000, 0.7071067811865114905, 1.000000000000000000),
 ( 1.000000000000000000, 0.7264088502634352684, 1.000000000000000000),
 ( 1.000000000000000000, 0.7445305694446069378, 1.000000000000000000),
 ( 1.000000000000000000, 0.7788548593121751296, 1.000000000000000000),
 ( 1.000000000000000000, 0.7952519535464425138, 1.000000000000000000),
 ( 1.000000000000000000, 0.8096947957033885368, 1.000000000000000000) ) ) 
 REPRESENTATION_ITEM ( '' )  SURFACE ( )  );
#30397 = EDGE_CURVE ( 'NONE', #63837, #24351, #21688, .T. ) ;
#30398 = DIRECTION ( 'NONE',  ( 0.000000000000000000, -0.9999999999976377785, -2.173523156925979128E-06 ) ) ;
#30399 = ORIENTED_EDGE ( 'NONE', *, *, #45124, .T. ) ;
#30400 = CARTESIAN_POINT ( 'NONE',  ( -66.58953762381672448, -24.64898659630367916, 1.056161002820382722 ) ) ;
#30402 = EDGE_CURVE ( 'NONE', #98229, #64340, #6927, .T. ) ;
#30401 = CARTESIAN_POINT ( 'NONE',  ( -61.64687923781919920, -25.14083923594766645, 2.947789366383931853 ) ) ;
#30403 = CARTESIAN_POINT ( 'NONE',  ( 21.43499300031224664, 3.042053824063517542, 11.49999999999998934 ) ) ;
#30404 = AXIS2_PLACEMENT_3D ( 'NONE', #98492, #99980, #28994 ) ;
#30405 = EDGE_CURVE ( 'NONE', #63299, #23903, #25301, .T. ) ;
#30406 = LINE ( 'NONE', #69971, #88539 ) ;
#30407 = CARTESIAN_POINT ( 'NONE',  ( 17.65527434030279252, -8.155491144718855168, -1.500000000000002220 ) ) ;
#30408 = ADVANCED_FACE ( 'NONE', ( #53120 ), #86034, .F. ) ;
#30409 = CARTESIAN_POINT ( 'NONE',  ( -82.52287095715011844, -24.51387760970725083, 9.387446482453416507 ) ) ;
#30410 = FACE_OUTER_BOUND ( 'NONE', #20353, .T. ) ;
#30411 = CARTESIAN_POINT ( 'NONE',  ( 16.01007288495529224, -11.65062672332236104, 11.49999999999998934 ) ) ;
#30412 = EDGE_LOOP ( 'NONE', ( #31617, #6805, #78633, #74635 ) ) ;
#30413 = EDGE_CURVE ( 'NONE', #47659, #56669, #99752, .T. ) ;
#30414 = CARTESIAN_POINT ( 'NONE',  ( 3.964343641299885146, 19.94596313931659992, 11.49999999999999645 ) ) ;
#30415 = CARTESIAN_POINT ( 'NONE',  ( -80.64599942773482155, -23.85016227208580020, -0.8807180028928338622 ) ) ;
#30416 = CARTESIAN_POINT ( 'NONE',  ( 33.10022444407529463, -4.633339536272139902, -11.64480304263449106 ) ) ;
#30417 = ORIENTED_EDGE ( 'NONE', *, *, #54162, .T. ) ;
#30418 = CARTESIAN_POINT ( 'NONE',  ( -30.56688274934923299, -25.56688301298833821, 3.825958421598585790 ) ) ;
#30419 = DIRECTION ( 'NONE',  ( -3.773278334444167608E-23, 1.000000000000000000, 0.000000000000000000 ) ) ;
#30420 = CARTESIAN_POINT ( 'NONE',  ( 33.74607884027702909, 0.3587747205144265483, -4.999864028243830916 ) ) ;
#30421 = B_SPLINE_CURVE_WITH_KNOTS ( 'NONE', 3,
 ( #41802, #64148, #87963, #48910, #40783, #26568, #10333, #49415 ),
 .UNSPECIFIED., .F., .F.,
 ( 4, 2, 2, 4 ),
 ( -0.001240666984355828697, -0.0002401179793394868714, 0.0007604310256768549540, 0.002761529035709537738 ),
 .UNSPECIFIED. ) ;
#30422 = CARTESIAN_POINT ( 'NONE',  ( -40.66403789857419326, -23.85049219812685095, 10.88485053497527488 ) ) ;
#30423 = CARTESIAN_POINT ( 'NONE',  ( -127.6228709571500275, -24.33927499327854704, 9.819080762295811837 ) ) ;
#30424 = CARTESIAN_POINT ( 'NONE',  ( -19.29710791919172053, 5.528754708966634901, -1.500000000000002220 ) ) ;
#30425 = EDGE_CURVE ( 'NONE', #71428, #11978, #92155, .T. ) ;
#30426 = EDGE_CURVE ( 'NONE', #89034, #47332, #58031, .T. ) ;
#30427 = LINE ( 'NONE', #52777, #51605 ) ;
#30428 = ORIENTED_EDGE ( 'NONE', *, *, #45047, .F. ) ;
#30429 = DIRECTION ( 'NONE',  ( 0.000000000000000000, 0.000000000000000000, -1.000000000000000000 ) ) ;
#30430 = CIRCLE ( 'NONE', #59639, 1.699999999999999289 ) ;
#30431 = CARTESIAN_POINT ( 'NONE',  ( -21.29394331855728240, -8.360804490491451801, 11.49999999999999645 ) ) ;
#30432 = CARTESIAN_POINT ( 'NONE',  ( -19.63924127562733446, 11.44998032699685631, -1.500000000000002220 ) ) ;
#30433 = CARTESIAN_POINT ( 'NONE',  ( -49.50986403386431078, -25.26258728624853234, 4.014908451308841109 ) ) ;
#30434 = DIRECTION ( 'NONE',  ( -1.000000000000000000, -0.000000000000000000, -0.000000000000000000 ) ) ;
#30435 = CARTESIAN_POINT ( 'NONE',  ( -10.16634758543296613, 5.965225279485572685, 30.00402280011862288 ) ) ;
#30436 = CARTESIAN_POINT ( 'NONE',  ( 6.044119082205957838, -5.876774720514424288, 21.40268112089023589 ) ) ;
#30437 = B_SPLINE_CURVE_WITH_KNOTS ( 'NONE', 3,
 ( #26256, #80039, #88160, #10024, #17639, #9525, #10525, #57228, #18139, #18630 ),
 .UNSPECIFIED., .F., .F.,
 ( 4, 2, 2, 2, 4 ),
 ( 0.000000000000000000, 0.0002557780953295595299, 0.0005115561906591190597, 0.0007673342859886786438, 0.001023112381318238119 ),
 .UNSPECIFIED. ) ;
#30438 = EDGE_CURVE ( 'NONE', #48122, #77832, #52115, .T. ) ;
#30439 = AXIS2_PLACEMENT_3D ( 'NONE', #92976, #77740, #92476 ) ;
#30440 = CARTESIAN_POINT ( 'NONE',  ( -16.22218391600152643, -6.376774720514426953, -54.85883559227303863 ) ) ;
#30441 = EDGE_CURVE ( 'NONE', #67226, #20703, #87712, .T. ) ;
#30442 = LINE ( 'NONE', #46678, #90628 ) ;
#30443 = VERTEX_POINT ( 'NONE', #55619 ) ;
#30444 = VECTOR ( 'NONE', #54555, 999.9999999999998863 ) ;
#30445 = CARTESIAN_POINT ( 'NONE',  ( 17.42226438573850800, -10.51879874471254261, -1.500000000000002220 ) ) ;
#30446 = ORIENTED_EDGE ( 'NONE', *, *, #47245, .F. ) ;
#30447 = CARTESIAN_POINT ( 'NONE',  ( -2.116611060711651504, 22.89395876494169002, -1.500000000000002220 ) ) ;
#30448 = ADVANCED_FACE ( 'NONE', ( #56123 ), #24639, .T. ) ;
#30449 = DIRECTION ( 'NONE',  ( -0.000000000000000000, -1.000000000000000000, -0.000000000000000000 ) ) ;
#30450 = VERTEX_POINT ( 'NONE', #32261 ) ;
#30451 = CARTESIAN_POINT ( 'NONE',  ( -24.97666371003640151, 5.965225279485592225, -15.72894043976419098 ) ) ;
#30452 = EDGE_CURVE ( 'NONE', #28633, #44325, #55112, .T. ) ;
#30453 = CARTESIAN_POINT ( 'NONE',  ( -77.63799604921862851, -23.96169478059713498, 10.65365249895717703 ) ) ;
#30454 = EDGE_CURVE ( 'NONE', #88744, #45969, #35019, .T. ) ;
#30455 = CARTESIAN_POINT ( 'NONE',  ( -51.62368732844929298, -24.66019654487199730, 8.947790411086117501 ) ) ;
#30457 = VERTEX_POINT ( 'NONE', #8427 ) ;
#30456 = CARTESIAN_POINT ( 'NONE',  ( -13.45305159987462851, 16.49040971879131234, 11.49999999999999645 ) ) ;
#30458 = ORIENTED_EDGE ( 'NONE', *, *, #87604, .T. ) ;
#30459 = CARTESIAN_POINT ( 'NONE',  ( -5.848988146064017180, 21.40304369876291446, -1.500000000000002220 ) ) ;
#30460 = CARTESIAN_POINT ( 'NONE',  ( -7.658335995763069448, 19.15843701367676388, -1.500000000000002220 ) ) ;
#30461 = ORIENTED_EDGE ( 'NONE', *, *, #74187, .F. ) ;
#30462 = ORIENTED_EDGE ( 'NONE', *, *, #69834, .F. ) ;
#30463 = CARTESIAN_POINT ( 'NONE',  ( -109.5136315545911856, -25.31627384547671511, 5.394825593643450823 ) ) ;
#30464 = ADVANCED_FACE ( 'NONE', ( #32761 ), #78926, .F. ) ;
#30465 = CARTESIAN_POINT ( 'NONE',  ( -39.05141833839561372, -25.27719696402067129, 4.032623266159655273 ) ) ;
#30466 = ORIENTED_EDGE ( 'NONE', *, *, #53805, .T. ) ;
#30467 = CARTESIAN_POINT ( 'NONE',  ( -49.34124502834663417, -25.22564238971922990, 6.480461498194810765 ) ) ;
#30468 = ORIENTED_EDGE ( 'NONE', *, *, #5463, .T. ) ;
#30469 = LINE ( 'NONE', #84247, #42182 ) ;
#30470 = DIRECTION ( 'NONE',  ( -3.773278334453079618E-23, 0.9999999999976377785, 2.173523156925979975E-06 ) ) ;
#30471 = CARTESIAN_POINT ( 'NONE',  ( 1.081820405348005165, -20.78239343107542680, -1.500000000000002220 ) ) ;
#30472 = CARTESIAN_POINT ( 'NONE',  ( 14.98227958311676744, 15.82868232077399462, 11.49999999999999645 ) ) ;
#30473 = CARTESIAN_POINT ( 'NONE',  ( -90.52380231474228367, -25.22391154813774250, 6.409327647370975711 ) ) ;
#30474 = CARTESIAN_POINT ( 'NONE',  ( -100.2506239054133204, -25.03433485709489759, 7.556303271660354426 ) ) ;
#30475 = CARTESIAN_POINT ( 'NONE',  ( 22.31695869535024102, -2.478243017838637652, 11.49999999999998934 ) ) ;
#30476 = CARTESIAN_POINT ( 'NONE',  ( -51.29424904866267099, -25.31296618838156931, 4.063411898103660214 ) ) ;
#30477 = VERTEX_POINT ( 'NONE', #23638 ) ;
#30478 = DIRECTION ( 'NONE',  ( -0.000000000000000000, 2.173523156925979552E-06, -0.9999999999976378895 ) ) ;
#30479 = CARTESIAN_POINT ( 'NONE',  ( -50.46342637979365264, -25.11078852230776803, 2.834907798866269868 ) ) ;
#30480 = B_SPLINE_SURFACE_WITH_KNOTS ( 'NONE', 3, 1, ( 
 ( #51507, #29153 ),
 ( #51010, #37766 ),
 ( #43398, #68723 ),
 ( #98654, #60126 ),
 ( #30143, #98153 ),
 ( #68225, #52502 ),
 ( #97668, #91547 ),
 ( #99152, #21525 ),
 ( #20533, #83432 ),
 ( #81944, #13920 ),
 ( #29652, #14419 ),
 ( #44897, #59621 ),
 ( #60626, #53009 ),
 ( #22020, #90554 ),
 ( #12430, #82439 ),
 ( #75322, #83939 ),
 ( #91052, #5317 ),
 ( #45394, #28660 ),
 ( #28166, #75819 ) ),
 .UNSPECIFIED., .F., .F., .F.,
 ( 4, 1, 1, 1, 1, 1, 1, 1, 1, 1, 1, 1, 1, 1, 1, 1, 4 ),
 ( 2, 2 ),
 ( 0.000000000000000000, 0.05527454908752621465, 0.1099660938819831402, 0.1632474428518071730, 0.2180761854823636270, 0.2733008743735952928, 0.3309093000114374239, 0.3909945233652084573, 0.4541759534308271173, 0.5188615408488264080, 0.5833105320111698910, 0.6485166818638251618, 0.7150308870971843200, 0.7825020728543330417, 0.8523226850768604868, 0.9249284897844326503, 1.000000000000000000 ),
 ( 0.000000000000000000, 1.000000000000000000 ),
 .UNSPECIFIED. ) ;
#30481 = VERTEX_POINT ( 'NONE', #54609 ) ;
#30482 = VERTEX_POINT ( 'NONE', #86549 ) ;
#30483 = ORIENTED_EDGE ( 'NONE', *, *, #6797, .T. ) ;
#30484 = CARTESIAN_POINT ( 'NONE',  ( -19.99122433398336440, 7.574256484821010105, -1.500000000000002220 ) ) ;
#30485 = ORIENTED_EDGE ( 'NONE', *, *, #22090, .F. ) ;
#30486 = CARTESIAN_POINT ( 'NONE',  ( 8.881738082190086203, 19.07353979602852689, 11.49999999999998934 ) ) ;
#30487 = CARTESIAN_POINT ( 'NONE',  ( -30.60464189315247907, -24.58218713401908317, 0.8299800598022480935 ) ) ;
#30488 = CARTESIAN_POINT ( 'NONE',  ( -41.46355252140796210, -25.28892596830917228, 4.097884790672636335 ) ) ;
#30489 = DIRECTION ( 'NONE',  ( -3.773278334453079618E-23, 0.9999999999976377785, 2.173523156925979975E-06 ) ) ;
#30490 = CARTESIAN_POINT ( 'NONE',  ( 8.537626919312410578, 20.26776412955123163, -1.500000000000002220 ) ) ;
#30491 = CARTESIAN_POINT ( 'NONE',  ( -87.58840615572438537, -24.34968618360935011, 0.1864209137778971292 ) ) ;
#30492 = VERTEX_POINT ( 'NONE', #17539 ) ;
#30493 = CARTESIAN_POINT ( 'NONE',  ( -83.62287095715005592, -29.50250786944525672, 11.44777988621623521 ) ) ;
#30494 = CARTESIAN_POINT ( 'NONE',  ( 31.13513474936814163, 4.540774720514427543, 3.331262582247520143 ) ) ;
#30495 = CIRCLE ( 'NONE', #87152, 0.8500000000000017542 ) ;
#30496 = DIRECTION ( 'NONE',  ( -0.000000000000000000, -0.000000000000000000, 1.000000000000000000 ) ) ;
#30497 = CARTESIAN_POINT ( 'NONE',  ( -33.62287095715005592, -23.48783264082477373, -1.443836473390074371 ) ) ;
#30498 = CARTESIAN_POINT ( 'NONE',  ( -30.62049582358472222, -24.26855077790994386, 9.960784317162937995 ) ) ;
#30499 = CARTESIAN_POINT ( 'NONE',  ( 12.11089201280794470, -17.53110042540249225, -1.500000000000002220 ) ) ;
#30500 = CARTESIAN_POINT ( 'NONE',  ( -98.62981689697267029, -24.15620529776628800, 10.23563542870660292 ) ) ;
#30501 = CARTESIAN_POINT ( 'NONE',  ( -27.68651082257923335, -24.75185970166884175, 2.274903409718059599 ) ) ;
#30502 = CARTESIAN_POINT ( 'NONE',  ( 0.7395552074414004640, -5.331939213628641205, -9.000000000000000000 ) ) ;
#30503 = AXIS2_PLACEMENT_3D ( 'NONE', #61771, #70369, #92690 ) ;
#30504 = CARTESIAN_POINT ( 'NONE',  ( -70.52287095715007581, -24.91544648472625667, 1.928969306349430868 ) ) ;
#30505 = CARTESIAN_POINT ( 'NONE',  ( 22.08653571170524543, -4.319401766784854324, -1.500000000000002220 ) ) ;
#30506 = ADVANCED_FACE ( 'NONE', ( #70331, #47497, #100246, #93148, #69326, #54120, #70834, #48001, #9420, #85043, #15529, #86048 ), #55531, .T. ) ;
#30507 = CARTESIAN_POINT ( 'NONE',  ( -110.9396397263220990, -25.30561928443788133, 5.929683345795315752 ) ) ;
#30508 = ORIENTED_EDGE ( 'NONE', *, *, #82207, .T. ) ;
#30509 = EDGE_CURVE ( 'NONE', #4409, #55534, #16845, .T. ) ;
#30510 = CARTESIAN_POINT ( 'NONE',  ( -99.28737118923764626, -25.13419999133549965, 7.096671994546412066 ) ) ;
#30511 = CARTESIAN_POINT ( 'NONE',  ( 18.70796670040472165, 5.986831462552164140, 11.49999999999999645 ) ) ;
#30512 = CARTESIAN_POINT ( 'NONE',  ( -128.6228709571500417, -23.48783264082479505, -1.443836473390056829 ) ) ;
#30513 = VECTOR ( 'NONE', #4613, 1000.000000000000114 ) ;
#30514 = EDGE_CURVE ( 'NONE', #93024, #20487, #12008, .T. ) ;
#30515 = CARTESIAN_POINT ( 'NONE',  ( -27.25988310792305214, -0.3587747205144265483, 30.32664379231667695 ) ) ;
#30516 = ORIENTED_EDGE ( 'NONE', *, *, #66200, .F. ) ;
#30517 = EDGE_CURVE ( 'NONE', #1418, #60061, #12420, .T. ) ;
#30518 = CARTESIAN_POINT ( 'NONE',  ( -50.55620429048337883, -23.48783264082477729, -1.443836473390070152 ) ) ;
#30519 = CARTESIAN_POINT ( 'NONE',  ( -42.62287095715004881, -24.64965695001467694, 8.947790433994187609 ) ) ;
#30520 = CARTESIAN_POINT ( 'NONE',  ( -100.6814946224345846, -25.31439533081184479, 5.197788989161054474 ) ) ;
#30521 = ADVANCED_FACE ( 'NONE', ( #37265 ), #74328, .T. ) ;
#30522 = EDGE_CURVE ( 'NONE', #57524, #99197, #39090, .T. ) ;
#30523 = CARTESIAN_POINT ( 'NONE',  ( -19.47062899137607772, 3.135797168518691169, -1.500000000000002220 ) ) ;
#30524 = ORIENTED_EDGE ( 'NONE', *, *, #25289, .F. ) ;
#30525 = EDGE_CURVE ( 'NONE', #7384, #31760, #43959, .T. ) ;
#30526 = CARTESIAN_POINT ( 'NONE',  ( -120.5228709571500616, -23.48786465467241769, 11.44779295918253759 ) ) ;
#30527 = CARTESIAN_POINT ( 'NONE',  ( -118.5228709571501042, -24.51283580621365488, 0.6167428607019833642 ) ) ;
#30528 = COORDINATED_UNIVERSAL_TIME_OFFSET ( 0, 0, .AHEAD. ) ;
#30529 = EDGE_LOOP ( 'NONE', ( #2036, #58551, #25089, #40873 ) ) ;
#30530 = DIRECTION ( 'NONE',  ( 0.000000000000000000, -1.000000000000000000, 0.000000000000000000 ) ) ;
#30531 = LINE ( 'NONE', #100017, #45829 ) ;
#30532 = CARTESIAN_POINT ( 'NONE',  ( 27.53860345374808105, 1.682774720514426114, 0.000000000000000000 ) ) ;
#30533 = CARTESIAN_POINT ( 'NONE',  ( -99.09546795806416242, -25.26638384523103653, 6.840687619165027655 ) ) ;
#30534 = DIRECTION ( 'NONE',  ( 0.000000000000000000, -1.000000000000000000, 0.000000000000000000 ) ) ;
#30535 = LINE ( 'NONE', #93935, #10056 ) ;
#30536 = CARTESIAN_POINT ( 'NONE',  ( -10.21384395349174490, -6.376774720514426953, 29.49402280011861777 ) ) ;
#30537 = CARTESIAN_POINT ( 'NONE',  ( 19.63333621495807435, 3.783328549194958867, -1.500000000000002220 ) ) ;
#30538 = EDGE_CURVE ( 'NONE', #52671, #13507, #21515, .T. ) ;
#30539 = CARTESIAN_POINT ( 'NONE',  ( -100.2631815169052203, -25.10935038814901787, 2.837686026794785210 ) ) ;
#30540 = CARTESIAN_POINT ( 'NONE',  ( 26.73860345374794534, 5.058662225110310828, -7.113848178280766099 ) ) ;
#30541 = ORIENTED_EDGE ( 'NONE', *, *, #5495, .F. ) ;
#30542 = EDGE_CURVE ( 'NONE', #43961, #28152, #32670, .T. ) ;
#30543 = CARTESIAN_POINT ( 'NONE',  ( -119.5576576810219507, -23.48783264082477373, -1.443836473390087916 ) ) ;
#30544 = CARTESIAN_POINT ( 'NONE',  ( -80.60234139019381416, -23.85049219812686161, 10.88485053497527311 ) ) ;
#30545 = DIRECTION ( 'NONE',  ( -0.000000000000000000, -1.000000000000000000, -0.000000000000000000 ) ) ;
#30546 = CARTESIAN_POINT ( 'NONE',  ( 4.653846153846159517, -5.876774720514419847, 19.99999999999999289 ) ) ;
#30547 = CARTESIAN_POINT ( 'NONE',  ( 3.300000000000006040, 5.449678256205721784E-16, -4.450000000000000178 ) ) ;
#30548 = CARTESIAN_POINT ( 'NONE',  ( -45.55620429048339304, -25.00182538069144655, 7.747789668545097541 ) ) ;
#30549 = B_SPLINE_SURFACE_WITH_KNOTS ( 'NONE', 3, 3, ( 
 ( #71136, #48810, #8733, #39670 ),
 ( #25453, #95969, #56428, #71636 ),
 ( #3139, #2138, #79735, #26468 ),
 ( #18347, #32060, #17849, #72145 ),
 ( #63035, #1630, #10231, #2632 ),
 ( #25956, #87859, #86843, #64050 ),
 ( #93956, #34080, #80244, #24447 ) ),
 .UNSPECIFIED., .F., .F., .F.,
 ( 4, 3, 4 ),
 ( 4, 4 ),
 ( 0.7945040050992248082, 0.8970133687736506767, 0.9995227324480765452 ),
 ( 0.7096743353268654131, 0.7110146926484223195 ),
 .UNSPECIFIED. ) ;
#30550 = DIRECTION ( 'NONE',  ( -1.000000000000000000, -1.413818403454611288E-16, 0.000000000000000000 ) ) ;
#30551 = CARTESIAN_POINT ( 'NONE',  ( -40.52287095715006870, -24.14406661686763300, 10.28769366194071466 ) ) ;
#30552 = ORIENTED_EDGE ( 'NONE', *, *, #82441, .T. ) ;
#30553 = CARTESIAN_POINT ( 'NONE',  ( -16.53579703214142427, -11.71821515807347680, -1.500000000000002220 ) ) ;
#30554 = CARTESIAN_POINT ( 'NONE',  ( -122.5889747868830284, -24.51314013834316086, 0.6176544820404212821 ) ) ;
#30555 = B_SPLINE_CURVE_WITH_KNOTS ( 'NONE', 3,
 ( #43555, #88735, #64920, #95835 ),
 .UNSPECIFIED., .F., .F.,
 ( 4, 4 ),
 ( 0.9404574821454589895, 0.9494639134175745232 ),
 .UNSPECIFIED. ) ;
#30556 = CARTESIAN_POINT ( 'NONE',  ( -33.62287095715005592, -29.50250243563736774, 8.947779886222150481 ) ) ;
#30557 = VECTOR ( 'NONE', #6335, 1000.000000000000114 ) ;
#30558 = B_SPLINE_CURVE_WITH_KNOTS ( 'NONE', 3,
 ( #46962, #77883, #8389, #39337, #70298, #779 ),
 .UNSPECIFIED., .F., .F.,
 ( 4, 2, 4 ),
 ( 0.000000000000000000, 0.001380901958385388545, 0.002761803916770777089 ),
 .UNSPECIFIED. ) ;
#30559 = CARTESIAN_POINT ( 'NONE',  ( -40.94687764114259920, -25.04307374350000259, 7.563175304812659761 ) ) ;
#30561 = EDGE_LOOP ( 'NONE', ( #78569, #26520, #26837, #25460 ) ) ;
#30560 = ADVANCED_FACE ( 'NONE', ( #59611 ), #36269, .T. ) ;
#30562 = PLANE ( 'NONE',  #1603 ) ;
#30563 = CARTESIAN_POINT ( 'NONE',  ( -9.210493908506615313, -17.87979239004878451, -1.500000000000002220 ) ) ;
#30564 = CARTESIAN_POINT ( 'NONE',  ( -20.42954818520503935, 5.180689535515515587, 11.49999999999999645 ) ) ;
#30565 = CARTESIAN_POINT ( 'NONE',  ( -32.58953762381672448, -24.65952944569304606, 1.056160979905698571 ) ) ;
#30566 = CARTESIAN_POINT ( 'NONE',  ( -13.28819421967561532, -17.68372732473523001, -1.500000000000002220 ) ) ;
#30567 = EDGE_CURVE ( 'NONE', #8495, #13454, #90052, .T. ) ;
#30568 = CARTESIAN_POINT ( 'NONE',  ( 17.96566822227200433, 9.963707542159163211, -1.500000000000002220 ) ) ;
#30569 = CARTESIAN_POINT ( 'NONE',  ( -70.52287095715007581, -29.50248789122583659, 2.256150453626215580 ) ) ;
#30570 = CARTESIAN_POINT ( 'NONE',  ( -60.64004623127358684, -24.40034930558990922, 0.3402023900116026289 ) ) ;
#30571 = ORIENTED_EDGE ( 'NONE', *, *, #18792, .T. ) ;
#30572 = LINE ( 'NONE', #22935, #59019 ) ;
#30573 = ORIENTED_EDGE ( 'NONE', *, *, #82640, .F. ) ;
#30574 = CARTESIAN_POINT ( 'NONE',  ( -6.499903988472228278, -6.376774720514408301, 19.18381548539529646 ) ) ;
#30575 = DIRECTION ( 'NONE',  ( -3.773278334453079618E-23, 0.9999999999976377785, 2.173523156925979975E-06 ) ) ;
#30576 = ORIENTED_EDGE ( 'NONE', *, *, #28294, .T. ) ;
#30577 = ORIENTED_EDGE ( 'NONE', *, *, #62022, .T. ) ;
#30578 = AXIS2_PLACEMENT_3D ( 'NONE', #16196, #77586, #54782 ) ;
#30579 = ORIENTED_EDGE ( 'NONE', *, *, #17394, .T. ) ;
#30580 = DIRECTION ( 'NONE',  ( 0.9980236263794188822, 0.000000000000000000, -0.06283980576413537855 ) ) ;
#30581 = CARTESIAN_POINT ( 'NONE',  ( -49.25194410911545617, -25.12154037719012933, 7.110284505066584160 ) ) ;
#30582 = CARTESIAN_POINT ( 'NONE',  ( 14.76093561896379214, 6.475225279485574248, -27.37148769130089931 ) ) ;
#30583 = CARTESIAN_POINT ( 'NONE',  ( 3.034461355793923509, -20.43525710956717845, -1.500000000000002220 ) ) ;
#30584 = CARTESIAN_POINT ( 'NONE',  ( 9.069627533930374241, 19.64968329815391712, 11.49999999999999645 ) ) ;
#30585 = ORIENTED_EDGE ( 'NONE', *, *, #95286, .T. ) ;
#30586 = DIRECTION ( 'NONE',  ( 0.000000000000000000, 1.000000000000000000, 0.000000000000000000 ) ) ;
#30587 = PLANE ( 'NONE',  #95060 ) ;
#30588 = CARTESIAN_POINT ( 'NONE',  ( -21.65924713590726469, 5.634197536097032888, -1.500000000000002220 ) ) ;
#30589 = DIRECTION ( 'NONE',  ( 0.000000000000000000, -2.173523156925979552E-06, 0.9999999999976378895 ) ) ;
#30590 = CARTESIAN_POINT ( 'NONE',  ( -82.62287095715005592, -23.47593901973091235, -1.443836447539004642 ) ) ;
#30591 = ORIENTED_EDGE ( 'NONE', *, *, #90840, .T. ) ;
#30592 = CARTESIAN_POINT ( 'NONE',  ( 33.34043384136952426, -4.658726884274800639, -12.67806891602219821 ) ) ;
#30593 = FACE_OUTER_BOUND ( 'NONE', #83227, .T. ) ;
#30594 = CARTESIAN_POINT ( 'NONE',  ( -115.5228709571500332, -24.51163499207174823, 0.6490370598554319193 ) ) ;
#30595 = CARTESIAN_POINT ( 'NONE',  ( -16.12721948686093754, -13.32240427740599564, -1.500000000000002220 ) ) ;
#30596 = ORIENTED_EDGE ( 'NONE', *, *, #64232, .F. ) ;
#30597 = CARTESIAN_POINT ( 'NONE',  ( -86.58308328051593605, -24.65952944569304606, 1.056160979905700126 ) ) ;
#30598 = EDGE_LOOP ( 'NONE', ( #32336, #25890, #86918, #75991 ) ) ;
#30599 = VECTOR ( 'NONE', #67245, 1000.000000000000114 ) ;
#30600 = CARTESIAN_POINT ( 'NONE',  ( -50.62287095715005592, -24.99156045073392463, 7.747789690856161648 ) ) ;
#30601 = CARTESIAN_POINT ( 'NONE',  ( 18.56724428474754518, 10.22298014144217859, -1.500000000000002220 ) ) ;
#30602 = ORIENTED_EDGE ( 'NONE', *, *, #93173, .F. ) ;
#30603 = CARTESIAN_POINT ( 'NONE',  ( -117.6270223626581384, -23.96119346886881019, -0.6495511937831995875 ) ) ;
#30604 = CARTESIAN_POINT ( 'NONE',  ( -99.87501341000351829, -25.26221294576034637, 6.992709272975608847 ) ) ;
#30605 = CARTESIAN_POINT ( 'NONE',  ( 21.06710269851327766, -5.618397932909799941, -1.500000000000002220 ) ) ;
#30606 = FACE_OUTER_BOUND ( 'NONE', #43176, .T. ) ;
#30607 = DIRECTION ( 'NONE',  ( -3.773278334444167608E-23, 1.000000000000000000, 0.000000000000000000 ) ) ;
#30608 = CARTESIAN_POINT ( 'NONE',  ( -84.62287095715005592, -24.64965695001469115, 8.947790433994182280 ) ) ;
#30609 = CARTESIAN_POINT ( 'NONE',  ( -15.04333773895388937, -15.80532200100455498, -1.500000000000002220 ) ) ;
#30610 = CARTESIAN_POINT ( 'NONE',  ( -41.55620429048340014, -24.64898659630529210, 1.056161002820823036 ) ) ;
#30611 = ORIENTED_EDGE ( 'NONE', *, *, #7194, .T. ) ;
#30612 = CARTESIAN_POINT ( 'NONE',  ( 25.90623483695386042, 5.165022820506127488, -7.573688418739351391 ) ) ;
#30613 = CARTESIAN_POINT ( 'NONE',  ( 0.7051282051282027341, -5.876774720514409189, 19.19230769230768985 ) ) ;
#30614 = CARTESIAN_POINT ( 'NONE',  ( 32.15269211224249091, -4.540774720514427543, 3.401810532325273861 ) ) ;
#30615 = ORIENTED_EDGE ( 'NONE', *, *, #42697, .F. ) ;
#30616 = ORIENTED_EDGE ( 'NONE', *, *, #59401, .T. ) ;
#30617 = EDGE_LOOP ( 'NONE', ( #34929, #59658, #6427, #41323, #60113 ) ) ;
#30618 = CARTESIAN_POINT ( 'NONE',  ( -125.9228709571500531, -23.47596703998600631, 11.44779298504227860 ) ) ;
#30619 = CARTESIAN_POINT ( 'NONE',  ( 3.302162439418223627, -20.95225242093645690, -1.500000000000002220 ) ) ;
#30620 = CARTESIAN_POINT ( 'NONE',  ( -119.6228709571500559, -24.64965695001469115, 8.947790433994175174 ) ) ;
#30621 = CARTESIAN_POINT ( 'NONE',  ( -79.02216967728209340, -25.03138069755155470, 6.505901493516774714 ) ) ;
#30622 = B_SPLINE_CURVE_WITH_KNOTS ( 'NONE', 3,
 ( #63474, #69567, #45, #99963, #94371, #46200 ),
 .UNSPECIFIED., .F., .F.,
 ( 4, 2, 4 ),
 ( 0.000000000000000000, 0.001380764517853247516, 0.002761529035706495033 ),
 .UNSPECIFIED. ) ;
#30623 = DIRECTION ( 'NONE',  ( 0.000000000000000000, -2.173523156925979552E-06, 0.9999999999976378895 ) ) ;
#30624 = CARTESIAN_POINT ( 'NONE',  ( 5.742690948595683409, -5.876774720514426953, 21.62260900090680593 ) ) ;
#30625 = CARTESIAN_POINT ( 'NONE',  ( -17.02366064725396555, -9.230830265533395362, 11.49999999999998934 ) ) ;
#30626 = EDGE_CURVE ( 'NONE', #77342, #36478, #68715, .T. ) ;
#30627 = CARTESIAN_POINT ( 'NONE',  ( -69.48331070941586063, -25.29418496701295282, 5.732640622402496611 ) ) ;
#30628 = ORIENTED_EDGE ( 'NONE', *, *, #95726, .T. ) ;
#30629 = VECTOR ( 'NONE', #30814, 1000.000000000000114 ) ;
#30630 = EDGE_CURVE ( 'NONE', #96177, #70011, #13251, .T. ) ;
#30631 = CARTESIAN_POINT ( 'NONE',  ( -19.46337940159461866, -0.4807646128305608779, 11.49999999999999645 ) ) ;
#30632 = CARTESIAN_POINT ( 'NONE',  ( -107.6228709571500701, -23.47596703998600631, 11.44779298504227860 ) ) ;
#30633 = VECTOR ( 'NONE', #97207, 1000.000000000000000 ) ;
#30634 = CARTESIAN_POINT ( 'NONE',  ( -49.62287095715007013, -24.50321055353804667, 9.387540953477540029 ) ) ;
#30635 = ORIENTED_EDGE ( 'NONE', *, *, #58853, .T. ) ;
#30636 = EDGE_CURVE ( 'NONE', #96384, #11381, #21024, .T. ) ;
#30637 = CARTESIAN_POINT ( 'NONE',  ( 2.834823996951755465, -6.376774720514406525, 18.76222163777333307 ) ) ;
#30638 = CARTESIAN_POINT ( 'NONE',  ( -8.376690734369036662, 12.50000000000004974, 2.100000000000000089 ) ) ;
#30639 = AXIS2_PLACEMENT_3D ( 'NONE', #34850, #97244, #73417 ) ;
#30640 = EDGE_CURVE ( 'NONE', #3242, #76617, #71324, .T. ) ;
#30641 = DIRECTION ( 'NONE',  ( 0.000000000000000000, -0.9999999999976377785, -2.173523156925979975E-06 ) ) ;
#30642 = CARTESIAN_POINT ( 'NONE',  ( -55.62287095715004881, -23.85196035786900026, -0.8779234886474988064 ) ) ;
#30643 = CARTESIAN_POINT ( 'NONE',  ( -8.122062702759739850, 17.86989387945112995, -1.500000000000002220 ) ) ;
#30644 = EDGE_CURVE ( 'NONE', #12095, #9929, #66495, .T. ) ;
#30645 = CARTESIAN_POINT ( 'NONE',  ( -41.42418673051398770, -25.31583634048925902, 4.451103923698910947 ) ) ;
#30646 = ORIENTED_EDGE ( 'NONE', *, *, #50080, .F. ) ;
#30647 = CARTESIAN_POINT ( 'NONE',  ( 10.40854797073303395, 18.91789161722374146, -1.500000000000002220 ) ) ;
#30648 = VECTOR ( 'NONE', #83951, 1000.000000000000000 ) ;
#30649 = B_SPLINE_CURVE_WITH_KNOTS ( 'NONE', 3,
 ( #8751, #55939, #48828, #39689, #40200, #70648, #32078, #1646, #16856, #10247, #32581, #41209, #63561, #72162, #66065, #43701, #89870, #88377 ),
 .UNSPECIFIED., .F., .F.,
 ( 4, 2, 2, 2, 2, 2, 2, 2, 4 ),
 ( 0.000000000000000000, 0.0002916214222385914677, 0.0005832428444771829354, 0.0008748642667157744031, 0.001166485688954365871, 0.001458107111192957338, 0.001749728533431548806, 0.002041349955670140274, 0.002332971377908731742 ),
 .UNSPECIFIED. ) ;
#30650 = CARTESIAN_POINT ( 'NONE',  ( 22.81105451610979173, 500000.0000000000582, -20.71691820600746681 ) ) ;
#30651 = ADVANCED_FACE ( 'NONE', ( #14904 ), #45878, .F. ) ;
#30652 = DIRECTION ( 'NONE',  ( 0.000000000000000000, 1.000000000000000000, 1.020425574104004246E-16 ) ) ;
#30653 = LINE ( 'NONE', #1211, #66669 ) ;
#30654 = CARTESIAN_POINT ( 'NONE',  ( -20.90396053131702914, -9.656267258341529214, -1.500000000000002220 ) ) ;
#30655 = PERSON_AND_ORGANIZATION ( #70597, #27821 ) ;
#30656 = CARTESIAN_POINT ( 'NONE',  ( -127.5228709571500616, -23.47593901973090524, -1.443836447538996204 ) ) ;
#30657 = CARTESIAN_POINT ( 'NONE',  ( 4.653726706778644306, -6.376774720514415407, 20.04674869880385302 ) ) ;
#30658 = CARTESIAN_POINT ( 'NONE',  ( 18.63370447891095694, 7.782165041754079304, 11.49999999999999645 ) ) ;
#30659 = CARTESIAN_POINT ( 'NONE',  ( 6.424528460793287543, -6.376774720514413630, 19.73230822599986212 ) ) ;
#30660 = CARTESIAN_POINT ( 'NONE',  ( -101.7482071278742808, -25.17643464477231063, 6.839252989080933709 ) ) ;
#30661 = CIRCLE ( 'NONE', #98664, 4.080000000000000071 ) ;
#30662 = CARTESIAN_POINT ( 'NONE',  ( -57.62287095715004881, -24.64965695001468404, 8.947790433994185832 ) ) ;
#30663 = CARTESIAN_POINT ( 'NONE',  ( -129.6238141773120560, -23.73766607897671577, -1.055555164236443577 ) ) ;
#30664 = CARTESIAN_POINT ( 'NONE',  ( -111.3663525145439053, -25.18425782680516178, 4.214194604219601459 ) ) ;
#30665 = CARTESIAN_POINT ( 'NONE',  ( 4.300141163375406528, 19.41444791797076874, 11.49999999999998934 ) ) ;
#30666 = CARTESIAN_POINT ( 'NONE',  ( -118.5228709571500758, -23.48786465467241769, 11.44779295918253759 ) ) ;
#30667 = CARTESIAN_POINT ( 'NONE',  ( 14.04693994163893578, -13.95676237773968609, -1.500000000000002220 ) ) ;
#30668 = CARTESIAN_POINT ( 'NONE',  ( -56.49251241998729256, -24.51314013834315730, 0.6176544820404098468 ) ) ;
#30669 = CARTESIAN_POINT ( 'NONE',  ( -39.57984969116796492, -25.10925652639403793, 3.109569470329076157 ) ) ;
#30670 = DIRECTION ( 'NONE',  ( -0.6599726524652352877, 0.000000000000000000, 0.7512896232465891000 ) ) ;
#30671 = CARTESIAN_POINT ( 'NONE',  ( 10.87737074370964407, 17.65887017642603851, 11.49999999999999645 ) ) ;
#30672 = CARTESIAN_POINT ( 'NONE',  ( -53.52287095715005449, -24.66019654487198665, 8.947790411086121054 ) ) ;
#30673 = CARTESIAN_POINT ( 'NONE',  ( -50.34100630499489881, -25.31439277421117851, 5.198616746494224117 ) ) ;
#30674 = VECTOR ( 'NONE', #100137, 1000.000000000000114 ) ;
#30675 = CARTESIAN_POINT ( 'NONE',  ( 21.55457256799317278, 7.124301260279622738, 11.49999999999999645 ) ) ;
#30676 = VERTEX_POINT ( 'NONE', #61615 ) ;
#30677 = CARTESIAN_POINT ( 'NONE',  ( -11.64875734969026233, 0.3587747205144265483, 30.51402280011862089 ) ) ;
#30678 = LINE ( 'NONE', #53536, #38675 ) ;
#30679 = CARTESIAN_POINT ( 'NONE',  ( 19.60372117168125072, 4.849774137724135237, 11.49999999999998934 ) ) ;
#30680 = CARTESIAN_POINT ( 'NONE',  ( 8.991545460846683824, -0.9385453280025082279, -3.722136940144805450 ) ) ;
#30681 = CARTESIAN_POINT ( 'NONE',  ( -52.58953762381671737, -23.47593901973091235, -1.443836447539009749 ) ) ;
#30682 = VERTEX_POINT ( 'NONE', #85422 ) ;
#30683 = ORIENTED_EDGE ( 'NONE', *, *, #83123, .F. ) ;
#30684 = CARTESIAN_POINT ( 'NONE',  ( 0.09189959430841809773, -5.876774720514410077, 19.67013632031035542 ) ) ;
#30685 = CARTESIAN_POINT ( 'NONE',  ( 22.67525425759127344, 3.225002893152739247, -1.500000000000002220 ) ) ;
#30686 = CARTESIAN_POINT ( 'NONE',  ( -50.97853604095990221, -25.27420597387646595, 3.451784371543335617 ) ) ;
#30687 = B_SPLINE_CURVE_WITH_KNOTS ( 'NONE', 3,
 ( #46482, #34760, #2822, #9915, #94652, #49499 ),
 .UNSPECIFIED., .F., .F.,
 ( 4, 2, 4 ),
 ( 1.570887131794952276E-05, 0.001396322306279766711, 0.002776935741241583645 ),
 .UNSPECIFIED. ) ;
#30688 = CARTESIAN_POINT ( 'NONE',  ( -7.466173891270859286, -20.28576548065916541, -1.500000000000002220 ) ) ;
#30689 = DIRECTION ( 'NONE',  ( 1.000000000000000000, 3.773278334444167608E-23, 8.201307833595939069E-29 ) ) ;
#30690 = CARTESIAN_POINT ( 'NONE',  ( -34.57049221944907913, -23.48783264082478084, -1.443836473390076591 ) ) ;
#30691 = CARTESIAN_POINT ( 'NONE',  ( 12.70736309587848645, -16.60074808024427284, 11.49999999999999645 ) ) ;
#30692 = ORIENTED_EDGE ( 'NONE', *, *, #68333, .F. ) ;
#30693 = CARTESIAN_POINT ( 'NONE',  ( -124.6261987484861748, -23.48783264082478084, -1.443836473390086361 ) ) ;
#30694 = CARTESIAN_POINT ( 'NONE',  ( -20.87105610827876134, -7.033761084331515256, 11.49999999999998934 ) ) ;
#30695 = EDGE_CURVE ( 'NONE', #42749, #58613, #32136, .T. ) ;
#30696 = MANIFOLD_SURFACE_SHAPE_REPRESENTATION ( '', ( #29565, #218 ), #69909 ) ;
#30697 = CARTESIAN_POINT ( 'NONE',  ( -105.5519745381963190, -24.40133493613049964, 9.663955038902797057 ) ) ;
#30698 = CYLINDRICAL_SURFACE ( 'NONE', #7480, 1.249999999999997558 ) ;
#30699 = EDGE_LOOP ( 'NONE', ( #1008, #61422 ) ) ;
#30700 = CARTESIAN_POINT ( 'NONE',  ( -73.62287095715005592, -23.47593901973091235, -1.443836447539006196 ) ) ;
#30701 = EDGE_CURVE ( 'NONE', #69181, #73710, #63616, .T. ) ;
#30702 = CARTESIAN_POINT ( 'NONE',  ( -46.55620429048338593, -23.48783264082477729, -1.443836473390070596 ) ) ;
#30703 = EDGE_LOOP ( 'NONE', ( #64128, #88280, #35272, #10998, #24083, #45214, #66184, #34576, #59324, #8284, #69894, #40700, #59051, #57826 ) ) ;
#30704 = CARTESIAN_POINT ( 'NONE',  ( -72.63936762441933581, -23.96169478059713143, 10.65365249895718414 ) ) ;
#30705 = EDGE_LOOP ( 'NONE', ( #67233, #16620, #68042 ) ) ;
#30706 = VECTOR ( 'NONE', #79873, 1000.000000000000114 ) ;
#30707 = ORIENTED_EDGE ( 'NONE', *, *, #59638, .T. ) ;
#30708 = FACE_OUTER_BOUND ( 'NONE', #64589, .T. ) ;
#30709 = CARTESIAN_POINT ( 'NONE',  ( 33.74607884027702909, 5.965225279485572685, -4.999864028243830916 ) ) ;
#30710 = CARTESIAN_POINT ( 'NONE',  ( -4.141439336867657417, -5.876774720514418071, 20.56083401959468304 ) ) ;
#30711 = CARTESIAN_POINT ( 'NONE',  ( 19.83930831332124001, -5.160774681608516268, -1.500000000000002220 ) ) ;
#30712 = ORIENTED_EDGE ( 'NONE', *, *, #36887, .T. ) ;
#30713 = CARTESIAN_POINT ( 'NONE',  ( 17.47419131657910540, 5.965225279485572685, 28.31804950686278843 ) ) ;
#30714 = CIRCLE ( 'NONE', #69617, 2.040000000000000036 ) ;
#30715 = LINE ( 'NONE', #62681, #17407 ) ;
#30716 = CARTESIAN_POINT ( 'NONE',  ( -29.49875734969025842, 5.965225279485572685, 25.61802280011862720 ) ) ;
#30717 = CARTESIAN_POINT ( 'NONE',  ( -5.617636847906702258, 21.56867655435222630, -1.500000000000002220 ) ) ;
#30718 = PLANE ( 'NONE',  #2750 ) ;
#30719 = CARTESIAN_POINT ( 'NONE',  ( -47.62287095715004881, -23.48786465467240703, 11.44779295918255180 ) ) ;
#30720 = ORIENTED_EDGE ( 'NONE', *, *, #58212, .T. ) ;
#30721 = CARTESIAN_POINT ( 'NONE',  ( -28.43450822049934956, -24.70030246006994901, 1.766382807631876606 ) ) ;
#30722 = AXIS2_PLACEMENT_3D ( 'NONE', #14210, #69010, #74618 ) ;
#30723 = CARTESIAN_POINT ( 'NONE',  ( -29.12273499046074221, -24.63645922367957297, 7.596952268176241141 ) ) ;
#30724 = AXIS2_PLACEMENT_3D ( 'NONE', #22423, #8728, #54402 ) ;
#30725 = CARTESIAN_POINT ( 'NONE',  ( -17.17656601037699104, 11.78060583124977256, -1.500000000000002220 ) ) ;
#30726 = ORIENTED_EDGE ( 'NONE', *, *, #96905, .T. ) ;
#30728 = EDGE_LOOP ( 'NONE', ( #7346, #33336, #60691, #15948 ) ) ;
#30727 = FACE_OUTER_BOUND ( 'NONE', #39712, .T. ) ;
#30729 = CIRCLE ( 'NONE', #61523, 2.249999999999998668 ) ;
#30730 = CARTESIAN_POINT ( 'NONE',  ( -51.52241826985714113, -25.25854396960094661, 6.308158736584201343 ) ) ;
#30731 = ORIENTED_EDGE ( 'NONE', *, *, #79716, .F. ) ;
#30732 = ORIENTED_EDGE ( 'NONE', *, *, #84386, .T. ) ;
#30733 = LINE ( 'NONE', #53592, #88342 ) ;
#30734 = CARTESIAN_POINT ( 'NONE',  ( -92.62287095715008434, -23.73934037231758154, 11.05740245334329153 ) ) ;
#30735 = CARTESIAN_POINT ( 'NONE',  ( -77.62287095715007013, -24.66019654487199730, 8.947790411086128159 ) ) ;
#30736 = CARTESIAN_POINT ( 'NONE',  ( -36.62287095715005592, -29.50250243563736774, 8.947779886222148704 ) ) ;
#30737 = CARTESIAN_POINT ( 'NONE',  ( -92.63388132361646399, -23.96169478059713498, 10.65365249895717881 ) ) ;
#30738 = DIRECTION ( 'NONE',  ( -3.773278334453080206E-23, 0.9999999999976377785, 2.173523156925979975E-06 ) ) ;
#30740 = ORIENTED_EDGE ( 'NONE', *, *, #77135, .F. ) ;
#30739 = CARTESIAN_POINT ( 'NONE',  ( -15.97456084408017674, 15.39233244482803009, 11.49999999999999645 ) ) ;
#30741 = DIRECTION ( 'NONE',  ( -3.773278334453079030E-23, 0.9999999999976377785, 2.173523156925979128E-06 ) ) ;
#30742 = ORIENTED_EDGE ( 'NONE', *, *, #7552, .F. ) ;
#30743 = CARTESIAN_POINT ( 'NONE',  ( -15.40814491850785650, 16.58152744545821022, -1.500000000000002220 ) ) ;
#30745 = VERTEX_POINT ( 'NONE', #9296 ) ;
#30744 = CARTESIAN_POINT ( 'NONE',  ( -111.5228709571500616, -23.48786465467242479, 11.44779295918253936 ) ) ;
#30746 = VERTEX_POINT ( 'NONE', #93028 ) ;
#30747 = CARTESIAN_POINT ( 'NONE',  ( -29.49875734969025842, 5.965225279485572685, 17.86602280011862476 ) ) ;
#30748 = CARTESIAN_POINT ( 'NONE',  ( -4.889416449700032530, -19.50743224814450016, 11.49999999999998934 ) ) ;
#30749 = B_SPLINE_SURFACE_WITH_KNOTS ( 'NONE', 3, 3, ( 
 ( #58845, #59338, #74560, #44614 ),
 ( #75540, #6044, #91282, #42633 ),
 ( #35004, #65985, #96902, #27396 ),
 ( #58356, #89292, #93776, #39500 ),
 ( #24267, #14145, #70449, #77042 ),
 ( #8040, #55241, #14651, #99385 ),
 ( #38498, #45123, #6549, #92768 ) ),
 .UNSPECIFIED., .F., .F., .F.,
 ( 4, 3, 4 ),
 ( 4, 4 ),
 ( 0.7945040050992250302, 0.8970133687736506767, 0.9995227324480763231 ),
 ( 0.4896184160691255394, 0.4908571809756236970 ),
 .UNSPECIFIED. ) ;
#30750 = CARTESIAN_POINT ( 'NONE',  ( -80.62287095715005592, -24.83602698348159876, 1.605859176311268399 ) ) ;
#30751 = ORIENTED_EDGE ( 'NONE', *, *, #16895, .F. ) ;
#30752 = CARTESIAN_POINT ( 'NONE',  ( -92.58953762381672448, -23.48786465467241413, 11.44779295918254469 ) ) ;
#30753 = CARTESIAN_POINT ( 'NONE',  ( -18.01732314745861530, 13.19606014829601826, -1.500000000000002220 ) ) ;
#30754 = VERTEX_POINT ( 'NONE', #1205 ) ;
#30755 = ORIENTED_EDGE ( 'NONE', *, *, #52529, .F. ) ;
#30756 = CARTESIAN_POINT ( 'NONE',  ( -101.3987937098823409, -25.25341184233823100, 6.605698944729169853 ) ) ;
#30757 = DIRECTION ( 'NONE',  ( -3.773278334453079030E-23, 0.9999999999976377785, 2.173523156925979128E-06 ) ) ;
#30758 = EDGE_CURVE ( 'NONE', #58273, #90958, #14518, .T. ) ;
#30759 = PLANE ( 'NONE',  #53894 ) ;
#30760 = CARTESIAN_POINT ( 'NONE',  ( -68.52287095715004739, -24.35013146730202749, 9.818937971375110152 ) ) ;
#30761 = ADVANCED_FACE ( 'NONE', ( #55490 ), #16404, .T. ) ;
#30762 = CARTESIAN_POINT ( 'NONE',  ( 13.32458981842495049, 5.152774720514427642, -26.34181586963115507 ) ) ;
#30763 = CARTESIAN_POINT ( 'NONE',  ( 9.052818235119415746, 17.31195010612007223, 11.49999999999998934 ) ) ;
#30764 = ADVANCED_FACE ( 'NONE', ( #86431 ), #3424, .T. ) ;
#30765 = CARTESIAN_POINT ( 'NONE',  ( -102.5228709571500900, -24.34917612407034682, 0.1852690917477876065 ) ) ;
#30766 = CARTESIAN_POINT ( 'NONE',  ( -18.34654256122676941, -11.15389649534839833, -1.500000000000002220 ) ) ;
#30767 = CARTESIAN_POINT ( 'NONE',  ( -25.97212670940007584, -24.92774901861465153, 2.712286590796212593 ) ) ;
#30768 = ADVANCED_FACE ( 'NONE', ( #32640 ), #38246, .T. ) ;
#30769 = FACE_OUTER_BOUND ( 'NONE', #883, .T. ) ;
#30770 = CARTESIAN_POINT ( 'NONE',  ( -59.55620429048337883, -23.48783264082478084, -1.443836473390068820 ) ) ;
#30771 = AXIS2_PLACEMENT_3D ( 'NONE', #80347, #88469, #80855 ) ;
#30772 = LINE ( 'NONE', #93660, #95827 ) ;
#30773 = CARTESIAN_POINT ( 'NONE',  ( 15.42672287639063100, 16.92133821996916865, -1.500000000000002220 ) ) ;
#30774 = PERSON_AND_ORGANIZATION ( #70597, #27821 ) ;
#30775 = CARTESIAN_POINT ( 'NONE',  ( -96.63904445658880604, -23.48786465467241058, 11.44779295918254469 ) ) ;
#30776 = CARTESIAN_POINT ( 'NONE',  ( -127.5562042904833930, -23.47593901973091235, -1.443836447538995760 ) ) ;
#30777 = CARTESIAN_POINT ( 'NONE',  ( 4.397486433803790007, -19.56896378179033036, 11.49999999999999645 ) ) ;
#30778 = CARTESIAN_POINT ( 'NONE',  ( -79.04068788000392942, -25.26612565946948052, 5.390100810327893122 ) ) ;
#30779 = CARTESIAN_POINT ( 'NONE',  ( -113.5562042904834072, -24.64965694238575367, 8.947790433994196491 ) ) ;
#30780 = CIRCLE ( 'NONE', #43754, 1.000000000000000000 ) ;
#30781 = LINE ( 'NONE', #46019, #73293 ) ;
#30782 = CARTESIAN_POINT ( 'NONE',  ( -108.6228709571500559, -23.94994826722515668, -0.6494450866351694218 ) ) ;
#30783 = ORIENTED_EDGE ( 'NONE', *, *, #20459, .F. ) ;
#30784 = ADVANCED_FACE ( 'NONE', ( #84924 ), #690, .F. ) ;
#30785 = CARTESIAN_POINT ( 'NONE',  ( -26.97298592485077506, -24.59688319057676154, 1.763040481647563995 ) ) ;
#30786 = FACE_OUTER_BOUND ( 'NONE', #70548, .T. ) ;
#30787 = CARTESIAN_POINT ( 'NONE',  ( 7.827691340095081607, 20.28360254610759839, 11.49999999999998934 ) ) ;
#30788 = LINE ( 'NONE', #8949, #12315 ) ;
#30789 = AXIS2_PLACEMENT_3D ( 'NONE', #16382, #39721, #40236 ) ;
#30790 = CARTESIAN_POINT ( 'NONE',  ( 13.16580039582533423, -14.52177825760336205, -1.500000000000002220 ) ) ;
#30791 = CARTESIAN_POINT ( 'NONE',  ( -38.52287095715006870, -23.48786465467241058, 11.44779295918255180 ) ) ;
#30792 = VECTOR ( 'NONE', #15125, 1000.000000000000000 ) ;
#30793 = CARTESIAN_POINT ( 'NONE',  ( -110.1668890976376360, -25.31698235040695621, 5.541054210284112713 ) ) ;
#30794 = APPROVAL_ROLE ( '' ) ;
#30795 = AXIS2_PLACEMENT_3D ( 'NONE', #80371, #33699, #56553 ) ;
#30796 = DIRECTION ( 'NONE',  ( 0.000000000000000000, 0.000000000000000000, 1.000000000000000000 ) ) ;
#30797 = CARTESIAN_POINT ( 'NONE',  ( 3.797776442307698286, -6.376774720514427841, 21.83974358974358410 ) ) ;
#30798 = CARTESIAN_POINT ( 'NONE',  ( -9.379331868514380943, 18.20734191464070406, 11.49999999999999645 ) ) ;
#30799 = LINE ( 'NONE', #61267, #3570 ) ;
#30800 = CARTESIAN_POINT ( 'NONE',  ( -120.5166145060558165, -24.92564183028979841, 1.928384488918253536 ) ) ;
#30801 = VECTOR ( 'NONE', #58110, 1000.000000000000114 ) ;
#30802 = VERTEX_POINT ( 'NONE', #38746 ) ;
#30803 = CARTESIAN_POINT ( 'NONE',  ( -99.72794805030189025, -25.26387389937925576, 4.442265393084401381 ) ) ;
#30804 = CARTESIAN_POINT ( 'NONE',  ( -39.56145255469812128, -25.18430974075399575, 3.766659751673692380 ) ) ;
#30805 = FACE_OUTER_BOUND ( 'NONE', #28609, .T. ) ;
#30806 = CARTESIAN_POINT ( 'NONE',  ( -85.62287095714999907, -24.15431212366391378, -0.2830839119429074402 ) ) ;
#30807 = CARTESIAN_POINT ( 'NONE',  ( -25.54628175542703161, -24.61459516021406913, 5.501431625134629577 ) ) ;
#30808 = CARTESIAN_POINT ( 'NONE',  ( 31.68302997424993350, 5.121054483180515149, -3.958552486145202831 ) ) ;
#30809 = EDGE_CURVE ( 'NONE', #80599, #46090, #77406, .T. ) ;
#30810 = CARTESIAN_POINT ( 'NONE',  ( -13.16640216892762894, -18.94680327863774849, 11.49999999999999645 ) ) ;
#30811 = CARTESIAN_POINT ( 'NONE',  ( -10.93939140624874007, -20.02795264745160608, 11.49999999999998934 ) ) ;
#30812 = CARTESIAN_POINT ( 'NONE',  ( -74.60678690070801622, -23.48783264082477018, -1.443836473390096353 ) ) ;
#30813 = CARTESIAN_POINT ( 'NONE',  ( -88.52287095715001897, -24.34917612406836795, 0.1852690917426557116 ) ) ;
#30814 = DIRECTION ( 'NONE',  ( -4.095491270384932624E-17, -0.5144957554275265688, 0.8574929257125440962 ) ) ;
#30815 = CARTESIAN_POINT ( 'NONE',  ( 9.841385673706204429, 20.17164819615926064, 11.49999999999999645 ) ) ;
#30816 = ORIENTED_EDGE ( 'NONE', *, *, #28364, .F. ) ;
#30817 = CARTESIAN_POINT ( 'NONE',  ( -100.6228709571500275, -24.52232992886363405, 0.6492154411906175815 ) ) ;
#30818 = CARTESIAN_POINT ( 'NONE',  ( -43.65487935057238644, -23.73766607897671221, -1.055555164236442689 ) ) ;
#30819 = CARTESIAN_POINT ( 'NONE',  ( 14.12621959167996977, 16.79361087625908056, 11.49999999999998934 ) ) ;
#30820 = EDGE_CURVE ( 'NONE', #97261, #100338, #36281, .T. ) ;
#30821 = B_SPLINE_CURVE_WITH_KNOTS ( 'NONE', 3,
 ( #28474, #92746, #31359, #54711, #90380, #7019 ),
 .UNSPECIFIED., .F., .F.,
 ( 4, 2, 4 ),
 ( 0.000000000000000000, 0.001380901958385392448, 0.002761803916770784895 ),
 .UNSPECIFIED. ) ;
#30822 = CARTESIAN_POINT ( 'NONE',  ( -98.52287095715009002, -24.66019654487200441, 8.947790411086119278 ) ) ;
#30823 = CARTESIAN_POINT ( 'NONE',  ( -87.55455836477378284, -23.96169478059713498, 10.65365249895718058 ) ) ;
#30824 = CARTESIAN_POINT ( 'NONE',  ( -40.66986802185439132, -25.31545374197336074, 5.060077358709395234 ) ) ;
#30825 = CARTESIAN_POINT ( 'NONE',  ( -78.60556800691774981, -23.48783264082477018, -1.443836473390096797 ) ) ;
#30826 = CARTESIAN_POINT ( 'NONE',  ( 13.91401389203221406, -5.356774720514425603, 158.0376437107427137 ) ) ;
#30827 = VERTEX_POINT ( 'NONE', #88937 ) ;
#30828 = CARTESIAN_POINT ( 'NONE',  ( 5.889875310795558150, 19.62242631308348706, -1.500000000000002220 ) ) ;
#30829 = VERTEX_POINT ( 'NONE', #19414 ) ;
#30830 = ORIENTED_EDGE ( 'NONE', *, *, #54196, .F. ) ;
#30831 = ORIENTED_EDGE ( 'NONE', *, *, #17276, .F. ) ;
#30832 = ORIENTED_EDGE ( 'NONE', *, *, #14237, .F. ) ;
#30833 = CARTESIAN_POINT ( 'NONE',  ( -18.41700849636773540, 13.91914711744011157, -1.500000000000002220 ) ) ;
#30834 = CARTESIAN_POINT ( 'NONE',  ( -45.52287095715006160, -24.99132157543083821, 2.256160258750667502 ) ) ;
#30835 = CARTESIAN_POINT ( 'NONE',  ( -18.13051092187696156, -9.059970205480309957, -1.500000000000002220 ) ) ;
#30836 = ORIENTED_EDGE ( 'NONE', *, *, #17646, .T. ) ;
#30837 = CARTESIAN_POINT ( 'NONE',  ( -115.5228709571500474, -23.47593901973090524, -1.443836447538996204 ) ) ;
#30838 = CARTESIAN_POINT ( 'NONE',  ( -92.52216719015747515, -23.48783264082477729, -1.443836473390063713 ) ) ;
#30839 = CARTESIAN_POINT ( 'NONE',  ( -101.2821955461997732, -25.18596798425043559, 6.774419534272953847 ) ) ;
#30840 = CARTESIAN_POINT ( 'NONE',  ( -70.49528693087628994, -24.63355581998385091, 0.9682620441943861067 ) ) ;
#30842 = ORIENTED_EDGE ( 'NONE', *, *, #92389, .T. ) ;
#30841 = CARTESIAN_POINT ( 'NONE',  ( 8.900169022907615357, -19.58186849131130813, 11.49999999999999645 ) ) ;
#30843 = CARTESIAN_POINT ( 'NONE',  ( -79.52287095715006160, -24.66019654487199375, 8.947790411086122830 ) ) ;
#30844 = CARTESIAN_POINT ( 'NONE',  ( -49.10457154551148307, -25.31573627678961103, 3.999772159320571063 ) ) ;
#30845 = VERTEX_POINT ( 'NONE', #86926 ) ;
#30846 = CARTESIAN_POINT ( 'NONE',  ( 20.64725891757762355, 2.036748910689437864, -1.500000000000002220 ) ) ;
#30847 = AXIS2_PLACEMENT_3D ( 'NONE', #15619, #48092, #24731 ) ;
#30848 = ORIENTED_EDGE ( 'NONE', *, *, #62590, .T. ) ;
#30849 = PRODUCT_DEFINITION ( 'UNKNOWN', '', #16510, #82459 ) ;
#30851 = ORIENTED_EDGE ( 'NONE', *, *, #27367, .F. ) ;
#30850 = DIRECTION ( 'NONE',  ( 1.251281512149627050E-16, 0.000000000000000000, -1.000000000000000000 ) ) ;
#30852 = DIRECTION ( 'NONE',  ( 0.000000000000000000, -1.000000000000000000, 0.000000000000000000 ) ) ;
#30853 = ORIENTED_EDGE ( 'NONE', *, *, #29190, .F. ) ;
#30854 = VERTEX_POINT ( 'NONE', #66125 ) ;
#30855 = CARTESIAN_POINT ( 'NONE',  ( 4.190829928318763109, -6.376774720514401196, 18.23548058298382557 ) ) ;
#30856 = CARTESIAN_POINT ( 'NONE',  ( -42.60799034082329229, -23.73791477778911485, 11.05961554403171299 ) ) ;
#30857 = CARTESIAN_POINT ( 'NONE',  ( -65.63886145207663958, -24.40034930558990922, 0.3402023900116040167 ) ) ;
#30858 = CARTESIAN_POINT ( 'NONE',  ( -11.46427080702723522, -18.74017919159951973, 11.49999999999999645 ) ) ;
#30859 = FACE_OUTER_BOUND ( 'NONE', #63304, .T. ) ;
#30860 = CARTESIAN_POINT ( 'NONE',  ( 22.54279463279464579, 0.6884863543687869125, -1.500000000000002220 ) ) ;
#30861 = CARTESIAN_POINT ( 'NONE',  ( -12.80012119340476140, -16.60591428456014640, -1.500000000000002220 ) ) ;
#30862 = CARTESIAN_POINT ( 'NONE',  ( -89.62287095715002749, -24.50216790748206108, 0.6166512839542551694 ) ) ;
#30863 = CARTESIAN_POINT ( 'NONE',  ( -27.96875734969026084, -6.376774720514426953, 26.43402280011862615 ) ) ;
#30864 = VERTEX_POINT ( 'NONE', #34157 ) ;
#30865 = VECTOR ( 'NONE', #72432, 1000.000000000000000 ) ;
#30866 = ORIENTED_EDGE ( 'NONE', *, *, #5648, .T. ) ;
#30867 = AXIS2_PLACEMENT_3D ( 'NONE', #96705, #64798, #80483 ) ;
#30868 = EDGE_LOOP ( 'NONE', ( #15597, #55612, #42285, #27739 ) ) ;
#30869 = CARTESIAN_POINT ( 'NONE',  ( 4.784292611718076849, -5.356774720514425603, -25.54547254883186014 ) ) ;
#30870 = AXIS2_PLACEMENT_3D ( 'NONE', #93282, #33388, #94789 ) ;
#30871 = CARTESIAN_POINT ( 'NONE',  ( -21.45671390985790694, -1.711987587955616119, -1.500000000000002220 ) ) ;
#30872 = CARTESIAN_POINT ( 'NONE',  ( -114.5562042904834072, -23.47593901973091235, -1.443836447538999312 ) ) ;
#30873 = ORIENTED_EDGE ( 'NONE', *, *, #28012, .F. ) ;
#30874 = CARTESIAN_POINT ( 'NONE',  ( 6.572693220633653688, -20.11273663914708365, -1.500000000000002220 ) ) ;
#30875 = LINE ( 'NONE', #92762, #57921 ) ;
#30876 = PLANE ( 'NONE',  #49527 ) ;
#30877 = DIRECTION ( 'NONE',  ( 0.000000000000000000, -0.8406134417706465634, -0.5416355246053453643 ) ) ;
#30878 = DIRECTION ( 'NONE',  ( 0.000000000000000000, 2.173523156925980399E-06, -0.9999999999976378895 ) ) ;
#30879 = CARTESIAN_POINT ( 'NONE',  ( -47.62287095715006302, -23.47596703998600276, 11.44779298504227505 ) ) ;
#30880 = CARTESIAN_POINT ( 'NONE',  ( -21.14524153552446606, 6.695245452574716261, -1.500000000000002220 ) ) ;
#30881 = CARTESIAN_POINT ( 'NONE',  ( -80.62287095715007013, -25.00158670708909625, 2.256160236439165967 ) ) ;
#30882 = EDGE_CURVE ( 'NONE', #64635, #75345, #80826, .T. ) ;
#30883 = ORIENTED_EDGE ( 'NONE', *, *, #63135, .F. ) ;
#30884 = CARTESIAN_POINT ( 'NONE',  ( 13.43165536947796213, -5.965225279485592225, -28.18099828186571187 ) ) ;
#30885 = DIRECTION ( 'NONE',  ( 0.8219392559241307517, 0.08114015731558495148, 0.5637660281018078701 ) ) ;
#30886 = CARTESIAN_POINT ( 'NONE',  ( -126.6234820361467825, -24.65952944569305316, 1.056160979905705455 ) ) ;
#30887 = CARTESIAN_POINT ( 'NONE',  ( 0.3000000000000007661, 0.000000000000000000, 0.000000000000000000 ) ) ;
#30888 = CARTESIAN_POINT ( 'NONE',  ( 16.20606029192996900, -10.75321813762353251, -1.500000000000002220 ) ) ;
#30889 = ADVANCED_FACE ( 'NONE', ( #96540 ), #40758, .F. ) ;
#30890 = CARTESIAN_POINT ( 'NONE',  ( -14.55006661338671847, 15.66751491618662406, 11.49999999999998934 ) ) ;
#30891 = CARTESIAN_POINT ( 'NONE',  ( -62.58331733608945058, -24.51314013834316441, 0.6176544820404141767 ) ) ;
#30892 = PLANE ( 'NONE',  #83538 ) ;
#30893 = EDGE_CURVE ( 'NONE', #71598, #10587, #79312, .T. ) ;
#30894 = CARTESIAN_POINT ( 'NONE',  ( -79.62287095715011276, -24.34917612406837861, 0.1852690917426644546 ) ) ;
#30895 = DIRECTION ( 'NONE',  ( -0.9978940991575085961, 0.000000000000000000, -0.06486421869277853025 ) ) ;
#30896 = CARTESIAN_POINT ( 'NONE',  ( -5.639450322166912777, -21.95568564230989850, -1.500000000000002220 ) ) ;
#30897 = PLANE ( 'NONE',  #80630 ) ;
#30898 = DIRECTION ( 'NONE',  ( -0.000000000000000000, -1.000000000000000000, -0.000000000000000000 ) ) ;
#30899 = CARTESIAN_POINT ( 'NONE',  ( -12.84220538718065185, 15.17226672225704398, 11.49999999999999645 ) ) ;
#30900 = FACE_OUTER_BOUND ( 'NONE', #46852, .T. ) ;
#30901 = EDGE_LOOP ( 'NONE', ( #17523, #84630, #95962, #90163 ) ) ;
#30902 = ADVANCED_FACE ( 'NONE', ( #41265 ), #41779, .T. ) ;
#30903 = DIRECTION ( 'NONE',  ( 8.630470681059372680E-33, 1.084202172485504434E-16, -1.000000000000000000 ) ) ;
#30904 = CARTESIAN_POINT ( 'NONE',  ( -5.960145391809922089, -5.876774720514415407, 20.04104409779160534 ) ) ;
#30905 = DIRECTION ( 'NONE',  ( 0.000000000000000000, -1.000000000000000000, 0.000000000000000000 ) ) ;
#30906 = CARTESIAN_POINT ( 'NONE',  ( 11.52859134480388903, -18.33581920571378632, 11.49999999999998934 ) ) ;
#30907 = PLANE ( 'NONE',  #85256 ) ;
#30908 = CARTESIAN_POINT ( 'NONE',  ( 18.36381783059253081, 6.383776564742674964, -1.500000000000002220 ) ) ;
#30909 = CARTESIAN_POINT ( 'NONE',  ( -114.6228709571500559, -24.64965695001469115, 8.947790433994176951 ) ) ;
#30910 = CARTESIAN_POINT ( 'NONE',  ( -55.57730503950245549, -24.92592662359560762, 8.075495903017996469 ) ) ;
#30911 = CARTESIAN_POINT ( 'NONE',  ( -9.134819693115781902, 17.59984377705169933, 11.49999999999998934 ) ) ;
#30912 = VERTEX_POINT ( 'NONE', #88439 ) ;
#30913 = CARTESIAN_POINT ( 'NONE',  ( 14.62039552936377085, -14.08751720214925207, 11.49999999999999645 ) ) ;
#30914 = CARTESIAN_POINT ( 'NONE',  ( -80.56574368191338920, -23.48783264082477018, -1.443836473390096131 ) ) ;
#30915 = VECTOR ( 'NONE', #95506, 1000.000000000000114 ) ;
#30916 = CARTESIAN_POINT ( 'NONE',  ( 33.50941771711502071, -4.400593307868461146, -12.46354170163592556 ) ) ;
#30917 = ORIENTED_EDGE ( 'NONE', *, *, #3292, .F. ) ;
#30918 = CARTESIAN_POINT ( 'NONE',  ( -0.03676920774744678322, -22.57399371096969531, 8.369064737642425200 ) ) ;
#30919 = FACE_OUTER_BOUND ( 'NONE', #36987, .T. ) ;
#30920 = CARTESIAN_POINT ( 'NONE',  ( -49.20147844880023058, -25.25214510237312737, 5.321223747615992039 ) ) ;
#30921 = CARTESIAN_POINT ( 'NONE',  ( -40.53339838483739044, -24.63419186844611630, 9.035850630976923981 ) ) ;
#30922 = PLANE ( 'NONE',  #43038 ) ;
#30923 = CARTESIAN_POINT ( 'NONE',  ( 18.99975792849237877, 6.539580213093530325, 11.49999999999998934 ) ) ;
#30924 = ADVANCED_FACE ( 'NONE', ( #71715 ), #57002, .T. ) ;
#30925 = CARTESIAN_POINT ( 'NONE',  ( -89.62287095715004170, -24.66019654487199020, 8.947790411086128159 ) ) ;
#30926 = ORIENTED_EDGE ( 'NONE', *, *, #25034, .F. ) ;
#30927 = CARTESIAN_POINT ( 'NONE',  ( -129.5228709571500758, -23.47593901973090524, -1.443836447538996204 ) ) ;
#30928 = AXIS2_PLACEMENT_3D ( 'NONE', #47368, #93022, #23499 ) ;
#30929 = CARTESIAN_POINT ( 'NONE',  ( -15.36296916364455711, -16.94538937337987150, 11.49999999999999645 ) ) ;
#30930 = CARTESIAN_POINT ( 'NONE',  ( -13.93578158028743985, 17.96481793202167054, -1.500000000000002220 ) ) ;
#30931 = VERTEX_POINT ( 'NONE', #9806 ) ;
#30932 = CARTESIAN_POINT ( 'NONE',  ( -109.6228709571500701, -23.73907113216991860, -1.053371485793223261 ) ) ;
#30933 = DIRECTION ( 'NONE',  ( 0.000000000000000000, 0.000000000000000000, 1.000000000000000000 ) ) ;
#30934 = CARTESIAN_POINT ( 'NONE',  ( -38.62892889660167839, -24.51419770103157703, 9.386484678747176957 ) ) ;
#30935 = AXIS2_PLACEMENT_3D ( 'NONE', #56194, #4397, #65322 ) ;
#30936 = CARTESIAN_POINT ( 'NONE',  ( -49.52287095715006160, -23.48783264082477018, -1.443836473390095465 ) ) ;
#30937 = FACE_OUTER_BOUND ( 'NONE', #54381, .T. ) ;
#30938 = EDGE_CURVE ( 'NONE', #50597, #18000, #48817, .T. ) ;
#30939 = CARTESIAN_POINT ( 'NONE',  ( -111.6228709571500843, -23.47596703998600631, 11.44779298504227860 ) ) ;
#30940 = VERTEX_POINT ( 'NONE', #64125 ) ;
#30941 = CARTESIAN_POINT ( 'NONE',  ( 15.88337727998148985, 12.78846505907953279, 11.49999999999998934 ) ) ;
#30942 = ORIENTED_EDGE ( 'NONE', *, *, #11628, .T. ) ;
#30943 = B_SPLINE_CURVE_WITH_KNOTS ( 'NONE', 3,
 ( #60792, #16588, #2388, #38934 ),
 .UNSPECIFIED., .F., .F.,
 ( 4, 4 ),
 ( 0.000000000000000000, 9.999999999994735322E-05 ),
 .UNSPECIFIED. ) ;
#30944 = CARTESIAN_POINT ( 'NONE',  ( 8.272623322502495213, 21.45567517505680044, 11.49999999999998934 ) ) ;
#30945 = CARTESIAN_POINT ( 'NONE',  ( -103.6228709571500701, -23.48783264082478794, -1.443836473390062158 ) ) ;
#30946 = ORIENTED_EDGE ( 'NONE', *, *, #17382, .T. ) ;
#30947 = FACE_OUTER_BOUND ( 'NONE', #4822, .T. ) ;
#30948 = B_SPLINE_CURVE_WITH_KNOTS ( 'NONE', 3,
 ( #25945, #10222, #17839, #88350, #11222, #26456 ),
 .UNSPECIFIED., .F., .F.,
 ( 4, 2, 4 ),
 ( 6.384118678613282972E-06, 0.001386860460828377153, 0.002767336802978141025 ),
 .UNSPECIFIED. ) ;
#30949 = CARTESIAN_POINT ( 'NONE',  ( 31.93426202889373400, 0.3587747205144265483, 6.907000118922838716 ) ) ;
#30950 = CARTESIAN_POINT ( 'NONE',  ( -51.60612219431600778, -23.73791477778912196, 11.05961554403170766 ) ) ;
#30952 = ORIENTED_EDGE ( 'NONE', *, *, #32537, .F. ) ;
#30951 = CARTESIAN_POINT ( 'NONE',  ( -14.73150212448299357, 15.28860238833873808, 11.49999999999999645 ) ) ;
#30953 = VERTEX_POINT ( 'NONE', #33651 ) ;
#30954 = CARTESIAN_POINT ( 'NONE',  ( 17.16062296631688255, 14.07911611715085876, -1.500000000000002220 ) ) ;
#30955 = CARTESIAN_POINT ( 'NONE',  ( -15.40095275084150117, -13.70674696055758801, -1.500000000000002220 ) ) ;
#30956 = EDGE_CURVE ( 'NONE', #48956, #79545, #95043, .T. ) ;
#30957 = ORIENTED_EDGE ( 'NONE', *, *, #62782, .F. ) ;
#30958 = ORIENTED_EDGE ( 'NONE', *, *, #92916, .T. ) ;
#30959 = CARTESIAN_POINT ( 'NONE',  ( -109.8650282762807393, -25.27682926508576955, 5.784628013120847179 ) ) ;
#30960 = CARTESIAN_POINT ( 'NONE',  ( 22.81105451610979173, 1.682774720514426114, -18.46691820600746681 ) ) ;
#30961 = ORIENTED_EDGE ( 'NONE', *, *, #94445, .T. ) ;
#30962 = CARTESIAN_POINT ( 'NONE',  ( 1.600000000000000755, 0.000000000000000000, 0.000000000000000000 ) ) ;
#30963 = EDGE_CURVE ( 'NONE', #14386, #65949, #31219, .T. ) ;
#30964 = ORIENTED_EDGE ( 'NONE', *, *, #71946, .T. ) ;
#30965 = CARTESIAN_POINT ( 'NONE',  ( -121.5562042904834072, -23.47596703998600631, 11.44779298504227683 ) ) ;
#30966 = FACE_OUTER_BOUND ( 'NONE', #42957, .T. ) ;
#30967 = CARTESIAN_POINT ( 'NONE',  ( 13.71216040526616098, 15.69570726272272232, -1.500000000000002220 ) ) ;
#30968 = CARTESIAN_POINT ( 'NONE',  ( -21.33044368757495590, -4.375833669458513597, 11.49999999999999645 ) ) ;
#30969 = CARTESIAN_POINT ( 'NONE',  ( 25.82162523591733816, -4.375719933211353663, -11.31246283257596552 ) ) ;
#30970 = CARTESIAN_POINT ( 'NONE',  ( -78.60051775479411162, -23.73791477778911840, 11.05961554403170588 ) ) ;
#30971 = CARTESIAN_POINT ( 'NONE',  ( -12.88509029660790617, -18.40938060607246740, -1.500000000000002220 ) ) ;
#30972 = EDGE_CURVE ( 'NONE', #24356, #58437, #65237, .T. ) ;
#30973 = ADVANCED_FACE ( 'NONE', ( #79810 ), #81319, .T. ) ;
#30974 = CARTESIAN_POINT ( 'NONE',  ( -19.77875734969026311, -5.356774720514425603, 27.31649921512899937 ) ) ;
#30975 = ORIENTED_EDGE ( 'NONE', *, *, #54716, .F. ) ;
#30976 = DIRECTION ( 'NONE',  ( 0.000000000000000000, -7.805083003223303470E-15, 1.000000000000000000 ) ) ;
#30977 = CARTESIAN_POINT ( 'NONE',  ( 4.967622410992271753, -5.876774720514416295, 20.05703257908297843 ) ) ;
#30978 = EDGE_CURVE ( 'NONE', #49308, #23684, #49396, .T. ) ;
#30979 = ORIENTED_EDGE ( 'NONE', *, *, #98781, .T. ) ;
#30980 = ORIENTED_EDGE ( 'NONE', *, *, #90093, .F. ) ;
#30981 = AXIS2_PLACEMENT_3D ( 'NONE', #39520, #86191, #95306 ) ;
#30982 = ORIENTED_EDGE ( 'NONE', *, *, #36567, .T. ) ;
#30983 = CARTESIAN_POINT ( 'NONE',  ( -19.36244235409943926, 8.944087295975924334, -1.500000000000002220 ) ) ;
#30984 = ORIENTED_EDGE ( 'NONE', *, *, #23659, .T. ) ;
#30985 = CARTESIAN_POINT ( 'NONE',  ( -6.845587600281468177, 19.88882266644084496, 11.49999999999998934 ) ) ;
#30986 = DIRECTION ( 'NONE',  ( 1.000000000000000000, 3.773278334444167608E-23, 8.201307833595939069E-29 ) ) ;
#30987 =( BOUNDED_SURFACE ( )  B_SPLINE_SURFACE ( 3, 2, ( 
 ( #52270, #59894, #12192 ),
 ( #27930, #58887, #83200 ),
 ( #11696, #20298, #13687 ),
 ( #35051, #44657, #51270 ) ),
 .UNSPECIFIED., .F., .F., .F. ) 
 B_SPLINE_SURFACE_WITH_KNOTS ( ( 4, 4 ),
 ( 3, 3 ),
 ( 0.01105101719324316605, 0.01425305434006712488 ),
 ( 0.000000000000000000, 1.000000000000000000 ),
 .UNSPECIFIED. ) 
 GEOMETRIC_REPRESENTATION_ITEM ( )  RATIONAL_B_SPLINE_SURFACE ( (
 ( 1.000000000000000000, 0.7071067811865476838, 1.000000000000000000),
 ( 1.000000000000000000, 0.7071067811865476838, 1.000000000000000000),
 ( 1.000000000000000000, 0.7071067811865479058, 1.000000000000000000),
 ( 1.000000000000000000, 0.7071067811865479058, 1.000000000000000000) ) ) 
 REPRESENTATION_ITEM ( '' )  SURFACE ( )  );
#30988 = CARTESIAN_POINT ( 'NONE',  ( -55.52287095715008292, -23.47593901973090169, -1.443836447538997092 ) ) ;
#30989 = CARTESIAN_POINT ( 'NONE',  ( -49.41232686713205169, -25.10396340747056598, 7.262126897097727962 ) ) ;
#30990 = CARTESIAN_POINT ( 'NONE',  ( 9.413913215453616701, -19.89622248225912315, -1.500000000000002220 ) ) ;
#30991 = DIRECTION ( 'NONE',  ( 0.000000000000000000, 0.000000000000000000, 1.000000000000000000 ) ) ;
#30992 = VERTEX_POINT ( 'NONE', #17926 ) ;
#30993 = DIRECTION ( 'NONE',  ( 0.000000000000000000, -1.000000000000000000, 0.000000000000000000 ) ) ;
#30994 = EDGE_CURVE ( 'NONE', #82528, #19708, #48883, .T. ) ;
#30995 = CARTESIAN_POINT ( 'NONE',  ( -49.10457154551148307, -25.26416398485831749, 3.999772271414141489 ) ) ;
#30996 = CARTESIAN_POINT ( 'NONE',  ( -19.94048968823238255, 6.179419890754223488, 11.49999999999999645 ) ) ;
#30997 = CARTESIAN_POINT ( 'NONE',  ( 29.59866736649642860, -4.678593451839772044, 28.90589631152484174 ) ) ;
#30998 = AXIS2_PLACEMENT_3D ( 'NONE', #26911, #51752, #88820 ) ;
#30999 = CARTESIAN_POINT ( 'NONE',  ( -108.6228709571500417, -24.66019654487199730, 8.947790411086124607 ) ) ;
#31000 = CARTESIAN_POINT ( 'NONE',  ( -10.24605875044832182, -22.99950505309962523, 9.174899246800714891 ) ) ;
#31001 = CARTESIAN_POINT ( 'NONE',  ( 9.569808575145499319, 19.01914523534739132, 11.49999999999998934 ) ) ;
#31002 = CARTESIAN_POINT ( 'NONE',  ( -31.24388727629347784, -25.26956746990935443, 6.087265963545713809 ) ) ;
#31003 = CARTESIAN_POINT ( 'NONE',  ( -107.5967350901245254, -23.48786465467241413, 11.44779295918253759 ) ) ;
#31004 = EDGE_CURVE ( 'NONE', #90981, #58179, #72719, .T. ) ;
#31005 = CARTESIAN_POINT ( 'NONE',  ( -90.62287095715005592, -24.91544648472620693, 1.928969306349234802 ) ) ;
#31006 = CARTESIAN_POINT ( 'NONE',  ( -69.33027971892866503, -25.28687673834294003, 5.910757521653128066 ) ) ;
#31007 = CARTESIAN_POINT ( 'NONE',  ( 0.003324065884441271702, 22.49086686382009503, -1.500000000000002220 ) ) ;
#31008 = EDGE_CURVE ( 'NONE', #59593, #21715, #9481, .T. ) ;
#31009 = CARTESIAN_POINT ( 'NONE',  ( -108.8769404936500109, -25.25626643526282322, 3.571638612575483318 ) ) ;
#31010 = ORIENTED_EDGE ( 'NONE', *, *, #14167, .F. ) ;
#31011 = CARTESIAN_POINT ( 'NONE',  ( -49.62287095715005592, -24.64965695001467694, 8.947790433994185832 ) ) ;
#31012 = CARTESIAN_POINT ( 'NONE',  ( 9.307004028210867475, 17.29072351678862418, 11.49999999999999645 ) ) ;
#31013 = DIRECTION ( 'NONE',  ( 3.773278334444166432E-23, -1.000000000000000000, 0.000000000000000000 ) ) ;
#31014 = LINE ( 'NONE', #61981, #12335 ) ;
#31015 = ORIENTED_EDGE ( 'NONE', *, *, #84916, .F. ) ;
#31016 = EDGE_CURVE ( 'NONE', #54879, #7016, #73641, .T. ) ;
#31017 = CARTESIAN_POINT ( 'NONE',  ( -69.84206102715404541, -25.30531021297771233, 4.913976341363863298 ) ) ;
#31018 = CARTESIAN_POINT ( 'NONE',  ( -95.52287095715006160, -29.50250786944525672, 11.44777988621623166 ) ) ;
#31019 = CARTESIAN_POINT ( 'NONE',  ( -88.86938553902136562, -25.32379766982192493, 4.367815445636562544 ) ) ;
#31020 = ADVANCED_FACE ( 'NONE', ( #58498 ), #89433, .F. ) ;
#31021 = CARTESIAN_POINT ( 'NONE',  ( 16.04393857186779115, -11.51807295290239885, 11.49999999999998934 ) ) ;
#31022 = EDGE_CURVE ( 'NONE', #16401, #78060, #28034, .T. ) ;
#31023 = VERTEX_POINT ( 'NONE', #91413 ) ;
#31024 = CARTESIAN_POINT ( 'NONE',  ( -120.5228709571499905, -24.15516710230294706, 10.28746687063725496 ) ) ;
#31025 = VECTOR ( 'NONE', #27138, 1000.000000000000114 ) ;
#31026 = PERSON_AND_ORGANIZATION_ROLE ( 'creator' ) ;
#31027 = ORIENTED_EDGE ( 'NONE', *, *, #82755, .F. ) ;
#31028 = LINE ( 'NONE', #92921, #64579 ) ;
#31029 = CARTESIAN_POINT ( 'NONE',  ( -48.62287095715006302, -24.50321055353803601, 9.387540953477527594 ) ) ;
#31030 = CARTESIAN_POINT ( 'NONE',  ( -55.47781443094807230, -25.00158670708910336, 2.256160236439221034 ) ) ;
#31031 = CARTESIAN_POINT ( 'NONE',  ( -99.20586904084365187, -25.03145057151672148, 7.003177191084415831 ) ) ;
#31032 = DIRECTION ( 'NONE',  ( -3.773278334444167608E-23, 1.000000000000000000, 0.000000000000000000 ) ) ;
#31033 = CARTESIAN_POINT ( 'NONE',  ( -56.55620429048340014, -24.65952944569304606, 1.056160979905696129 ) ) ;
#31034 = CARTESIAN_POINT ( 'NONE',  ( -13.89275734969026388, -0.3587747205144262708, 31.02402280011862246 ) ) ;
#31035 = CARTESIAN_POINT ( 'NONE',  ( -12.72357806474857966, 15.40231687525621318, -1.500000000000002220 ) ) ;
#31036 = DIRECTION ( 'NONE',  ( -3.469446951953614189E-15, 1.000000000000000000, 0.000000000000000000 ) ) ;
#31037 = CARTESIAN_POINT ( 'NONE',  ( 30.93860345374796594, -0.6647747205144265426, 28.83647319851474933 ) ) ;
#31038 = ORIENTED_EDGE ( 'NONE', *, *, #53564, .T. ) ;
#31039 = CARTESIAN_POINT ( 'NONE',  ( -79.59586937953757513, -23.96169478059713143, 10.65365249895718058 ) ) ;
#31040 = CARTESIAN_POINT ( 'NONE',  ( -109.5745106736623029, -25.18430227007843669, 3.630693441492102824 ) ) ;
#31041 = CARTESIAN_POINT ( 'NONE',  ( -35.66629527092394625, -23.85016227208580730, -0.8807180028928173199 ) ) ;
#31042 = LINE ( 'NONE', #78702, #32183 ) ;
#31043 = VECTOR ( 'NONE', #11069, 1000.000000000000000 ) ;
#31044 = CYLINDRICAL_SURFACE ( 'NONE', #49659, 1.000000000000000000 ) ;
#31045 = DIRECTION ( 'NONE',  ( -0.000000000000000000, 1.000000000000000000, -0.000000000000000000 ) ) ;
#31046 = LINE ( 'NONE', #71127, #9052 ) ;
#31047 = PLANE ( 'NONE',  #40440 ) ;
#31048 = VERTEX_POINT ( 'NONE', #90426 ) ;
#31049 = CARTESIAN_POINT ( 'NONE',  ( 0.8729654516333695824, -20.24016528753796962, 11.49999999999998934 ) ) ;
#31050 = CARTESIAN_POINT ( 'NONE',  ( -109.5895376238167103, -23.48783264082478794, -1.443836473390060382 ) ) ;
#31051 = CARTESIAN_POINT ( 'NONE',  ( -99.62287095715005592, -23.47593901973091235, -1.443836447539001089 ) ) ;
#31052 = ORIENTED_EDGE ( 'NONE', *, *, #77510, .F. ) ;
#31053 = CARTESIAN_POINT ( 'NONE',  ( -24.57525087998973845, -6.376774720514426953, -15.45548830044933197 ) ) ;
#31054 = VECTOR ( 'NONE', #14293, 1000.000000000000227 ) ;
#31055 = CARTESIAN_POINT ( 'NONE',  ( 20.09017895974002599, 0.4902201509063087159, -1.500000000000002220 ) ) ;
#31056 = CARTESIAN_POINT ( 'NONE',  ( -1.999300432013352058, 20.99099883833691749, 11.49999999999999645 ) ) ;
#31057 = AXIS2_PLACEMENT_3D ( 'NONE', #2652, #94981, #62542 ) ;
#31058 = CARTESIAN_POINT ( 'NONE',  ( 22.05266032001784637, -1.487345182339283367, -1.500000000000002220 ) ) ;
#31059 = CARTESIAN_POINT ( 'NONE',  ( -13.21525772315781388, 15.71049578022273785, -1.500000000000002220 ) ) ;
#31060 = CARTESIAN_POINT ( 'NONE',  ( -122.5228709571500616, -24.66019654487200441, 8.947790411086112172 ) ) ;
#31061 = EDGE_CURVE ( 'NONE', #31540, #44951, #89303, .T. ) ;
#31062 = B_SPLINE_CURVE_WITH_KNOTS ( 'NONE', 3,
 ( #29310, #21681, #23183, #8477 ),
 .UNSPECIFIED., .F., .F.,
 ( 4, 4 ),
 ( 0.9611863596518752662, 0.9701927909239907999 ),
 .UNSPECIFIED. ) ;
#31063 = CARTESIAN_POINT ( 'NONE',  ( 16.09828331921172051, 3.622774695106080411, -27.82448843548682049 ) ) ;
#31064 = ORIENTED_EDGE ( 'NONE', *, *, #66974, .F. ) ;
#31065 = PLANE ( 'NONE',  #94645 ) ;
#31066 = ORIENTED_EDGE ( 'NONE', *, *, #57867, .F. ) ;
#31067 = CARTESIAN_POINT ( 'NONE',  ( -6.728471858368818559, -6.376774720514408301, 19.14926908420045137 ) ) ;
#31068 = CARTESIAN_POINT ( 'NONE',  ( -64.62287095715005592, -24.64965695001468404, 8.947790433994185832 ) ) ;
#31069 = VERTEX_POINT ( 'NONE', #43268 ) ;
#31070 = VERTEX_POINT ( 'NONE', #68098 ) ;
#31071 = ORIENTED_EDGE ( 'NONE', *, *, #56157, .F. ) ;
#31072 = DIRECTION ( 'NONE',  ( -1.000000000000000000, -0.000000000000000000, -7.994117400814786717E-16 ) ) ;
#31073 = DIRECTION ( 'NONE',  ( -0.8788171126619707119, 0.4771587602595986910, -0.000000000000000000 ) ) ;
#31074 = CARTESIAN_POINT ( 'NONE',  ( -77.58953762381672448, -24.65952944569304606, 1.056160979905698794 ) ) ;
#31075 = CARTESIAN_POINT ( 'NONE',  ( 1.453578435135240321, -20.60874541997745268, -1.500000000000002220 ) ) ;
#31076 = CARTESIAN_POINT ( 'NONE',  ( 17.73057777116804701, 12.32922261165129285, 11.49999999999999645 ) ) ;
#31077 = ORIENTED_EDGE ( 'NONE', *, *, #100121, .F. ) ;
#31078 = EDGE_CURVE ( 'NONE', #55585, #89617, #59101, .T. ) ;
#31079 = FACE_OUTER_BOUND ( 'NONE', #66083, .T. ) ;
#31080 = CARTESIAN_POINT ( 'NONE',  ( -60.62287095715006302, -24.51163499207174468, 0.6490370598554270343 ) ) ;
#31081 = CARTESIAN_POINT ( 'NONE',  ( -21.16225983376422448, 7.283793490815352989, 11.49999999999998934 ) ) ;
#31082 = EDGE_CURVE ( 'NONE', #89004, #17644, #37354, .T. ) ;
#31083 = EDGE_CURVE ( 'NONE', #84745, #11381, #96643, .T. ) ;
#31084 = CARTESIAN_POINT ( 'NONE',  ( -79.36551648466291908, -25.12205614543422172, 6.194054221785125769 ) ) ;
#31085 = CARTESIAN_POINT ( 'NONE',  ( -53.52287095715009002, -24.33832256527048088, 0.1851278514138568754 ) ) ;
#31086 = VERTEX_POINT ( 'NONE', #14287 ) ;
#31087 = FACE_OUTER_BOUND ( 'NONE', #21675, .T. ) ;
#31088 = CARTESIAN_POINT ( 'NONE',  ( -49.48966588299922620, -24.51419770103158413, 9.386484678747189392 ) ) ;
#31089 = EDGE_CURVE ( 'NONE', #75416, #13388, #55500, .T. ) ;
#31090 = CARTESIAN_POINT ( 'NONE',  ( -115.5228709571501042, -23.84047902841602351, -0.8780736468305720965 ) ) ;
#31091 = CARTESIAN_POINT ( 'NONE',  ( 17.12911088700535700, -11.98135219954639830, 11.49999999999998934 ) ) ;
#31092 = ORIENTED_EDGE ( 'NONE', *, *, #10077, .T. ) ;
#31093 = FACE_OUTER_BOUND ( 'NONE', #67074, .T. ) ;
#31094 = VERTEX_POINT ( 'NONE', #44761 ) ;
#31095 = B_SPLINE_CURVE_WITH_KNOTS ( 'NONE', 3,
 ( #41354, #87021, #33742, #18011 ),
 .UNSPECIFIED., .F., .F.,
 ( 4, 4 ),
 ( 0.000000000000000000, 9.999999999998897304E-05 ),
 .UNSPECIFIED. ) ;
#31096 = AXIS2_PLACEMENT_3D ( 'NONE', #28761, #52104, #83030 ) ;
#31097 = CARTESIAN_POINT ( 'NONE',  ( -109.5922553255047660, -23.96169478059713853, 10.65365249895717703 ) ) ;
#31098 = CARTESIAN_POINT ( 'NONE',  ( -18.51692787870624102, -10.26217664800131502, -1.500000000000002220 ) ) ;
#31099 = ORIENTED_EDGE ( 'NONE', *, *, #78848, .F. ) ;
#31100 = LINE ( 'NONE', #69677, #25166 ) ;
#31101 = CARTESIAN_POINT ( 'NONE',  ( -21.76810506448615712, 0.6044244127108716613, -1.500000000000002220 ) ) ;
#31102 = PLANE ( 'NONE',  #70806 ) ;
#31103 = DIRECTION ( 'NONE',  ( 0.000000000000000000, 1.000000000000000000, 0.000000000000000000 ) ) ;
#31104 = LINE ( 'NONE', #60087, #62732 ) ;
#31105 = CARTESIAN_POINT ( 'NONE',  ( 6.392671032147439369, 20.83241601264130693, -1.500000000000002220 ) ) ;
#31106 = CARTESIAN_POINT ( 'NONE',  ( -95.52287095715013265, -24.83602698348160231, 1.605859176311266179 ) ) ;
#31107 = EDGE_LOOP ( 'NONE', ( #1651, #53785, #91155, #16562 ) ) ;
#31108 = DIRECTION ( 'NONE',  ( 0.000000000000000000, -2.173523156925979552E-06, 0.9999999999976378895 ) ) ;
#31109 = CARTESIAN_POINT ( 'NONE',  ( 8.349999999999972999, 27.69999999999999574, 0.000000000000000000 ) ) ;
#31110 = EDGE_CURVE ( 'NONE', #19391, #60254, #27541, .T. ) ;
#31111 = ORIENTED_EDGE ( 'NONE', *, *, #33058, .T. ) ;
#31112 = ORIENTED_EDGE ( 'NONE', *, *, #40039, .F. ) ;
#31113 = ADVANCED_FACE ( 'NONE', ( #16175 ), #957, .F. ) ;
#31114 = VERTEX_POINT ( 'NONE', #60987 ) ;
#31115 = CARTESIAN_POINT ( 'NONE',  ( -72.52287095715007581, -29.50247984919015209, -1.443849546365055359 ) ) ;
#31116 = CARTESIAN_POINT ( 'NONE',  ( -44.62287095715004881, -24.64898659630528854, 1.056161002820819261 ) ) ;
#31117 = CARTESIAN_POINT ( 'NONE',  ( 21.17954554857512761, 0.9134790845329443520, 11.49999999999998934 ) ) ;
#31118 = VECTOR ( 'NONE', #9198, 1000.000000000000000 ) ;
#31119 = CARTESIAN_POINT ( 'NONE',  ( -121.6228709571500417, -23.72747288104441665, -1.053458166803660445 ) ) ;
#31120 = CARTESIAN_POINT ( 'NONE',  ( -79.88583274576632220, -25.03138275433761706, 7.452192808739267704 ) ) ;
#31121 = EDGE_CURVE ( 'NONE', #53265, #81299, #18023, .T. ) ;
#31122 = CARTESIAN_POINT ( 'NONE',  ( 21.48910942911434319, -4.361838973203037817, -16.63132305728401050 ) ) ;
#31123 = DIRECTION ( 'NONE',  ( 1.000000000000000000, 0.000000000000000000, -0.000000000000000000 ) ) ;
#31124 = CARTESIAN_POINT ( 'NONE',  ( 19.05472526407214673, 3.605321472892077050, 11.49999999999998934 ) ) ;
#31125 = CARTESIAN_POINT ( 'NONE',  ( -51.92991042017824554, -25.26556399697136968, 6.106724579306912482 ) ) ;
#31126 = ORIENTED_EDGE ( 'NONE', *, *, #45417, .T. ) ;
#31127 = CARTESIAN_POINT ( 'NONE',  ( 7.440116899146960172, 17.95454168335740874, 11.49999999999999645 ) ) ;
#31128 = CARTESIAN_POINT ( 'NONE',  ( -126.5228709571500616, -23.47596703998600631, 11.44779298504227683 ) ) ;
#31129 = CARTESIAN_POINT ( 'NONE',  ( 10.54059822343757880, -6.376774720514426953, 23.12308057603841149 ) ) ;
#31130 = ORIENTED_EDGE ( 'NONE', *, *, #80690, .T. ) ;
#31131 = EDGE_CURVE ( 'NONE', #69074, #9599, #8573, .T. ) ;
#31132 = CARTESIAN_POINT ( 'NONE',  ( 2.790451961050095520, -5.876774720514409189, 18.85195250256714417 ) ) ;
#31133 = CARTESIAN_POINT ( 'NONE',  ( -70.66311671602751687, -25.30500184331102886, 4.882606927408491337 ) ) ;
#31135 = ADVANCED_FACE ( 'NONE', ( #91918 ), #22391, .F. ) ;
#31134 = CARTESIAN_POINT ( 'NONE',  ( -64.62287095715011276, -23.94994826722565762, -0.6494450866342728057 ) ) ;
#31136 = B_SPLINE_CURVE_WITH_KNOTS ( 'NONE', 3,
 ( #95193, #3366, #50518, #26686 ),
 .UNSPECIFIED., .F., .F.,
 ( 4, 4 ),
 ( 0.000000000000000000, 9.999999999998897304E-05 ),
 .UNSPECIFIED. ) ;
#31137 = VECTOR ( 'NONE', #51613, 1000.000000000000114 ) ;
#31138 = CARTESIAN_POINT ( 'NONE',  ( -55.62287095715004881, -23.48783264082478084, -1.443836473390068820 ) ) ;
#31139 = CARTESIAN_POINT ( 'NONE',  ( -3.832734262880480358, 19.25313627021017382, -1.500000000000002220 ) ) ;
#31140 = CARTESIAN_POINT ( 'NONE',  ( -35.62287095715005592, -29.50248789122583659, 2.256150453626215580 ) ) ;
#31142 = ORIENTED_EDGE ( 'NONE', *, *, #7060, .F. ) ;
#31141 = APPROVAL_PERSON_ORGANIZATION ( #92546, #28322, #54006 ) ;
#31143 = CARTESIAN_POINT ( 'NONE',  ( 17.73057777116804701, 12.32922261165129285, 11.49999999999998934 ) ) ;
#31144 = CARTESIAN_POINT ( 'NONE',  ( -13.57581083383197296, -5.876774720514426953, 19.78786796564403616 ) ) ;
#31145 = LINE ( 'NONE', #61116, #36154 ) ;
#31146 = EDGE_CURVE ( 'NONE', #43589, #48508, #10564, .T. ) ;
#31147 = DIRECTION ( 'NONE',  ( 0.000000000000000000, 0.000000000000000000, 1.000000000000000000 ) ) ;
#31148 = CARTESIAN_POINT ( 'NONE',  ( -14.43837761634077310, -17.93274050997184332, -1.500000000000002220 ) ) ;
#31149 = PERSON_AND_ORGANIZATION ( #70597, #27821 ) ;
#31150 = CARTESIAN_POINT ( 'NONE',  ( -93.55196295890371516, -24.15543982623907837, -0.2315651400026621232 ) ) ;
#31151 = CARTESIAN_POINT ( 'NONE',  ( 3.902919446070569176, -6.376774720514427841, 21.47497695444087284 ) ) ;
#31152 = CARTESIAN_POINT ( 'NONE',  ( -121.5556932203309799, -23.96169478059713853, 10.65365249895717525 ) ) ;
#31153 = DIRECTION ( 'NONE',  ( 1.000000000000000000, -0.000000000000000000, -0.000000000000000000 ) ) ;
#31154 = CARTESIAN_POINT ( 'NONE',  ( -111.6050501299251323, -25.29823978627861791, 3.602891629172883636 ) ) ;
#31155 = CARTESIAN_POINT ( 'NONE',  ( -63.62287095715004881, -24.64965695001468404, 8.947790433994185832 ) ) ;
#31156 = DIRECTION ( 'NONE',  ( 1.000000000000000000, -4.218088402344531063E-15, 0.000000000000000000 ) ) ;
#31157 = CARTESIAN_POINT ( 'NONE',  ( 11.60740158406642664, -16.16820694497113564, 11.49999999999998934 ) ) ;
#31158 = CARTESIAN_POINT ( 'NONE',  ( -27.96875734969026084, 3.316774720514426456, 23.50402280011861933 ) ) ;
#31159 = CARTESIAN_POINT ( 'NONE',  ( 3.337697395173636394, -19.57427954046807983, -1.500000000000002220 ) ) ;
#31160 = CARTESIAN_POINT ( 'NONE',  ( 0.3670296583442628213, -5.876774720514417183, 20.26087634804755311 ) ) ;
#31161 = DIRECTION ( 'NONE',  ( -3.773278334453079618E-23, 0.9999999999976377785, 2.173523156925979975E-06 ) ) ;
#31162 = DIRECTION ( 'NONE',  ( -0.8246584009594636333, -1.974890369949422540E-15, 0.5656310827093757876 ) ) ;
#31163 = CARTESIAN_POINT ( 'NONE',  ( 6.562613027033147084, 19.67253995144353240, 11.49999999999999645 ) ) ;
#31164 = DIRECTION ( 'NONE',  ( 1.000000000000000000, 3.773278334444167608E-23, 8.201307833595939069E-29 ) ) ;
#31165 = CARTESIAN_POINT ( 'NONE',  ( -4.621320343559254695, 11.49999999999999467, 2.100000000000000089 ) ) ;
#31166 = CARTESIAN_POINT ( 'NONE',  ( 6.135622925040504327, -21.92205258971886650, 11.49999999999999645 ) ) ;
#31167 = VECTOR ( 'NONE', #55367, 1000.000000000000000 ) ;
#31168 = ORIENTED_EDGE ( 'NONE', *, *, #31661, .F. ) ;
#31169 = CARTESIAN_POINT ( 'NONE',  ( -83.62287095715009855, -23.73934037231757443, 11.05740245334328975 ) ) ;
#31170 = B_SPLINE_CURVE_WITH_KNOTS ( 'NONE', 3,
 ( #65602, #3685, #3195, #20379, #50360, #89412, #97021, #66105 ),
 .UNSPECIFIED., .F., .F.,
 ( 4, 2, 2, 4 ),
 ( -0.001224873891641420440, -0.0002244903592271052430, 0.0007758931731872099544, 0.002776660238015836880 ),
 .UNSPECIFIED. ) ;
#31171 = CARTESIAN_POINT ( 'NONE',  ( -92.52287095715006160, -24.64965694238407323, 8.947790433994196491 ) ) ;
#31172 = ORIENTED_EDGE ( 'NONE', *, *, #54568, .T. ) ;
#31173 = CARTESIAN_POINT ( 'NONE',  ( 19.91930514195032487, 3.327535025408205893, 11.49999999999998934 ) ) ;
#31174 = CARTESIAN_POINT ( 'NONE',  ( -108.6228709571500417, -24.50321055353805022, 9.387540953477527594 ) ) ;
#31175 = DIRECTION ( 'NONE',  ( 0.000000000000000000, 2.173523156925980399E-06, -0.9999999999976378895 ) ) ;
#31176 = ORIENTED_EDGE ( 'NONE', *, *, #52088, .T. ) ;
#31177 = ORIENTED_EDGE ( 'NONE', *, *, #97955, .T. ) ;
#31178 = CARTESIAN_POINT ( 'NONE',  ( 282.9764569301858046, 6.376774720514426953, 20.79159422840526616 ) ) ;
#31179 = CARTESIAN_POINT ( 'NONE',  ( 6.305670413343573699, 22.00876638805999974, 11.49999999999998934 ) ) ;
#31180 = CARTESIAN_POINT ( 'NONE',  ( -41.57697449856503624, -25.20347274299025031, 3.352851794561174437 ) ) ;
#31181 = CARTESIAN_POINT ( 'NONE',  ( -19.28869470675124731, 9.786980993800005635, -1.500000000000002220 ) ) ;
#31182 = CARTESIAN_POINT ( 'NONE',  ( -123.5542534380672919, -24.51314013834318217, 0.6176544820404261671 ) ) ;
#31183 = VECTOR ( 'NONE', #28414, 1000.000000000000114 ) ;
#31184 = CARTESIAN_POINT ( 'NONE',  ( -19.94816486946033507, 6.322790147265108018, 11.49999999999999645 ) ) ;
#31185 = ORIENTED_EDGE ( 'NONE', *, *, #9377, .F. ) ;
#31186 = CARTESIAN_POINT ( 'NONE',  ( -69.53040046975404209, -25.31612467077423290, 5.066170237949151556 ) ) ;
#31187 = CARTESIAN_POINT ( 'NONE',  ( -20.26759042640731323, -8.618136523154847239, -1.500000000000002220 ) ) ;
#31188 = DIRECTION ( 'NONE',  ( 0.000000000000000000, -1.000000000000000000, 0.000000000000000000 ) ) ;
#31189 = DIRECTION ( 'NONE',  ( 1.000000000000000000, 0.000000000000000000, 0.000000000000000000 ) ) ;
#31190 = VERTEX_POINT ( 'NONE', #41030 ) ;
#31191 = CARTESIAN_POINT ( 'NONE',  ( 4.468667172983064262, -6.376774720514401196, 18.40700896291420463 ) ) ;
#31192 = LINE ( 'NONE', #24080, #54307 ) ;
#31193 = ORIENTED_EDGE ( 'NONE', *, *, #29975, .T. ) ;
#31194 = CARTESIAN_POINT ( 'NONE',  ( 22.81105451610979173, 1.477225279485574028, -18.46691820600746681 ) ) ;
#31195 = EDGE_CURVE ( 'NONE', #99951, #44074, #32488, .T. ) ;
#31196 = EDGE_LOOP ( 'NONE', ( #84144, #3319, #79414, #13780 ) ) ;
#31197 = EDGE_CURVE ( 'NONE', #73248, #27537, #9066, .T. ) ;
#31198 = EDGE_LOOP ( 'NONE', ( #30980, #41449, #60397, #4998 ) ) ;
#31199 = CARTESIAN_POINT ( 'NONE',  ( -41.55620429048339304, -24.64965694238574656, 8.947790433994205372 ) ) ;
#31200 = CARTESIAN_POINT ( 'NONE',  ( -101.7007079832508367, -25.27404824587932097, 3.725872426325841147 ) ) ;
#31201 = CARTESIAN_POINT ( 'NONE',  ( -4.635780534842457001, -5.876774720514410077, 19.53657742262743113 ) ) ;
#31202 = CARTESIAN_POINT ( 'NONE',  ( -4.302178748239556150, -20.00421716419250373, -1.500000000000002220 ) ) ;
#31203 = ADVANCED_FACE ( 'NONE', ( #86688 ), #78058, .T. ) ;
#31204 = ORIENTED_EDGE ( 'NONE', *, *, #47186, .T. ) ;
#31205 = DIRECTION ( 'NONE',  ( -0.000000000000000000, 1.000000000000000000, -0.000000000000000000 ) ) ;
#31206 = CARTESIAN_POINT ( 'NONE',  ( -33.62287095715005592, -23.48786465467240347, 11.44779295918255535 ) ) ;
#31207 = DIRECTION ( 'NONE',  ( -3.773278334453079618E-23, 0.9999999999976377785, 2.173523156925979975E-06 ) ) ;
#31208 = CARTESIAN_POINT ( 'NONE',  ( 20.12748746789148413, 9.599020362109589755, 11.49999999999998934 ) ) ;
#31209 = EDGE_CURVE ( 'NONE', #90352, #45280, #17175, .T. ) ;
#31211 = LINE ( 'NONE', #46446, #80465 ) ;
#31210 = AXIS2_PLACEMENT_3D ( 'NONE', #92649, #45504, #93146 ) ;
#31212 = FACE_OUTER_BOUND ( 'NONE', #27970, .T. ) ;
#31213 = ORIENTED_EDGE ( 'NONE', *, *, #95650, .F. ) ;
#31214 = B_SPLINE_CURVE_WITH_KNOTS ( 'NONE', 3,
 ( #89097, #26698, #34810, #57658, #57167, #49049 ),
 .UNSPECIFIED., .F., .F.,
 ( 4, 2, 4 ),
 ( 0.000000000000000000, 0.001380901958385397869, 0.002761803916770795737 ),
 .UNSPECIFIED. ) ;
#31215 = DIRECTION ( 'NONE',  ( 0.000000000000000000, -1.478457507934778393E-16, -1.000000000000000000 ) ) ;
#31216 = CARTESIAN_POINT ( 'NONE',  ( -29.39543059329891506, -24.63645834301326332, 7.191773098902599415 ) ) ;
#31217 = LOCAL_TIME ( 0, 54, 15.00000000000000000, #78686 ) ;
#31218 = CARTESIAN_POINT ( 'NONE',  ( 0.5783248939474509021, 20.82821387695577187, 11.49999999999998934 ) ) ;
#31219 = B_SPLINE_CURVE_WITH_KNOTS ( 'NONE', 3,
 ( #87936, #58005, #56504, #42289, #97042, #2213, #25534, #64630 ),
 .UNSPECIFIED., .F., .F.,
 ( 4, 2, 2, 4 ),
 ( 6.384118678613149141E-06, 0.002007151183507258855, 0.003007534715921581642, 0.004007918248335903995 ),
 .UNSPECIFIED. ) ;
#31220 = ORIENTED_EDGE ( 'NONE', *, *, #71850, .T. ) ;
#31222 = VERTEX_POINT ( 'NONE', #2465 ) ;
#31221 = CARTESIAN_POINT ( 'NONE',  ( 3.787259615384621636, -6.376774720514404748, 18.51923076923076650 ) ) ;
#31223 = AXIS2_PLACEMENT_3D ( 'NONE', #67001, #22279, #48154 ) ;
#31225 = EDGE_CURVE ( 'NONE', #58528, #20674, #63382, .T. ) ;
#31224 = FACE_OUTER_BOUND ( 'NONE', #22859, .T. ) ;
#31226 = CARTESIAN_POINT ( 'NONE',  ( 16.30764028314251846, 13.22082560946828522, -1.500000000000002220 ) ) ;
#31227 = ORIENTED_EDGE ( 'NONE', *, *, #62556, .T. ) ;
#31228 = CARTESIAN_POINT ( 'NONE',  ( -37.62287095715005592, -24.64965695001467694, 8.947790433994187609 ) ) ;
#31229 = DIRECTION ( 'NONE',  ( 1.000000000000000000, -0.000000000000000000, -0.000000000000000000 ) ) ;
#31230 = CARTESIAN_POINT ( 'NONE',  ( 8.583179188118256420, -5.356774720514425603, -25.03641645905366886 ) ) ;
#31231 = VECTOR ( 'NONE', #56226, 1000.000000000000000 ) ;
#31232 = CARTESIAN_POINT ( 'NONE',  ( 27.53860345374784657, 4.772774720514425972, -8.321925749325748356 ) ) ;
#31233 = CARTESIAN_POINT ( 'NONE',  ( -20.27875734969026311, -6.376774720514428729, 24.00402280011862288 ) ) ;
#31234 = CARTESIAN_POINT ( 'NONE',  ( -79.62287095715005592, -23.47593901973091235, -1.443836447539004642 ) ) ;
#31236 = ORIENTED_EDGE ( 'NONE', *, *, #53424, .F. ) ;
#31235 = CARTESIAN_POINT ( 'NONE',  ( -0.8134642310582372859, 22.17477653155656725, 11.49999999999999645 ) ) ;
#31237 = CARTESIAN_POINT ( 'NONE',  ( -38.52287095715008292, -23.48783264083452593, -1.443836473374935592 ) ) ;
#31238 = CARTESIAN_POINT ( 'NONE',  ( -74.52287095715007581, -23.47596703998600631, 11.44779298504228748 ) ) ;
#31239 = ORIENTED_EDGE ( 'NONE', *, *, #34911, .F. ) ;
#31240 = CARTESIAN_POINT ( 'NONE',  ( 22.15051849217804403, -4.756829024181505439, 11.49999999999998934 ) ) ;
#31242 = ORIENTED_EDGE ( 'NONE', *, *, #81684, .F. ) ;
#31241 = FACE_OUTER_BOUND ( 'NONE', #31960, .T. ) ;
#31243 = VERTEX_POINT ( 'NONE', #70472 ) ;
#31244 = CARTESIAN_POINT ( 'NONE',  ( -113.2228709571500644, -23.47596703998600631, 11.44779298504227860 ) ) ;
#31245 = AXIS2_PLACEMENT_3D ( 'NONE', #38622, #54363, #61477 ) ;
#31246 = CARTESIAN_POINT ( 'NONE',  ( -15.35229381799144299, -13.07563953244551591, 11.49999999999998934 ) ) ;
#31247 = CARTESIAN_POINT ( 'NONE',  ( -81.62287095715005592, -24.35013146730203459, 9.818937971375111928 ) ) ;
#31248 = VERTEX_POINT ( 'NONE', #31909 ) ;
#31249 = CARTESIAN_POINT ( 'NONE',  ( -94.62287095715005592, -29.50250243563736774, 8.947779886222139822 ) ) ;
#31250 = CARTESIAN_POINT ( 'NONE',  ( -19.39139147909919458, -11.06001032434818576, -1.500000000000002220 ) ) ;
#31251 = EDGE_LOOP ( 'NONE', ( #65998, #96728, #49090, #22694 ) ) ;
#31252 = ORIENTED_EDGE ( 'NONE', *, *, #80822, .F. ) ;
#31253 = CARTESIAN_POINT ( 'NONE',  ( -101.4413695709857990, -25.25341166521219805, 6.524206359329101090 ) ) ;
#31255 = CARTESIAN_POINT ( 'NONE',  ( -69.34303308397305443, -25.24554880456021522, 6.209207408033732278 ) ) ;
#31254 = AXIS2_PLACEMENT_3D ( 'NONE', #91874, #75152, #22345 ) ;
#31256 = DIRECTION ( 'NONE',  ( 1.000000000000000000, -0.000000000000000000, 0.000000000000000000 ) ) ;
#31257 = CARTESIAN_POINT ( 'NONE',  ( 3.509873074917118085, 0.3587747205144265483, 29.15869884040363758 ) ) ;
#31259 = ADVANCED_FACE ( 'NONE', ( #18180 ), #56268, .T. ) ;
#31258 = CARTESIAN_POINT ( 'NONE',  ( -30.62207085380013183, -24.04615231314291179, -0.4716817114508918829 ) ) ;
#31260 = CARTESIAN_POINT ( 'NONE',  ( 10.86043079284791091, -16.25897383129715834, 11.49999999999998934 ) ) ;
#31261 = AXIS2_PLACEMENT_3D ( 'NONE', #23397, #54383, #2607 ) ;
#31262 = LINE ( 'NONE', #16030, #86298 ) ;
#31263 = CARTESIAN_POINT ( 'NONE',  ( 20.96596170256846747, -4.772324250704091497, 11.49999999999998934 ) ) ;
#31264 = CARTESIAN_POINT ( 'NONE',  ( -128.5222656252491902, -23.48783264082478794, -1.443836473390056829 ) ) ;
#31265 = CARTESIAN_POINT ( 'NONE',  ( -51.52287095715006870, -24.65952944569304606, 1.056160979905693686 ) ) ;
#31266 = CARTESIAN_POINT ( 'NONE',  ( -71.55620429048337883, -23.48786465467241058, 11.44779295918254292 ) ) ;
#31267 = EDGE_CURVE ( 'NONE', #14750, #34120, #24294, .T. ) ;
#31268 = CARTESIAN_POINT ( 'NONE',  ( -80.62287095715007013, -23.47596703998600631, 11.44779298504227860 ) ) ;
#31269 = CARTESIAN_POINT ( 'NONE',  ( 15.09361930729867574, -17.17024899132524496, -1.500000000000002220 ) ) ;
#31270 = APPROVAL_ROLE ( '' ) ;
#31271 = CARTESIAN_POINT ( 'NONE',  ( -96.51331733479386799, -24.15620529776628445, 10.23563542870660115 ) ) ;
#31272 = CARTESIAN_POINT ( 'NONE',  ( -53.65874886358959373, -23.48783264082475952, -1.443836473390095909 ) ) ;
#31273 = CARTESIAN_POINT ( 'NONE',  ( 1.468936567494551593, -19.95401460376903913, 11.49999999999999645 ) ) ;
#31274 = FACE_OUTER_BOUND ( 'NONE', #31107, .T. ) ;
#31275 = DIRECTION ( 'NONE',  ( -3.773278334444166432E-23, 1.000000000000000000, 0.000000000000000000 ) ) ;
#31276 = CARTESIAN_POINT ( 'NONE',  ( 4.263585034174699473, -5.876774720514402972, 18.26968045024142739 ) ) ;
#31277 = DIRECTION ( 'NONE',  ( 0.000000000000000000, -1.571307496355802709E-16, -1.000000000000000000 ) ) ;
#31278 = VERTEX_POINT ( 'NONE', #48654 ) ;
#31279 = DIRECTION ( 'NONE',  ( 0.000000000000000000, 0.000000000000000000, -1.000000000000000000 ) ) ;
#31280 = CARTESIAN_POINT ( 'NONE',  ( -97.62287095715005592, -29.50250243563736774, 8.947779886222138046 ) ) ;
#31281 = CARTESIAN_POINT ( 'NONE',  ( 21.72137571921558319, 1.130696696492564213, 11.49999999999998934 ) ) ;
#31282 = CARTESIAN_POINT ( 'NONE',  ( -45.52287095715007581, -24.63345952396255001, 9.038047939301508293 ) ) ;
#31283 = CARTESIAN_POINT ( 'NONE',  ( -18.74838588596843181, -5.942601993926947657, -1.500000000000002220 ) ) ;
#31284 = LINE ( 'NONE', #39401, #75033 ) ;
#31285 = AXIS2_PLACEMENT_3D ( 'NONE', #20913, #27049, #97052 ) ;
#31286 = CARTESIAN_POINT ( 'NONE',  ( -109.3602963299949806, -25.31697955520687771, 4.255031523248292480 ) ) ;
#31287 = DATE_TIME_ROLE ( 'classification_date' ) ;
#31288 = SECURITY_CLASSIFICATION ( '', '', #17062 ) ;
#31289 = CARTESIAN_POINT ( 'NONE',  ( -56.62287095715008434, -23.47596703998600276, 11.44779298504227683 ) ) ;
#31290 = CARTESIAN_POINT ( 'NONE',  ( 2.708118538500707828, -5.876774720514424288, 20.94830092343283212 ) ) ;
#31291 = CARTESIAN_POINT ( 'NONE',  ( 3.086129920417311823, 20.35385046113321295, 11.49999999999999645 ) ) ;
#31292 = CARTESIAN_POINT ( 'NONE',  ( -27.70544111104076990, -24.65058036537550024, 8.251826706788236265 ) ) ;
#31293 = CARTESIAN_POINT ( 'NONE',  ( -120.5910596545900120, -24.15503026093913874, -0.2815557561904504791 ) ) ;
#31294 = VECTOR ( 'NONE', #58119, 1000.000000000000114 ) ;
#31295 = EDGE_LOOP ( 'NONE', ( #69690, #23734, #86967, #76483, #4777, #59819 ) ) ;
#31296 = SHAPE_REPRESENTATION_RELATIONSHIP ( 'NONE' , 'NONE' ,  #22430, #48872 ) ;
#31297 = CARTESIAN_POINT ( 'NONE',  ( -46.62287095715006302, -24.34917612406838217, 0.1852690917426625117 ) ) ;
#31298 = CARTESIAN_POINT ( 'NONE',  ( -39.61224275064198963, -25.18430957889518496, 3.692191345043688511 ) ) ;
#31299 = CARTESIAN_POINT ( 'NONE',  ( -97.59977826141401636, -23.48783264082477018, -1.443836473390088360 ) ) ;
#31300 = CARTESIAN_POINT ( 'NONE',  ( 15.03705075715986972, -3.514354387074007047, -27.31754965648562816 ) ) ;
#31301 = CIRCLE ( 'NONE', #21510, 28.96799999999999642 ) ;
#31302 = B_SPLINE_CURVE_WITH_KNOTS ( 'NONE', 3,
 ( #89927, #59481, #66123, #42287, #27538, #43757 ),
 .UNSPECIFIED., .F., .F.,
 ( 4, 2, 4 ),
 ( 0.000000000000000000, 0.001380901958385396351, 0.002761803916770792702 ),
 .UNSPECIFIED. ) ;
#31303 = FACE_OUTER_BOUND ( 'NONE', #66300, .T. ) ;
#31304 = CARTESIAN_POINT ( 'NONE',  ( 3.300000000000006040, 0.000000000000000000, 4.450000000000000178 ) ) ;
#31305 = CARTESIAN_POINT ( 'NONE',  ( 22.18053613645642841, 6.281410551025238043, 11.49999999999999645 ) ) ;
#31306 = CARTESIAN_POINT ( 'NONE',  ( 15.15630024635751383, 17.02982414992789018, 11.49999999999998934 ) ) ;
#31307 = CARTESIAN_POINT ( 'NONE',  ( -74.54565784544875839, -24.34968618360933590, 0.1864209137778816416 ) ) ;
#31308 = B_SPLINE_SURFACE_WITH_KNOTS ( 'NONE', 3, 1, ( 
 ( #46530, #23675 ),
 ( #17072, #40421 ),
 ( #15568, #100282 ),
 ( #56158, #54650 ),
 ( #85582, #16064 ),
 ( #69364, #47037 ),
 ( #87086, #79475 ),
 ( #16564, #39911 ),
 ( #47538, #30803 ),
 ( #38411, #77953 ),
 ( #1367, #63275 ),
 ( #92687, #8466 ),
 ( #39417, #853 ),
 ( #31807, #24676 ),
 ( #349, #77458 ) ),
 .UNSPECIFIED., .F., .F., .F.,
 ( 4, 1, 1, 1, 1, 1, 1, 1, 1, 1, 1, 1, 4 ),
 ( 2, 2 ),
 ( 0.000000000000000000, 0.1101655532114483721, 0.2157872561749787366, 0.3180274349094209807, 0.4175739541655078546, 0.5116504876474516905, 0.5961620971027632443, 0.6729345334849961002, 0.7436695573498580680, 0.8106770010653628900, 0.8740589623137356989, 0.9366963019193721429, 1.000000000000000000 ),
 ( 0.000000000000000000, 1.000000000000000000 ),
 .UNSPECIFIED. ) ;
#31309 = CARTESIAN_POINT ( 'NONE',  ( -96.60008298486154388, -23.48783264082477018, -1.443836473390089914 ) ) ;
#31310 = CARTESIAN_POINT ( 'NONE',  ( 0.8126045299064816874, -1.450440077808303752, -8.999999999999998224 ) ) ;
#31311 = CARTESIAN_POINT ( 'NONE',  ( -8.193370562272118462, -20.86776251599019361, 11.49999999999999645 ) ) ;
#31312 = VERTEX_POINT ( 'NONE', #55260 ) ;
#31313 = CARTESIAN_POINT ( 'NONE',  ( -64.52287095715006160, -29.50248528299804818, 1.056150453629034924 ) ) ;
#31314 = CARTESIAN_POINT ( 'NONE',  ( -72.62287095715005592, -29.50248528299804818, 1.056150453629036701 ) ) ;
#31315 = CARTESIAN_POINT ( 'NONE',  ( -20.07106029494397248, -8.819774368769808248, 11.49999999999998934 ) ) ;
#31316 = CARTESIAN_POINT ( 'NONE',  ( 30.00738719773716312, 1.682774720514426114, -9.049252915307087974 ) ) ;
#31317 = CARTESIAN_POINT ( 'NONE',  ( -44.52975563414968008, -24.66019654487199020, 8.947790411086115725 ) ) ;
#31318 = CARTESIAN_POINT ( 'NONE',  ( -69.07358128771278416, -25.17156706459151394, 6.804697550444784859 ) ) ;
#31319 = ORIENTED_EDGE ( 'NONE', *, *, #78705, .T. ) ;
#31320 = LINE ( 'NONE', #45562, #84849 ) ;
#31321 = DIRECTION ( 'NONE',  ( -1.000000000000000000, -0.000000000000000000, -0.000000000000000000 ) ) ;
#31322 = EDGE_LOOP ( 'NONE', ( #11495, #23554, #46622, #1397 ) ) ;
#31323 = EDGE_CURVE ( 'NONE', #80599, #69536, #91780, .T. ) ;
#31324 = CARTESIAN_POINT ( 'NONE',  ( 8.813945691637787405, 18.49579627399651471, -1.500000000000002220 ) ) ;
#31325 = VERTEX_POINT ( 'NONE', #16674 ) ;
#31326 = ORIENTED_EDGE ( 'NONE', *, *, #52786, .F. ) ;
#31327 = ORIENTED_EDGE ( 'NONE', *, *, #20402, .F. ) ;
#31328 = ORIENTED_EDGE ( 'NONE', *, *, #65486, .T. ) ;
#31329 = CARTESIAN_POINT ( 'NONE',  ( -13.34915495237762251, 18.83725853537101358, -1.500000000000002220 ) ) ;
#31330 = CARTESIAN_POINT ( 'NONE',  ( -49.15015151476772814, -25.24433540152454825, 3.685374804461877929 ) ) ;
#31331 = CARTESIAN_POINT ( 'NONE',  ( -8.348131891436525009, -18.51812344263101906, -1.500000000000002220 ) ) ;
#31332 = AXIS2_PLACEMENT_3D ( 'NONE', #49488, #65227, #3321 ) ;
#31333 = EDGE_CURVE ( 'NONE', #79616, #78997, #24783, .T. ) ;
#31334 = VERTEX_POINT ( 'NONE', #71482 ) ;
#31335 = DIRECTION ( 'NONE',  ( 0.000000000000000000, -2.173523156925980399E-06, 0.9999999999976378895 ) ) ;
#31336 = CARTESIAN_POINT ( 'NONE',  ( -87.62287095715004170, -29.50247984919015209, -1.443849546365051806 ) ) ;
#31337 = ADVANCED_FACE ( 'NONE', ( #32913 ), #49927, .T. ) ;
#31338 = PLANE ( 'NONE',  #36710 ) ;
#31339 = CARTESIAN_POINT ( 'NONE',  ( 4.627238781264984446, -5.876774720514409189, 19.49219360614394247 ) ) ;
#31341 = ORIENTED_EDGE ( 'NONE', *, *, #67338, .T. ) ;
#31340 = CARTESIAN_POINT ( 'NONE',  ( 15.57385778016992894, -14.83193121981731544, 11.49999999999999645 ) ) ;
#31342 = CARTESIAN_POINT ( 'NONE',  ( -75.64825452142250128, -23.85016227208580730, -0.8807180028928284221 ) ) ;
#31344 = AXIS2_PLACEMENT_3D ( 'NONE', #53528, #7321, #13941 ) ;
#31343 = CARTESIAN_POINT ( 'NONE',  ( 23.91005183030481263, -4.132774720514426292, -14.40591128290692069 ) ) ;
#31345 = EDGE_CURVE ( 'NONE', #88329, #86782, #3471, .T. ) ;
#31346 = ORIENTED_EDGE ( 'NONE', *, *, #56542, .T. ) ;
#31347 = EDGE_CURVE ( 'NONE', #59306, #27806, #50647, .T. ) ;
#31348 = CARTESIAN_POINT ( 'NONE',  ( 20.09396958936853395, 5.161349618257207617, 11.49999999999998934 ) ) ;
#31349 = VERTEX_POINT ( 'NONE', #33908 ) ;
#31351 = ORIENTED_EDGE ( 'NONE', *, *, #21976, .T. ) ;
#31350 = LINE ( 'NONE', #62314, #78221 ) ;
#31352 = CARTESIAN_POINT ( 'NONE',  ( -111.5135283796893617, -24.66019654487200441, 8.947790411086105067 ) ) ;
#31353 = CARTESIAN_POINT ( 'NONE',  ( -61.52287095715006160, -24.65952944569304606, 1.056160979905695463 ) ) ;
#31354 = ORIENTED_EDGE ( 'NONE', *, *, #14486, .F. ) ;
#31355 = ORIENTED_EDGE ( 'NONE', *, *, #60694, .T. ) ;
#31356 = CARTESIAN_POINT ( 'NONE',  ( 4.967620699791259753, -6.376774720514415407, 19.94530485585548973 ) ) ;
#31357 = DIRECTION ( 'NONE',  ( 0.000000000000000000, 0.000000000000000000, 1.000000000000000000 ) ) ;
#31358 = EDGE_CURVE ( 'NONE', #5872, #82135, #88700, .T. ) ;
#31359 = CARTESIAN_POINT ( 'NONE',  ( -102.5228709571500332, -24.33927499327854349, 9.819080762295810061 ) ) ;
#31360 = CARTESIAN_POINT ( 'NONE',  ( 21.66556372666567754, 3.824538051775513647, 11.49999999999999645 ) ) ;
#31361 = CARTESIAN_POINT ( 'NONE',  ( -89.58845897716231832, -24.35071581493543391, 9.817618358456025263 ) ) ;
#31362 = CARTESIAN_POINT ( 'NONE',  ( 13.09772080625096891, 18.35129493929886380, -1.500000000000002220 ) ) ;
#31363 = CARTESIAN_POINT ( 'NONE',  ( 18.89479412359299815, 9.153864009170110450, 11.49999999999998934 ) ) ;
#31364 = VECTOR ( 'NONE', #97321, 1000.000000000000114 ) ;
#31365 = DIRECTION ( 'NONE',  ( 1.232047923278981953E-16, 1.000000000000000000, 0.000000000000000000 ) ) ;
#31366 = ORIENTED_EDGE ( 'NONE', *, *, #16359, .F. ) ;
#31367 = ORIENTED_EDGE ( 'NONE', *, *, #57176, .F. ) ;
#31368 = LINE ( 'NONE', #15140, #27156 ) ;
#31369 = AXIS2_PLACEMENT_3D ( 'NONE', #71978, #49150, #95302 ) ;
#31370 = B_SPLINE_CURVE_WITH_KNOTS ( 'NONE', 3,
 ( #83069, #98804, #53153, #74961 ),
 .UNSPECIFIED., .F., .F.,
 ( 4, 4 ),
 ( 0.000000000000000000, 9.999999999999592548E-05 ),
 .UNSPECIFIED. ) ;
#31371 = LINE ( 'NONE', #8030, #86229 ) ;
#31372 = ORIENTED_EDGE ( 'NONE', *, *, #30311, .T. ) ;
#31373 = CARTESIAN_POINT ( 'NONE',  ( 20.98173926746349238, 2.650078317256617577, 11.49999999999998934 ) ) ;
#31374 = LINE ( 'NONE', #99864, #64456 ) ;
#31375 = CARTESIAN_POINT ( 'NONE',  ( -61.66187308073543250, -25.27183489919806192, 3.712349809207165841 ) ) ;
#31376 = CARTESIAN_POINT ( 'NONE',  ( -121.5883704999377102, -24.65952944569305316, 1.056160979905707897 ) ) ;
#31377 = CARTESIAN_POINT ( 'NONE',  ( -94.52287095715006160, -23.47596703998600631, 11.44779298504228393 ) ) ;
#31379 = B_SPLINE_CURVE_WITH_KNOTS ( 'NONE', 3,
 ( #30064, #28579, #90479, #37684 ),
 .UNSPECIFIED., .F., .F.,
 ( 4, 4 ),
 ( 0.8310934634990968517, 0.8400998947712122744 ),
 .UNSPECIFIED. ) ;
#31378 = CARTESIAN_POINT ( 'NONE',  ( -127.5228709571500616, -24.35013146730204525, 9.818937971375092388 ) ) ;
#31380 = CARTESIAN_POINT ( 'NONE',  ( 13.47465251475156656, -17.59220275312388182, -1.500000000000002220 ) ) ;
#31381 = VECTOR ( 'NONE', #61097, 1000.000000000000114 ) ;
#31382 = CARTESIAN_POINT ( 'NONE',  ( 0.3910256410256383042, -6.376774720514408301, 19.19230769230768985 ) ) ;
#31383 = EDGE_CURVE ( 'NONE', #65831, #87201, #45780, .T. ) ;
#31384 = ORIENTED_EDGE ( 'NONE', *, *, #70272, .F. ) ;
#31385 = PLANE ( 'NONE',  #25436 ) ;
#31386 = CARTESIAN_POINT ( 'NONE',  ( -10.24059822343757986, -6.376774720514426953, 22.82308057603840368 ) ) ;
#31387 = CARTESIAN_POINT ( 'NONE',  ( -43.62287095715004881, -23.48783264082477729, -1.443836473390071928 ) ) ;
#31388 = EDGE_CURVE ( 'NONE', #65697, #22696, #4633, .T. ) ;
#31389 = CARTESIAN_POINT ( 'NONE',  ( -100.6244608836033336, -24.92564183028979130, 1.928384488918251760 ) ) ;
#31390 = CARTESIAN_POINT ( 'NONE',  ( -34.62287095715005592, -29.50250243563736774, 8.947779886222150481 ) ) ;
#31391 = CARTESIAN_POINT ( 'NONE',  ( 19.33761327413411024, 2.027444641817329973, 11.49999999999998934 ) ) ;
#31392 = CARTESIAN_POINT ( 'NONE',  ( -13.99230614532761052, -16.21612836239924960, 11.49999999999998934 ) ) ;
#31393 = CARTESIAN_POINT ( 'NONE',  ( -62.54344358126193271, -24.34968618360933945, 0.1864209137778798930 ) ) ;
#31394 = CARTESIAN_POINT ( 'NONE',  ( -60.49077534611401319, -24.63419186845290199, 9.035850630957110496 ) ) ;
#31395 = DIRECTION ( 'NONE',  ( 0.7071067811865476838, 0.000000000000000000, -0.7071067811865474617 ) ) ;
#31396 = CARTESIAN_POINT ( 'NONE',  ( -101.0406423489954477, -25.27360018180653967, 3.494480365757756779 ) ) ;
#31397 = CARTESIAN_POINT ( 'NONE',  ( -5.793434319722853054, -21.96748078227757617, -1.500000000000002220 ) ) ;
#31398 = B_SPLINE_SURFACE_WITH_KNOTS ( 'NONE', 3, 1, ( 
 ( #30844, #49089 ),
 ( #80019, #57210 ),
 ( #80520, #18123 ),
 ( #56708, #25227 ),
 ( #64835, #26237 ),
 ( #2409, #10007 ),
 ( #11012, #47585 ),
 ( #18612, #86631 ),
 ( #72921, #56205 ),
 ( #87131, #95746 ),
 ( #10504, #40965 ) ),
 .UNSPECIFIED., .F., .F., .F.,
 ( 4, 1, 1, 1, 1, 1, 1, 1, 4 ),
 ( 2, 2 ),
 ( 0.000000000000000000, 0.1219040408698844752, 0.2394126076020045568, 0.3554101042801769972, 0.4720907288033014959, 0.5928589821563612361, 0.7187034677136832084, 0.8548923829515286954, 0.9999999999999998890 ),
 ( 0.000000000000000000, 1.000000000000000000 ),
 .UNSPECIFIED. ) ;
#31399 = EDGE_CURVE ( 'NONE', #19500, #30802, #22761, .T. ) ;
#31400 = CARTESIAN_POINT ( 'NONE',  ( -17.64648606763744354, -5.965225279485594001, -23.04404205923972526 ) ) ;
#31401 = FACE_OUTER_BOUND ( 'NONE', #35529, .T. ) ;
#31402 = CARTESIAN_POINT ( 'NONE',  ( 16.46483878678964174, 11.07114234313464252, 11.49999999999999645 ) ) ;
#31403 = CARTESIAN_POINT ( 'NONE',  ( 5.344006250707635353, -6.376774720514418959, 20.55781796641452885 ) ) ;
#31404 = CARTESIAN_POINT ( 'NONE',  ( -31.52287095715006160, -23.47593901973090169, -1.443836447538997536 ) ) ;
#31405 = ORIENTED_EDGE ( 'NONE', *, *, #41131, .F. ) ;
#31406 = CARTESIAN_POINT ( 'NONE',  ( 3.106028565906091998, -6.376774720514426953, 3.106028565906120864 ) ) ;
#31407 = ADVANCED_FACE ( 'NONE', ( #19169 ), #74461, .F. ) ;
#31408 = CARTESIAN_POINT ( 'NONE',  ( -80.52287095715007581, -24.91570333825475458, 8.075032458260915647 ) ) ;
#31409 = VECTOR ( 'NONE', #16086, 1000.000000000000114 ) ;
#31410 = DIRECTION ( 'NONE',  ( -0.9888510809027409865, 4.164321980682959710E-15, -0.1489078231574183231 ) ) ;
#31411 = CARTESIAN_POINT ( 'NONE',  ( -10.14273968512601520, 19.10955606681249463, -1.500000000000002220 ) ) ;
#31412 = CARTESIAN_POINT ( 'NONE',  ( -29.62287096154833677, -23.39681786206389447, 11.44779298504227860 ) ) ;
#31413 = CARTESIAN_POINT ( 'NONE',  ( -14.39514105012195344, 13.04300321504834947, -1.500000000000002220 ) ) ;
#31414 = CARTESIAN_POINT ( 'NONE',  ( -55.59257803871130932, -24.40133493613049964, 9.663955038902800609 ) ) ;
#31415 = CARTESIAN_POINT ( 'NONE',  ( 17.96171645398845129, 8.431260308876343146, 11.49999999999998934 ) ) ;
#31416 = ORIENTED_EDGE ( 'NONE', *, *, #1107, .T. ) ;
#31417 = AXIS2_PLACEMENT_3D ( 'NONE', #39441, #40942, #41444 ) ;
#31418 = CARTESIAN_POINT ( 'NONE',  ( -2.125485521908593078, 20.27274140177646444, 11.49999999999999645 ) ) ;
#31419 = CARTESIAN_POINT ( 'NONE',  ( -80.55868892812124216, -23.85016227208580730, -0.8807180028928341953 ) ) ;
#31420 = CC_DESIGN_PERSON_AND_ORGANIZATION_ASSIGNMENT ( #43277, #82321, ( #51515 ) ) ;
#31421 = CARTESIAN_POINT ( 'NONE',  ( -123.5228709571500616, -29.50250243563736774, 8.947779886222134493 ) ) ;
#31422 = EDGE_LOOP ( 'NONE', ( #79687, #77108, #89343, #16258 ) ) ;
#31423 = CARTESIAN_POINT ( 'NONE',  ( -41.41113444086114725, -25.26397904058624277, 3.881650733674827602 ) ) ;
#31424 = CARTESIAN_POINT ( 'NONE',  ( -92.52287095715007581, -24.50216790748206108, 0.6166512839542513946 ) ) ;
#31425 = CARTESIAN_POINT ( 'NONE',  ( -27.96875734969026084, 6.376774720514426953, -0.08597719988137648983 ) ) ;
#31426 = DIRECTION ( 'NONE',  ( 0.000000000000000000, 1.734723475976807094E-15, 1.000000000000000000 ) ) ;
#31427 = DIRECTION ( 'NONE',  ( -3.773278334453079618E-23, 0.9999999999976377785, 2.173523156925979975E-06 ) ) ;
#31428 = CARTESIAN_POINT ( 'NONE',  ( 17.00595499256408871, 10.69956108467327205, 11.49999999999998934 ) ) ;
#31429 = AXIS2_PLACEMENT_3D ( 'NONE', #41442, #73886, #19588 ) ;
#31430 = DIRECTION ( 'NONE',  ( 3.773278334444167608E-23, -1.000000000000000000, 0.000000000000000000 ) ) ;
#31431 = ORIENTED_EDGE ( 'NONE', *, *, #60898, .T. ) ;
#31432 = LINE ( 'NONE', #72009, #47919 ) ;
#31433 = CARTESIAN_POINT ( 'NONE',  ( -22.32109313027335062, -5.015931025267754251, 11.49999999999999645 ) ) ;
#31434 = CARTESIAN_POINT ( 'NONE',  ( -20.26579564662877075, -10.28286414166031726, -1.500000000000002220 ) ) ;
#31435 = VERTEX_POINT ( 'NONE', #34908 ) ;
#31436 = CARTESIAN_POINT ( 'NONE',  ( -71.70011599639640565, -25.23854420923243325, 6.372362213873513426 ) ) ;
#31437 = FACE_OUTER_BOUND ( 'NONE', #66297, .T. ) ;
#31438 = CYLINDRICAL_SURFACE ( 'NONE', #24111, 1.836000000000000743 ) ;
#31439 = CARTESIAN_POINT ( 'NONE',  ( -30.57287095715006231, -24.49177996402112356, 9.428047631786927951 ) ) ;
#31440 = CARTESIAN_POINT ( 'NONE',  ( -128.5218873095093954, -23.96169478059714919, 10.65365249895717170 ) ) ;
#31441 = CARTESIAN_POINT ( 'NONE',  ( 17.51792015816173986, -5.965225279485572685, 29.01255224319336889 ) ) ;
#31442 = ORIENTED_EDGE ( 'NONE', *, *, #59294, .T. ) ;
#31443 = CARTESIAN_POINT ( 'NONE',  ( 16.53694760393551988, -11.94906295602464397, 11.49999999999998934 ) ) ;
#31444 = ORIENTED_EDGE ( 'NONE', *, *, #90843, .T. ) ;
#31445 = EDGE_CURVE ( 'NONE', #19525, #16750, #88219, .T. ) ;
#31446 = B_SPLINE_CURVE_WITH_KNOTS ( 'NONE', 3,
 ( #88821, #18791, #11188, #80200 ),
 .UNSPECIFIED., .F., .F.,
 ( 4, 4 ),
 ( 0.000000000000000000, 1.000000000000000000 ),
 .UNSPECIFIED. ) ;
#31447 = CARTESIAN_POINT ( 'NONE',  ( -14.90462150274475306, 17.49973755783957685, 11.49999999999998934 ) ) ;
#31448 = CARTESIAN_POINT ( 'NONE',  ( -54.49167730237748231, -24.51419770103157347, 9.386484678747178734 ) ) ;
#31449 = ORIENTED_EDGE ( 'NONE', *, *, #98274, .T. ) ;
#31450 = CARTESIAN_POINT ( 'NONE',  ( -101.6228709571500843, -24.50321055353805377, 9.387540953477515160 ) ) ;
#31451 = CARTESIAN_POINT ( 'NONE',  ( -81.04628668253678825, -25.15830465083685752, 6.953829097328267927 ) ) ;
#31452 = CARTESIAN_POINT ( 'NONE',  ( -96.62287095715005592, -23.47593901973091235, -1.443836447539001089 ) ) ;
#31454 = ORIENTED_EDGE ( 'NONE', *, *, #90920, .T. ) ;
#31453 = CARTESIAN_POINT ( 'NONE',  ( 7.794017451908327843, -19.83292067980804774, 11.49999999999999645 ) ) ;
#31455 = B_SPLINE_CURVE_WITH_KNOTS ( 'NONE', 3,
 ( #55030, #46912, #9843, #2248 ),
 .UNSPECIFIED., .F., .F.,
 ( 4, 4 ),
 ( 0.000000000000000000, 9.999999999998897304E-05 ),
 .UNSPECIFIED. ) ;
#31456 = EDGE_CURVE ( 'NONE', #94742, #61907, #51129, .T. ) ;
#31457 = ORIENTED_EDGE ( 'NONE', *, *, #32717, .T. ) ;
#31458 = CARTESIAN_POINT ( 'NONE',  ( 9.120982285578694615, 20.23247719416018242, -1.500000000000002220 ) ) ;
#31459 = EDGE_CURVE ( 'NONE', #46359, #41475, #83560, .T. ) ;
#31460 = CARTESIAN_POINT ( 'NONE',  ( 16.46467569749531634, 12.45148609503053017, -1.500000000000002220 ) ) ;
#31461 = VECTOR ( 'NONE', #70103, 1000.000000000000114 ) ;
#31462 = ORIENTED_EDGE ( 'NONE', *, *, #21004, .F. ) ;
#31463 = ORIENTED_EDGE ( 'NONE', *, *, #16553, .T. ) ;
#31464 = CARTESIAN_POINT ( 'NONE',  ( -112.6228709571500701, -24.50321055353806443, 9.387540953477524042 ) ) ;
#31465 = CARTESIAN_POINT ( 'NONE',  ( -95.63923326134215586, -23.85049219812686161, 10.88485053497527133 ) ) ;
#31466 = ORIENTED_EDGE ( 'NONE', *, *, #40169, .T. ) ;
#31467 = CARTESIAN_POINT ( 'NONE',  ( -50.12942939268734932, -25.13686567213617806, 7.080268837617579969 ) ) ;
#31468 = ORIENTED_EDGE ( 'NONE', *, *, #21069, .T. ) ;
#31469 = CARTESIAN_POINT ( 'NONE',  ( -58.58292334261074075, -24.51419770103156637, 9.386484678747176957 ) ) ;
#31470 = DIRECTION ( 'NONE',  ( -0.6451914333552788428, 0.000000000000000000, -0.7640209514960704107 ) ) ;
#31471 = CARTESIAN_POINT ( 'NONE',  ( -15.88994834598175387, -13.44966708658631838, -1.500000000000002220 ) ) ;
#31472 = EDGE_CURVE ( 'NONE', #46485, #67426, #8384, .T. ) ;
#31473 = CARTESIAN_POINT ( 'NONE',  ( 21.07893183998518438, -5.767110019903106455, 11.49999999999999645 ) ) ;
#31474 = CIRCLE ( 'NONE', #96310, 1.000000000000000000 ) ;
#31475 = FACE_OUTER_BOUND ( 'NONE', #84406, .T. ) ;
#31476 = CARTESIAN_POINT ( 'NONE',  ( -78.62361342553873556, -24.66019654487200441, 8.947790411086119278 ) ) ;
#31477 = CARTESIAN_POINT ( 'NONE',  ( -21.16806448877717628, 7.570426553894726851, -1.500000000000002220 ) ) ;
#31478 = CARTESIAN_POINT ( 'NONE',  ( -118.6235039397453335, -24.66019654487199730, 8.947790411086115725 ) ) ;
#31479 = DIRECTION ( 'NONE',  ( 0.000000000000000000, 0.9999999999976377785, 2.173523156925979975E-06 ) ) ;
#31480 = CARTESIAN_POINT ( 'NONE',  ( 4.689770114687411784, -5.876774720514424288, 21.33175327469028915 ) ) ;
#31481 = ORIENTED_EDGE ( 'NONE', *, *, #24819, .T. ) ;
#31482 = ORIENTED_EDGE ( 'NONE', *, *, #97660, .T. ) ;
#31483 = ORIENTED_EDGE ( 'NONE', *, *, #16939, .F. ) ;
#31484 = CARTESIAN_POINT ( 'NONE',  ( -11.21157863559261791, -18.18922556752850994, -1.500000000000002220 ) ) ;
#31485 = VERTEX_POINT ( 'NONE', #53138 ) ;
#31486 = CARTESIAN_POINT ( 'NONE',  ( 19.40125262130244366, -8.172613994405130811, 11.49999999999998934 ) ) ;
#31487 = CARTESIAN_POINT ( 'NONE',  ( -30.43724401707702754, -24.37552172231524494, 0.3015907515355735202 ) ) ;
#31488 = CARTESIAN_POINT ( 'NONE',  ( 6.088051586893210576, -19.00464151315268424, -1.500000000000002220 ) ) ;
#31489 = CARTESIAN_POINT ( 'NONE',  ( -50.47720752119995780, -24.92592662359561473, 8.075495903018000021 ) ) ;
#31490 = CARTESIAN_POINT ( 'NONE',  ( 2.922108196329484375, -6.376774720514417183, 20.36383711510645256 ) ) ;
#31491 = CARTESIAN_POINT ( 'NONE',  ( 5.346615758220810477, 21.33151429383102382, -1.500000000000002220 ) ) ;
#31492 = DIRECTION ( 'NONE',  ( 0.000000000000000000, -2.173523156925979552E-06, 0.9999999999976378895 ) ) ;
#31493 = VERTEX_POINT ( 'NONE', #75945 ) ;
#31494 = CARTESIAN_POINT ( 'NONE',  ( 3.106028565906091998, -5.876774720514426953, 3.106028565906120864 ) ) ;
#31495 = CARTESIAN_POINT ( 'NONE',  ( -12.64432969575900323, -5.965225279485592225, -26.13179214487284696 ) ) ;
#31496 = CARTESIAN_POINT ( 'NONE',  ( -20.80165436122882383, -1.723964017131293103, 11.49999999999999645 ) ) ;
#31497 = EDGE_CURVE ( 'NONE', #83300, #16519, #15049, .T. ) ;
#31498 = CARTESIAN_POINT ( 'NONE',  ( 31.63608487984670958, -3.398012287350409277, 27.34773272911736797 ) ) ;
#31499 = CARTESIAN_POINT ( 'NONE',  ( -2.499999999999996891, 4.999999999999999112, 2.100000000000000089 ) ) ;
#31500 = AXIS2_PLACEMENT_3D ( 'NONE', #10070, #8576, #48656 ) ;
#31501 = CARTESIAN_POINT ( 'NONE',  ( -38.62287095715005592, -24.66019654487199020, 8.947790411086137041 ) ) ;
#31502 = CARTESIAN_POINT ( 'NONE',  ( 21.17668642892995834, 2.279540523802085605, -1.500000000000002220 ) ) ;
#31503 = CARTESIAN_POINT ( 'NONE',  ( -46.62287095715004881, -23.48786465467241058, 11.44779295918255180 ) ) ;
#31504 = DIRECTION ( 'NONE',  ( -1.000000000000000000, -0.000000000000000000, 0.000000000000000000 ) ) ;
#31505 = B_SPLINE_CURVE_WITH_KNOTS ( 'NONE', 3,
 ( #41548, #64408, #48674, #43423 ),
 .UNSPECIFIED., .F., .F.,
 ( 4, 4 ),
 ( 0.8110791717832845915, 0.8200856030554002363 ),
 .UNSPECIFIED. ) ;
#31506 = DIRECTION ( 'NONE',  ( -0.000000000000000000, 1.000000000000000000, -0.000000000000000000 ) ) ;
#31507 = CARTESIAN_POINT ( 'NONE',  ( -5.576690828732316696, -5.876774720514418071, 20.34213149456667935 ) ) ;
#31508 = CARTESIAN_POINT ( 'NONE',  ( -12.86601690267178100, 18.50254183665605012, -1.500000000000002220 ) ) ;
#31509 = EDGE_CURVE ( 'NONE', #81354, #73682, #34826, .T. ) ;
#31510 = CARTESIAN_POINT ( 'NONE',  ( -129.5228709571500758, -24.65952944569305316, 1.056160979905707675 ) ) ;
#31511 = VERTEX_POINT ( 'NONE', #45522 ) ;
#31512 = CARTESIAN_POINT ( 'NONE',  ( -79.26673083468246261, -25.30578403561748146, 5.000323484767054794 ) ) ;
#31513 = CARTESIAN_POINT ( 'NONE',  ( 3.085011456917871264, -5.876774720514408301, 19.00082519311127172 ) ) ;
#31514 = CARTESIAN_POINT ( 'NONE',  ( -5.312243195520525596, -18.98051080891723430, 11.49999999999999645 ) ) ;
#31515 = CARTESIAN_POINT ( 'NONE',  ( -125.6228709571500275, -23.48783264082479505, -1.443836473390057273 ) ) ;
#31516 = CARTESIAN_POINT ( 'NONE',  ( -32.52287095715005449, -23.73934037231756022, 11.05740245334329686 ) ) ;
#31517 = ORIENTED_EDGE ( 'NONE', *, *, #37860, .F. ) ;
#31518 = CARTESIAN_POINT ( 'NONE',  ( -99.58877505434060140, -24.34968618360934300, 0.1864209137778966852 ) ) ;
#31519 = DIRECTION ( 'NONE',  ( 0.000000000000000000, 0.000000000000000000, -1.000000000000000000 ) ) ;
#31520 = CARTESIAN_POINT ( 'NONE',  ( -90.93265888899549054, -25.30572777988224331, 5.920366768842380445 ) ) ;
#31521 = DIRECTION ( 'NONE',  ( 1.000000000000000000, 3.773278334444166432E-23, 8.201307841325785021E-29 ) ) ;
#31522 = CARTESIAN_POINT ( 'NONE',  ( 11.81298147481671279, -15.83112273922526470, -1.500000000000002220 ) ) ;
#31523 = VERTEX_POINT ( 'NONE', #84064 ) ;
#31524 = CARTESIAN_POINT ( 'NONE',  ( -120.5228709571500048, -24.52323809116984066, 9.355190652339418378 ) ) ;
#31525 = AXIS2_PLACEMENT_3D ( 'NONE', #25689, #18078, #67630 ) ;
#31526 = EDGE_CURVE ( 'NONE', #1781, #16401, #5941, .T. ) ;
#31527 = APPLICATION_PROTOCOL_DEFINITION ( 'international standard', 'config_control_design', 1994, #9663 ) ;
#31528 = VERTEX_POINT ( 'NONE', #29783 ) ;
#31529 = CARTESIAN_POINT ( 'NONE',  ( -109.6228709571500275, -23.73934037231757799, 11.05740245334328087 ) ) ;
#31530 = DIRECTION ( 'NONE',  ( -1.000000000000000000, -3.773278334444167608E-23, -8.201307833595939069E-29 ) ) ;
#31531 = CARTESIAN_POINT ( 'NONE',  ( -100.6183367005896514, -25.30264758658750779, 4.735178788106561676 ) ) ;
#31532 = CARTESIAN_POINT ( 'NONE',  ( -99.65618967412262919, -25.26638501296867645, 7.377943290858292258 ) ) ;
#31533 = CARTESIAN_POINT ( 'NONE',  ( -67.62287095715008434, -24.33832256526968507, 0.1851278514119886476 ) ) ;
#31534 = CARTESIAN_POINT ( 'NONE',  ( -59.52287095715009002, -23.47593901973090524, -1.443836447538997092 ) ) ;
#31535 = FACE_OUTER_BOUND ( 'NONE', #54481, .T. ) ;
#31536 = CARTESIAN_POINT ( 'NONE',  ( 18.80801646011137507, -6.797914457553222434, -1.500000000000002220 ) ) ;
#31537 = CIRCLE ( 'NONE', #67268, 24.00000000000000000 ) ;
#31538 = CARTESIAN_POINT ( 'NONE',  ( -99.29064586046420970, -25.27532990705892146, 3.426410652678359092 ) ) ;
#31539 = FACE_OUTER_BOUND ( 'NONE', #85213, .T. ) ;
#31540 = VERTEX_POINT ( 'NONE', #61751 ) ;
#31541 = EDGE_CURVE ( 'NONE', #58944, #76875, #8221, .T. ) ;
#31542 = ADVANCED_FACE ( 'NONE', ( #46020 ), #76440, .T. ) ;
#31543 = B_SPLINE_CURVE_WITH_KNOTS ( 'NONE', 3,
 ( #14906, #47378, #23007, #84925 ),
 .UNSPECIFIED., .F., .F.,
 ( 4, 4 ),
 ( 0.000000000000000000, 9.999999999998897304E-05 ),
 .UNSPECIFIED. ) ;
#31544 = ADVANCED_FACE ( 'NONE', ( #44011 ), #76938, .T. ) ;
#31545 = DIRECTION ( 'NONE',  ( -0.000000000000000000, -0.000000000000000000, -1.000000000000000000 ) ) ;
#31546 = CARTESIAN_POINT ( 'NONE',  ( -109.4273347235498193, -25.29012848027490179, 3.857971622509586584 ) ) ;
#31547 = CARTESIAN_POINT ( 'NONE',  ( -120.6228709571500417, -23.48783264082479505, -1.443836473390058384 ) ) ;
#31548 = CARTESIAN_POINT ( 'NONE',  ( -100.5228709571501042, -24.83620972994592790, 8.398175272781370992 ) ) ;
#31549 = DIRECTION ( 'NONE',  ( 0.000000000000000000, -1.000000000000000000, 0.000000000000000000 ) ) ;
#31550 = DIRECTION ( 'NONE',  ( -0.000000000000000000, 0.000000000000000000, -1.000000000000000000 ) ) ;
#31551 = CARTESIAN_POINT ( 'NONE',  ( -3.108425644221024520, -5.876774720514416295, 20.25188360057253334 ) ) ;
#31552 = CARTESIAN_POINT ( 'NONE',  ( 0.06697178475903577122, -5.876774720514410077, 19.29815762497054976 ) ) ;
#31553 = VERTEX_POINT ( 'NONE', #52130 ) ;
#31554 = CARTESIAN_POINT ( 'NONE',  ( 18.81862293822770837, 7.596102252255398035, 11.49999999999998934 ) ) ;
#31555 = B_SPLINE_CURVE_WITH_KNOTS ( 'NONE', 3,
 ( #18141, #70941, #72941, #2427, #17642, #79032, #71441, #78522 ),
 .UNSPECIFIED., .F., .F.,
 ( 4, 2, 2, 4 ),
 ( 0.000000000000000000, 0.002001098010032690590, 0.003001647015049033716, 0.004002196020065376843 ),
 .UNSPECIFIED. ) ;
#31556 = B_SPLINE_CURVE_WITH_KNOTS ( 'NONE', 3,
 ( #84006, #99709, #14492, #37838 ),
 .UNSPECIFIED., .F., .F.,
 ( 4, 4 ),
 ( 0.000000000000000000, 9.999999999998897304E-05 ),
 .UNSPECIFIED. ) ;
#31557 = ADVANCED_FACE ( 'NONE', ( #92670, #38391 ), #14043, .T. ) ;
#31558 = CARTESIAN_POINT ( 'NONE',  ( -73.62287095715005592, -23.48786465467241058, 11.44779295918254469 ) ) ;
#31559 = CARTESIAN_POINT ( 'NONE',  ( -99.62287095715002749, -23.94994826722516379, -0.6494450866351717533 ) ) ;
#31560 = EDGE_LOOP ( 'NONE', ( #93271, #80593, #98335, #10288 ) ) ;
#31561 = CARTESIAN_POINT ( 'NONE',  ( 31.74473449900405697, -4.976825198871215328, -4.259190951192157293 ) ) ;
#31562 = CARTESIAN_POINT ( 'NONE',  ( -18.49208213979201076, -7.923680710433813168, -1.500000000000002220 ) ) ;
#31563 = CARTESIAN_POINT ( 'NONE',  ( 21.03498508994548999, -2.205306954651367946, 11.49999999999999645 ) ) ;
#31564 = VECTOR ( 'NONE', #46022, 1000.000000000000000 ) ;
#31565 = CARTESIAN_POINT ( 'NONE',  ( -8.904070064990065703, -20.24664451029508783, 11.49999999999998934 ) ) ;
#31566 = EDGE_CURVE ( 'NONE', #58202, #42138, #36398, .T. ) ;
#31567 = CARTESIAN_POINT ( 'NONE',  ( 4.814550503181614260, -19.98661186389175271, 11.49999999999998934 ) ) ;
#31568 = CARTESIAN_POINT ( 'NONE',  ( -60.59240994803741387, -24.40034930558990922, 0.3402023900116026289 ) ) ;
#31569 = ORIENTED_EDGE ( 'NONE', *, *, #62047, .T. ) ;
#31570 = FACE_OUTER_BOUND ( 'NONE', #45678, .T. ) ;
#31571 = VERTEX_POINT ( 'NONE', #6943 ) ;
#31572 = EDGE_CURVE ( 'NONE', #87155, #16636, #71562, .T. ) ;
#31573 = CARTESIAN_POINT ( 'NONE',  ( 3.252401863874210264, -5.965225279485592225, -29.35688408629928858 ) ) ;
#31574 = CARTESIAN_POINT ( 'NONE',  ( -80.58953762381672448, -23.47593901973091235, -1.443836447539004642 ) ) ;
#31575 = EDGE_LOOP ( 'NONE', ( #53795, #49288, #6355, #85506 ) ) ;
#31576 = ORIENTED_EDGE ( 'NONE', *, *, #32563, .T. ) ;
#31577 = ORIENTED_EDGE ( 'NONE', *, *, #65723, .T. ) ;
#31578 = CARTESIAN_POINT ( 'NONE',  ( -98.52287095715006160, -23.48783264082477018, -1.443836473390087916 ) ) ;
#31579 = CARTESIAN_POINT ( 'NONE',  ( -49.96261679139975342, -25.04210150420108505, 7.519895067019000123 ) ) ;
#31580 = CARTESIAN_POINT ( 'NONE',  ( -68.58035869059457923, -24.66019654487199375, 8.947790411086122830 ) ) ;
#31581 = CARTESIAN_POINT ( 'NONE',  ( -7.658335995763069448, 19.15843701367676388, -1.500000000000002220 ) ) ;
#31582 = ADVANCED_FACE ( 'NONE', ( #90683 ), #99767, .F. ) ;
#31583 = CARTESIAN_POINT ( 'NONE',  ( 21.52761780497506905, -1.784033869580059939, 11.49999999999999645 ) ) ;
#31584 = VERTEX_POINT ( 'NONE', #52624 ) ;
#31585 = CARTESIAN_POINT ( 'NONE',  ( -107.5228709571500758, -29.50248528299804818, 1.056150453629043584 ) ) ;
#31586 = CARTESIAN_POINT ( 'NONE',  ( 9.402885806365684829, -5.965225279485572685, 29.04108526060719342 ) ) ;
#31587 = CARTESIAN_POINT ( 'NONE',  ( -22.19192207843486386, -2.872123673023632584, 11.49999999999998934 ) ) ;
#31588 = ADVANCED_FACE ( 'NONE', ( #85061 ), #83053, .T. ) ;
#31589 = CARTESIAN_POINT ( 'NONE',  ( -47.66152167227360081, -23.48786465467240347, 11.44779295918255002 ) ) ;
#31590 = LINE ( 'NONE', #48334, #91860 ) ;
#31591 = EDGE_LOOP ( 'NONE', ( #12972, #66330, #23225, #30033 ) ) ;
#31592 = CARTESIAN_POINT ( 'NONE',  ( -119.4335848664117634, -25.40066263013008196, 5.394419962397462243 ) ) ;
#31593 = CARTESIAN_POINT ( 'NONE',  ( -120.6228709571501270, -24.83620972994592435, 8.398175272781365663 ) ) ;
#31594 = CARTESIAN_POINT ( 'NONE',  ( -18.74228827200876779, -9.293929619069025705, 11.49999999999998934 ) ) ;
#31595 = ORIENTED_EDGE ( 'NONE', *, *, #45361, .T. ) ;
#31596 = AXIS2_PLACEMENT_3D ( 'NONE', #66040, #18335, #95455 ) ;
#31597 = DIRECTION ( 'NONE',  ( -0.000000000000000000, -1.000000000000000000, -0.000000000000000000 ) ) ;
#31598 = ORIENTED_EDGE ( 'NONE', *, *, #58263, .F. ) ;
#31599 = CARTESIAN_POINT ( 'NONE',  ( -60.62287095715004881, -29.50248528299804818, 1.056150453629034924 ) ) ;
#31600 = CARTESIAN_POINT ( 'NONE',  ( -21.05374637409849825, 2.266213160971460194, -1.500000000000002220 ) ) ;
#31601 = VERTEX_POINT ( 'NONE', #93168 ) ;
#31602 = CARTESIAN_POINT ( 'NONE',  ( -50.58240830060177728, -24.73486907724918282, 1.287355809206965684 ) ) ;
#31603 = CARTESIAN_POINT ( 'NONE',  ( -15.04333773895388937, -15.80532200100455498, 11.49999999999998934 ) ) ;
#31604 = DIRECTION ( 'NONE',  ( -0.000000000000000000, -0.000000000000000000, -1.000000000000000000 ) ) ;
#31605 = CARTESIAN_POINT ( 'NONE',  ( -98.62287095715005592, -24.64898659630529210, 1.056161002820829697 ) ) ;
#31606 = CARTESIAN_POINT ( 'NONE',  ( -35.52287095715008292, -24.51254535375843702, 9.355368624242190734 ) ) ;
#31607 = CARTESIAN_POINT ( 'NONE',  ( -3.204121956075930200, -21.57847171274271858, -1.500000000000002220 ) ) ;
#31608 = CARTESIAN_POINT ( 'NONE',  ( -30.57287095715006231, -24.75555062611201507, 1.382286062901152857 ) ) ;
#31609 = ORIENTED_EDGE ( 'NONE', *, *, #21109, .T. ) ;
#31610 = CYLINDRICAL_SURFACE ( 'NONE', #89099, 3.349999999999998757 ) ;
#31611 = FACE_OUTER_BOUND ( 'NONE', #43504, .T. ) ;
#31612 = ORIENTED_EDGE ( 'NONE', *, *, #4107, .F. ) ;
#31613 = CIRCLE ( 'NONE', #42934, 251.4258649670780699 ) ;
#31614 = VECTOR ( 'NONE', #20959, 1000.000000000000114 ) ;
#31615 = ORIENTED_EDGE ( 'NONE', *, *, #51743, .F. ) ;
#31616 = ADVANCED_FACE ( 'NONE', ( #15548 ), #56139, .F. ) ;
#31617 = ORIENTED_EDGE ( 'NONE', *, *, #42264, .T. ) ;
#31618 = CARTESIAN_POINT ( 'NONE',  ( -29.16535361088288170, -25.13616264269015232, 3.785723840771683779 ) ) ;
#31619 = CARTESIAN_POINT ( 'NONE',  ( -5.366453405989236813, 0.000000000000000000, 18.35000000000000142 ) ) ;
#31620 = CARTESIAN_POINT ( 'NONE',  ( 20.41123533131232648, 5.719371238976541427, 11.49999999999998934 ) ) ;
#31621 = CARTESIAN_POINT ( 'NONE',  ( -94.54501400172604519, -24.65952944569304606, 1.056160979905701680 ) ) ;
#31622 = FACE_BOUND ( 'NONE', #878, .T. ) ;
#31623 = CARTESIAN_POINT ( 'NONE',  ( -23.71328795744024376, -0.3587747205144057872, -17.58350715675015863 ) ) ;
#31624 = FACE_BOUND ( 'NONE', #70374, .T. ) ;
#31625 = CARTESIAN_POINT ( 'NONE',  ( 3.017506814366913481, 19.14668354085002733, 11.49999999999998934 ) ) ;
#31626 = EDGE_CURVE ( 'NONE', #9739, #55399, #26379, .T. ) ;
#31627 = CARTESIAN_POINT ( 'NONE',  ( -69.37719319406642171, -25.27788132133623833, 5.961564651755576705 ) ) ;
#31628 = VERTEX_POINT ( 'NONE', #55638 ) ;
#31629 = CARTESIAN_POINT ( 'NONE',  ( -18.23695082634099407, 6.967386181637144738, 11.49999999999999645 ) ) ;
#31630 = CARTESIAN_POINT ( 'NONE',  ( -34.55620429048339304, -23.48783264082477729, -1.443836473390074593 ) ) ;
#31631 = FACE_OUTER_BOUND ( 'NONE', #72711, .T. ) ;
#31632 = VERTEX_POINT ( 'NONE', #77934 ) ;
#31633 = CARTESIAN_POINT ( 'NONE',  ( -103.5895376238167103, -23.47596703998600631, 11.44779298504227683 ) ) ;
#31634 = CARTESIAN_POINT ( 'NONE',  ( -44.52287095715006160, -23.47593901973090169, -1.443836447538997092 ) ) ;
#31635 = CARTESIAN_POINT ( 'NONE',  ( -106.5228709571500474, -24.33832256527049154, 0.1851278514138675058 ) ) ;
#31636 = CARTESIAN_POINT ( 'NONE',  ( -93.50736637352794389, -24.51419770103157703, 9.386484678747164523 ) ) ;
#31637 = CARTESIAN_POINT ( 'NONE',  ( -2.223759785643201869, -19.53228827767608777, 11.49999999999998934 ) ) ;
#31638 = CARTESIAN_POINT ( 'NONE',  ( -68.52287095715006160, -24.65952944569304606, 1.056160979905697239 ) ) ;
#31639 = ORIENTED_EDGE ( 'NONE', *, *, #53740, .F. ) ;
#31640 = B_SPLINE_CURVE_WITH_KNOTS ( 'NONE', 3,
 ( #15665, #14158, #37508, #91781, #90798, #29392 ),
 .UNSPECIFIED., .F., .F.,
 ( 4, 2, 4 ),
 ( 0.000000000000000000, 0.001380764517854769086, 0.002761529035709538171 ),
 .UNSPECIFIED. ) ;
#31641 = VECTOR ( 'NONE', #473, 1000.000000000000000 ) ;
#31642 = CARTESIAN_POINT ( 'NONE',  ( 11.83326311654409935, 18.06170320929925310, 11.49999999999998934 ) ) ;
#31643 = CARTESIAN_POINT ( 'NONE',  ( -40.47826423538212737, -24.73486907724917927, 1.287355809206960577 ) ) ;
#31644 = CARTESIAN_POINT ( 'NONE',  ( -77.62287095715005592, -23.47593901973091235, -1.443836447539004642 ) ) ;
#31645 = CARTESIAN_POINT ( 'NONE',  ( 6.910522817300494225, 22.03692736239173300, -1.500000000000002220 ) ) ;
#31646 = ADVANCED_FACE ( 'NONE', ( #63763 ), #25671, .F. ) ;
#31647 = DATE_AND_TIME ( #84935, #42484 ) ;
#31648 = CARTESIAN_POINT ( 'NONE',  ( -74.52287095715007581, -23.47596703998600631, 11.44779298504228748 ) ) ;
#31649 = CARTESIAN_POINT ( 'NONE',  ( -130.5728709571500588, -23.53197991584895021, -1.479945482512685428 ) ) ;
#31650 = CARTESIAN_POINT ( 'NONE',  ( -110.6228709571500559, -29.50248789122583659, 2.256150453626215580 ) ) ;
#31651 = CARTESIAN_POINT ( 'NONE',  ( -100.4498239493576648, -25.04307398257883932, 7.563174194274490780 ) ) ;
#31652 = CARTESIAN_POINT ( 'NONE',  ( 5.642884982650352654, -5.876774720514425177, 20.85668005806743608 ) ) ;
#31653 = PLANE ( 'NONE',  #45627 ) ;
#31654 = CARTESIAN_POINT ( 'NONE',  ( -99.64934318012689118, -25.26400883459589153, 4.927356406368939901 ) ) ;
#31655 = CARTESIAN_POINT ( 'NONE',  ( -19.77041435686880533, -2.435487021107205940, 11.49999999999998934 ) ) ;
#31657 = EDGE_CURVE ( 'NONE', #35613, #23703, #23656, .T. ) ;
#31656 = CARTESIAN_POINT ( 'NONE',  ( 32.40199294184732537, -5.965225279485572685, -12.82361242714782712 ) ) ;
#31658 = CARTESIAN_POINT ( 'NONE',  ( -7.150643268323968904, -18.52920452239153448, -1.500000000000002220 ) ) ;
#31659 = EDGE_CURVE ( 'NONE', #62579, #50327, #17560, .T. ) ;
#31660 = FACE_OUTER_BOUND ( 'NONE', #16124, .T. ) ;
#31661 = EDGE_CURVE ( 'NONE', #61801, #98189, #32281, .T. ) ;
#31662 = EDGE_CURVE ( 'NONE', #12412, #65034, #8446, .T. ) ;
#31663 = DIRECTION ( 'NONE',  ( 0.000000000000000000, -1.000000000000000000, 0.000000000000000000 ) ) ;
#31664 = DIRECTION ( 'NONE',  ( 0.5656310827093757876, -2.995395837334947501E-15, 0.8246584009594636333 ) ) ;
#31665 = CARTESIAN_POINT ( 'NONE',  ( 19.40724743217988291, -7.346346906864608783, 11.49999999999999645 ) ) ;
#31666 = CARTESIAN_POINT ( 'NONE',  ( -102.5228709571500758, -23.47596703998600631, 11.44779298504228215 ) ) ;
#31667 = VECTOR ( 'NONE', #38263, 1000.000000000000227 ) ;
#31668 = CARTESIAN_POINT ( 'NONE',  ( -88.62287095715004170, -23.47593901973091235, -1.443836447539002865 ) ) ;
#31669 = CARTESIAN_POINT ( 'NONE',  ( -22.19569011343799048, 5.130922947863589378, 11.49999999999999645 ) ) ;
#31670 = VECTOR ( 'NONE', #1880, 1000.000000000000114 ) ;
#31671 = VERTEX_POINT ( 'NONE', #63251 ) ;
#31672 = CARTESIAN_POINT ( 'NONE',  ( -57.62287095715002749, -24.51283580621364422, 0.6167428607019694864 ) ) ;
#31673 = DIRECTION ( 'NONE',  ( 1.000000000000000000, 0.000000000000000000, 0.000000000000000000 ) ) ;
#31674 = B_SPLINE_CURVE_WITH_KNOTS ( 'NONE', 3,
 ( #96688, #64274, #10451, #25680, #56651, #87588, #72370, #2865 ),
 .UNSPECIFIED., .F., .F.,
 ( 4, 2, 2, 4 ),
 ( -0.001240355328176840580, -0.0002398155169399329104, 0.0007607242942969747596, 0.002761803916770785763 ),
 .UNSPECIFIED. ) ;
#31675 = ORIENTED_EDGE ( 'NONE', *, *, #5837, .T. ) ;
#31676 = VECTOR ( 'NONE', #51236, 1000.000000000000000 ) ;
#31677 = CARTESIAN_POINT ( 'NONE',  ( 2.532258636284850706, -20.04889675553949147, 11.49999999999998934 ) ) ;
#31678 = EDGE_CURVE ( 'NONE', #37802, #23353, #17053, .T. ) ;
#31679 = EDGE_CURVE ( 'NONE', #81281, #79893, #54629, .T. ) ;
#31680 = CARTESIAN_POINT ( 'NONE',  ( -4.700032041049139409, -6.144890974841530351, 9.000000000000000000 ) ) ;
#31681 = VECTOR ( 'NONE', #84393, 1000.000000000000000 ) ;
#31682 = CARTESIAN_POINT ( 'NONE',  ( -97.62287095715005592, -24.64965695001468404, 8.947790433994178727 ) ) ;
#31683 = ORIENTED_EDGE ( 'NONE', *, *, #58385, .T. ) ;
#31684 = VECTOR ( 'NONE', #28454, 1000.000000000000000 ) ;
#31685 = VERTEX_POINT ( 'NONE', #9945 ) ;
#31686 = EDGE_CURVE ( 'NONE', #64811, #37373, #85564, .T. ) ;
#31687 = CARTESIAN_POINT ( 'NONE',  ( -19.37210865224160017, 0.3587747205143967943, -21.60955166348796297 ) ) ;
#31688 = CARTESIAN_POINT ( 'NONE',  ( 18.88093902437788785, 12.95799798663108682, 11.49999999999998934 ) ) ;
#31689 = CARTESIAN_POINT ( 'NONE',  ( -51.23509499458276650, -25.27420657037325569, 3.726222110248589292 ) ) ;
#31690 = CARTESIAN_POINT ( 'NONE',  ( 21.02075834227166951, -5.193550065563941942, -1.500000000000002220 ) ) ;
#31691 = CARTESIAN_POINT ( 'NONE',  ( -104.6228709571500701, -24.51283580621365132, 0.6167428607019816988 ) ) ;
#31692 = CARTESIAN_POINT ( 'NONE',  ( 16.15719879640481338, -13.26386290209467944, 11.49999999999999645 ) ) ;
#31693 = EDGE_LOOP ( 'NONE', ( #11602, #73940, #39066, #61206 ) ) ;
#31694 = DIRECTION ( 'NONE',  ( 3.773278334444166432E-23, -1.000000000000000000, 0.000000000000000000 ) ) ;
#31695 = CARTESIAN_POINT ( 'NONE',  ( -68.94292010565295925, -25.24754505917867320, 6.048224126016797264 ) ) ;
#31696 = CARTESIAN_POINT ( 'NONE',  ( -21.82725030464235516, 2.967780500094957308, 11.49999999999998934 ) ) ;
#31697 = B_SPLINE_CURVE_WITH_KNOTS ( 'NONE', 3,
 ( #48215, #93871, #53824, #24362, #62946, #15244 ),
 .UNSPECIFIED., .F., .F.,
 ( 4, 2, 4 ),
 ( 1.570887131794333942E-05, 0.001396322306279759555, 0.002776935741241575838 ),
 .UNSPECIFIED. ) ;
#31698 = EDGE_CURVE ( 'NONE', #99097, #64167, #55416, .T. ) ;
#31699 = CARTESIAN_POINT ( 'NONE',  ( -124.4728709548940486, -25.40673988423725049, 2.000950542041663116 ) ) ;
#31700 = DIRECTION ( 'NONE',  ( 0.7512896232465891000, -1.109416176496795172E-16, 0.6599726524652352877 ) ) ;
#31701 = ORIENTED_EDGE ( 'NONE', *, *, #3975, .F. ) ;
#31702 = CARTESIAN_POINT ( 'NONE',  ( -49.63711845704647629, -25.27344830480632609, 3.620155576039564504 ) ) ;
#31703 = CARTESIAN_POINT ( 'NONE',  ( -46.58953762381671737, -23.48783264082478439, -1.443836473390070818 ) ) ;
#31704 = EDGE_LOOP ( 'NONE', ( #8538, #31326, #66042, #49829 ) ) ;
#31705 = DIRECTION ( 'NONE',  ( -1.000000000000000000, -9.637352644315600173E-17, 0.000000000000000000 ) ) ;
#31706 = EDGE_LOOP ( 'NONE', ( #85336, #20849, #3924, #13858 ) ) ;
#31707 = ORIENTED_EDGE ( 'NONE', *, *, #15618, .F. ) ;
#31708 = CARTESIAN_POINT ( 'NONE',  ( -61.64687923781919920, -25.20074463982482982, 3.409327697717700278 ) ) ;
#31709 = CARTESIAN_POINT ( 'NONE',  ( -92.52287095715006160, -29.50247984919015209, -1.443849546365051806 ) ) ;
#31710 = CARTESIAN_POINT ( 'NONE',  ( -4.743266218460161276, -5.876774720514413630, 19.49357334786887108 ) ) ;
#31711 = CARTESIAN_POINT ( 'NONE',  ( 13.99439195134931069, 14.96789054323355828, -1.500000000000002220 ) ) ;
#31712 = EDGE_CURVE ( 'NONE', #78336, #71801, #47016, .T. ) ;
#31713 = VERTEX_POINT ( 'NONE', #93673 ) ;
#31714 = CARTESIAN_POINT ( 'NONE',  ( -26.91814428177455909, 6.376774720514426953, 29.98490496616818746 ) ) ;
#31715 = CARTESIAN_POINT ( 'NONE',  ( -44.56898227375175026, -23.48783264082476663, -1.443836473390095021 ) ) ;
#31716 = LINE ( 'NONE', #8376, #30444 ) ;
#31717 = CARTESIAN_POINT ( 'NONE',  ( 21.78807519107708401, 4.755904613692067073, -1.500000000000002220 ) ) ;
#31718 = EDGE_CURVE ( 'NONE', #39067, #65225, #6961, .T. ) ;
#31719 = CARTESIAN_POINT ( 'NONE',  ( -55.52287095715006870, -24.92604778743017135, 8.074972756849364330 ) ) ;
#31720 = CARTESIAN_POINT ( 'NONE',  ( -26.49221882413262819, -24.65723053117703500, 7.825584094027206561 ) ) ;
#31721 = ORIENTED_EDGE ( 'NONE', *, *, #522, .F. ) ;
#31722 = ADVANCED_FACE ( 'NONE', ( #33277 ), #55135, .T. ) ;
#31723 = CARTESIAN_POINT ( 'NONE',  ( -29.36544338184978642, -24.97648490869306315, 2.618731075491085747 ) ) ;
#31724 = CARTESIAN_POINT ( 'NONE',  ( -73.52287095715010423, -23.48783264082477018, -1.443836473390093689 ) ) ;
#31725 = AXIS2_PLACEMENT_3D ( 'NONE', #84957, #53035, #21554 ) ;
#31726 = CARTESIAN_POINT ( 'NONE',  ( -17.75621389795859884, -10.86975384844714831, 11.49999999999998934 ) ) ;
#31727 = ORIENTED_EDGE ( 'NONE', *, *, #75870, .T. ) ;
#31729 = ORIENTED_EDGE ( 'NONE', *, *, #23879, .T. ) ;
#31728 = CARTESIAN_POINT ( 'NONE',  ( -51.62287095715005592, -24.64898659630367206, 1.056161002820821038 ) ) ;
#31730 = ORIENTED_EDGE ( 'NONE', *, *, #81738, .T. ) ;
#31731 = CARTESIAN_POINT ( 'NONE',  ( 21.57151214508649772, 3.625915217019311583E-15, -2.299999999999999822 ) ) ;
#31732 = CARTESIAN_POINT ( 'NONE',  ( -20.70934228997045068, 3.328930095467914185, -1.500000000000002220 ) ) ;
#31733 = ORIENTED_EDGE ( 'NONE', *, *, #8785, .T. ) ;
#31734 = CARTESIAN_POINT ( 'NONE',  ( -69.52287095715004739, -24.35013146730203815, 9.818937971375103047 ) ) ;
#31735 = CARTESIAN_POINT ( 'NONE',  ( -82.52287095715006160, -23.47593901973090169, -1.443836447538996648 ) ) ;
#31736 = FACE_OUTER_BOUND ( 'NONE', #52373, .T. ) ;
#31737 = FACE_OUTER_BOUND ( 'NONE', #87611, .T. ) ;
#31738 = CARTESIAN_POINT ( 'NONE',  ( -59.62366531831469274, -24.65952944569304961, 1.056160979905697905 ) ) ;
#31739 = DIRECTION ( 'NONE',  ( -0.000000000000000000, -1.000000000000000000, -0.000000000000000000 ) ) ;
#31741 = ORIENTED_EDGE ( 'NONE', *, *, #45551, .F. ) ;
#31740 = CARTESIAN_POINT ( 'NONE',  ( 21.18294168759468832, 6.642818831845659133, 11.49999999999999645 ) ) ;
#31742 = CARTESIAN_POINT ( 'NONE',  ( -108.6228709571500559, -23.47593901973091235, -1.443836447538999312 ) ) ;
#31743 = PLANE ( 'NONE',  #53791 ) ;
#31744 = EDGE_LOOP ( 'NONE', ( #18958, #20085, #80815, #82797 ) ) ;
#31745 = CARTESIAN_POINT ( 'NONE',  ( 12.64511023617726160, -18.80563239904246231, 11.49999999999998934 ) ) ;
#31747 = VERTEX_POINT ( 'NONE', #16542 ) ;
#31746 = CARTESIAN_POINT ( 'NONE',  ( -87.52287095715006160, -23.47593901973090524, -1.443836447538996648 ) ) ;
#31748 = B_SPLINE_CURVE_WITH_KNOTS ( 'NONE', 3,
 ( #87037, #1813, #89050, #63733 ),
 .UNSPECIFIED., .F., .F.,
 ( 4, 4 ),
 ( 0.4608290667565730359, 0.4698354980286885696 ),
 .UNSPECIFIED. ) ;
#31749 = ORIENTED_EDGE ( 'NONE', *, *, #16882, .F. ) ;
#31750 = DIRECTION ( 'NONE',  ( 0.000000000000000000, 0.000000000000000000, 1.000000000000000000 ) ) ;
#31751 = VECTOR ( 'NONE', #79984, 1000.000000000000114 ) ;
#31752 = CARTESIAN_POINT ( 'NONE',  ( 7.141438900065890216, -18.84860497471923679, -1.500000000000002220 ) ) ;
#31753 = CARTESIAN_POINT ( 'NONE',  ( -80.62287095715005592, -24.15431212366392444, -0.2830839119429126582 ) ) ;
#31754 = EDGE_LOOP ( 'NONE', ( #40851, #6238, #81759, #19944 ) ) ;
#31755 = AXIS2_PLACEMENT_3D ( 'NONE', #63590, #23993, #87401 ) ;
#31756 = CARTESIAN_POINT ( 'NONE',  ( 15.11782173391125639, -3.530785491095171924, -28.35562479723304818 ) ) ;
#31757 = CARTESIAN_POINT ( 'NONE',  ( -3.217810451210200817, -22.18463865543611391, -1.500000000000002220 ) ) ;
#31758 = AXIS2_PLACEMENT_3D ( 'NONE', #53005, #52499, #75815 ) ;
#31759 = AXIS2_PLACEMENT_3D ( 'NONE', #82774, #44229, #44723 ) ;
#31760 = VERTEX_POINT ( 'NONE', #95187 ) ;
#31761 = ORIENTED_EDGE ( 'NONE', *, *, #99421, .T. ) ;
#31762 = CARTESIAN_POINT ( 'NONE',  ( -101.5158928754072605, -25.16257325694536817, 6.338294381039898617 ) ) ;
#31763 = CARTESIAN_POINT ( 'NONE',  ( -4.401146115524053215, -6.376774720514411854, 19.34190049657481936 ) ) ;
#31764 = CARTESIAN_POINT ( 'NONE',  ( -40.35495219140244672, -25.31533539124680487, 5.080713930537138268 ) ) ;
#31765 = FACE_OUTER_BOUND ( 'NONE', #84039, .T. ) ;
#31766 = VECTOR ( 'NONE', #52152, 1000.000000000000000 ) ;
#31767 = CARTESIAN_POINT ( 'NONE',  ( -30.60914355658976049, -24.37807914296825729, 0.3010598746230576106 ) ) ;
#31768 = CARTESIAN_POINT ( 'NONE',  ( -16.69004703121433408, -10.21020960635683394, -1.500000000000002220 ) ) ;
#31769 = CARTESIAN_POINT ( 'NONE',  ( -33.52287095715006160, -24.64898659630367206, 1.056161002820817485 ) ) ;
#31770 = ORIENTED_EDGE ( 'NONE', *, *, #54270, .T. ) ;
#31771 = CARTESIAN_POINT ( 'NONE',  ( 8.645823604709390153, 19.67543227842514852, -1.500000000000002220 ) ) ;
#31772 = CARTESIAN_POINT ( 'NONE',  ( -4.568292318365942073, 0.3587747205144265483, 30.06720597538392425 ) ) ;
#31773 = DIRECTION ( 'NONE',  ( -6.924038193813838377E-14, 0.000000000000000000, -1.000000000000000000 ) ) ;
#31774 = CARTESIAN_POINT ( 'NONE',  ( -118.2228709571500787, -23.47593901973090524, -1.443836447538996426 ) ) ;
#31775 = CARTESIAN_POINT ( 'NONE',  ( -70.55620429048340725, -25.00182538069145721, 7.747789668545099317 ) ) ;
#31776 = CARTESIAN_POINT ( 'NONE',  ( 16.54545882101025711, 15.75737887292823558, -1.500000000000002220 ) ) ;
#31777 = APPLICATION_PROTOCOL_DEFINITION ( 'international standard', 'config_control_design', 1994, #87445 ) ;
#31778 = CARTESIAN_POINT ( 'NONE',  ( -46.52287095715006160, -24.64898659630367561, 1.056161002820821038 ) ) ;
#31779 = CARTESIAN_POINT ( 'NONE',  ( -92.62287095715004170, -23.72747288104469376, -1.053458166803225460 ) ) ;
#31780 = CARTESIAN_POINT ( 'NONE',  ( -10.28607412905329532, -17.16720287211733975, 11.49999999999999645 ) ) ;
#31781 = CARTESIAN_POINT ( 'NONE',  ( -54.62287095715004881, -23.48783264082478084, -1.443836473390070596 ) ) ;
#31782 = CARTESIAN_POINT ( 'NONE',  ( 8.160000000000000142, -9.123836073446797812, -2.666350264951732552 ) ) ;
#31783 = EDGE_CURVE ( 'NONE', #34238, #46809, #78443, .T. ) ;
#31784 = EDGE_CURVE ( 'NONE', #44867, #24870, #86569, .T. ) ;
#31786 = B_SPLINE_CURVE_WITH_KNOTS ( 'NONE', 3,
 ( #67500, #28923, #75582, #470 ),
 .UNSPECIFIED., .F., .F.,
 ( 4, 4 ),
 ( 0.000000000000000000, 0.0004038461538461296518 ),
 .UNSPECIFIED. ) ;
#31785 = FACE_OUTER_BOUND ( 'NONE', #45804, .T. ) ;
#31787 = DIRECTION ( 'NONE',  ( -3.773278334453079618E-23, 0.9999999999976377785, 2.173523156925979975E-06 ) ) ;
#31788 = EDGE_LOOP ( 'NONE', ( #83992, #65229, #4703, #75460 ) ) ;
#31789 = EDGE_CURVE ( 'NONE', #8495, #89963, #271, .T. ) ;
#31790 = CARTESIAN_POINT ( 'NONE',  ( -21.33044368757495590, -4.375833669458513597, 11.49999999999998934 ) ) ;
#31791 = CARTESIAN_POINT ( 'NONE',  ( -118.6228709571500559, -29.50248528299804818, 1.056150453629045360 ) ) ;
#31792 = CARTESIAN_POINT ( 'NONE',  ( 19.58216393897113505, 1.562425146961006650, -1.500000000000002220 ) ) ;
#31793 = CIRCLE ( 'NONE', #35283, 1.000000000000000888 ) ;
#31794 = EDGE_CURVE ( 'NONE', #37689, #63088, #97678, .T. ) ;
#31795 = CARTESIAN_POINT ( 'NONE',  ( -85.52287095715004739, -23.85229601348995487, 10.88205029486208808 ) ) ;
#31796 = ADVANCED_FACE ( 'NONE', ( #34791 ), #75136, .T. ) ;
#31797 = DIRECTION ( 'NONE',  ( -1.000000000000000000, 0.000000000000000000, 0.000000000000000000 ) ) ;
#31798 = PERSON_AND_ORGANIZATION_ROLE ( 'classification_officer' ) ;
#31799 = CARTESIAN_POINT ( 'NONE',  ( -91.54878298496558386, -24.35071581493543391, 9.817618358456025263 ) ) ;
#31800 = CARTESIAN_POINT ( 'NONE',  ( -73.62287095715002749, -24.51387760970725083, 9.387446482453428942 ) ) ;
#31801 = CARTESIAN_POINT ( 'NONE',  ( 12.93548710985481698, 15.95582723538240266, 11.49999999999999645 ) ) ;
#31802 = PLANE ( 'NONE',  #42477 ) ;
#31803 = CARTESIAN_POINT ( 'NONE',  ( -120.5896316483122206, -24.52300882791530512, 0.6510814631126412566 ) ) ;
#31804 = B_SPLINE_CURVE_WITH_KNOTS ( 'NONE', 3,
 ( #47095, #63839, #86643, #63332 ),
 .UNSPECIFIED., .F., .F.,
 ( 4, 4 ),
 ( 0.000000000000000000, 0.0001002978978728732653 ),
 .UNSPECIFIED. ) ;
#31805 = CARTESIAN_POINT ( 'NONE',  ( -19.71520456405594857, 11.01310763156902972, 11.49999999999999645 ) ) ;
#31806 = ORIENTED_EDGE ( 'NONE', *, *, #77076, .F. ) ;
#31807 = CARTESIAN_POINT ( 'NONE',  ( -99.52927036222322954, -25.31296297631381620, 4.031758516326467756 ) ) ;
#31808 = CARTESIAN_POINT ( 'NONE',  ( -37.52287095715009713, -23.94994826722564696, -0.6494450866342743600 ) ) ;
#31809 = CARTESIAN_POINT ( 'NONE',  ( -10.24059822343757808, -5.876774720514426953, 0.000000000000000000 ) ) ;
#31810 = LINE ( 'NONE', #352, #1337 ) ;
#31811 = EDGE_CURVE ( 'NONE', #29757, #89989, #61424, .T. ) ;
#31812 = FACE_OUTER_BOUND ( 'NONE', #33687, .T. ) ;
#31813 = CARTESIAN_POINT ( 'NONE',  ( -75.62287095715005592, -23.47593901973091235, -1.443836447539004642 ) ) ;
#31814 = VECTOR ( 'NONE', #41408, 1000.000000000000000 ) ;
#31815 = ORIENTED_EDGE ( 'NONE', *, *, #51290, .F. ) ;
#31816 = ADVANCED_FACE ( 'NONE', ( #11446 ), #12439, .T. ) ;
#31817 = DIRECTION ( 'NONE',  ( 0.8264557562326034779, 0.000000000000000000, 0.5630016722799281448 ) ) ;
#31818 = CARTESIAN_POINT ( 'NONE',  ( 13.81544771398824345, -18.15223324129861382, 11.49999999999998934 ) ) ;
#31819 = CARTESIAN_POINT ( 'NONE',  ( -74.50330917534071773, -24.34968618360933590, 0.1864209137778816416 ) ) ;
#31820 = CARTESIAN_POINT ( 'NONE',  ( -96.54971732979119281, -24.34968618360933945, 0.1864209137778868874 ) ) ;
#31821 = CARTESIAN_POINT ( 'NONE',  ( -104.5895376238167103, -24.66019654487199730, 8.947790411086122830 ) ) ;
#31822 = CARTESIAN_POINT ( 'NONE',  ( 17.95543856985664277, -13.40637504462900331, 11.49999999999999645 ) ) ;
#31823 = ORIENTED_EDGE ( 'NONE', *, *, #76331, .F. ) ;
#31824 = CARTESIAN_POINT ( 'NONE',  ( -70.62287095715007013, -24.92604778743016780, 8.074972756849353672 ) ) ;
#31825 = CARTESIAN_POINT ( 'NONE',  ( -4.809782828112996178, 21.40371668077904488, 11.49999999999998934 ) ) ;
#31826 = CARTESIAN_POINT ( 'NONE',  ( -113.5228709571500758, -23.48783264082477373, -1.443836473390082586 ) ) ;
#31827 = AXIS2_PLACEMENT_3D ( 'NONE', #40801, #2255, #31519 ) ;
#31828 = CARTESIAN_POINT ( 'NONE',  ( -34.58675657562977079, -24.35071581493542681, 9.817618358456032368 ) ) ;
#31829 = CARTESIAN_POINT ( 'NONE',  ( -1.877194073982709988, 8.794404527355018431, 0.000000000000000000 ) ) ;
#31830 = VERTEX_POINT ( 'NONE', #50028 ) ;
#31831 = CARTESIAN_POINT ( 'NONE',  ( -48.53097579249177329, -24.66019654487199730, 8.947790411086119278 ) ) ;
#31832 = DIRECTION ( 'NONE',  ( 0.000000000000000000, 0.000000000000000000, 1.000000000000000000 ) ) ;
#31833 = ORIENTED_EDGE ( 'NONE', *, *, #2318, .T. ) ;
#31834 = AXIS2_PLACEMENT_3D ( 'NONE', #4017, #43576, #66437 ) ;
#31835 = CARTESIAN_POINT ( 'NONE',  ( -18.53176153473302179, -8.692061069824589481, 11.49999999999998934 ) ) ;
#31836 = ORIENTED_EDGE ( 'NONE', *, *, #6248, .F. ) ;
#31837 = ORIENTED_EDGE ( 'NONE', *, *, #15883, .T. ) ;
#31838 = VERTEX_POINT ( 'NONE', #64772 ) ;
#31839 = ORIENTED_EDGE ( 'NONE', *, *, #65845, .T. ) ;
#31840 = CARTESIAN_POINT ( 'NONE',  ( -22.63574357292403860, -4.499050354539342322, -1.500000000000002220 ) ) ;
#31841 = CARTESIAN_POINT ( 'NONE',  ( -102.5895376238167387, -24.66019654487199730, 8.947790411086126383 ) ) ;
#31842 = CARTESIAN_POINT ( 'NONE',  ( -16.53579703214142427, -11.71821515807347680, -1.500000000000002220 ) ) ;
#31843 = ORIENTED_EDGE ( 'NONE', *, *, #44039, .F. ) ;
#31844 = DIRECTION ( 'NONE',  ( -3.773278334453079618E-23, 0.9999999999976377785, 2.173523156925979975E-06 ) ) ;
#31845 = CARTESIAN_POINT ( 'NONE',  ( -37.62287095715005592, -23.48783264082477373, -1.443836473390072372 ) ) ;
#31846 = AXIS2_PLACEMENT_3D ( 'NONE', #66272, #73369, #79969 ) ;
#31847 = EDGE_CURVE ( 'NONE', #9262, #6118, #42024, .T. ) ;
#31848 = CARTESIAN_POINT ( 'NONE',  ( -112.6228709571500559, -23.47593901973091235, -1.443836447538999312 ) ) ;
#31849 = CARTESIAN_POINT ( 'NONE',  ( -63.52287095715006160, -24.64965694238575011, 8.947790433994201820 ) ) ;
#31851 = EDGE_LOOP ( 'NONE', ( #668, #68850, #32828, #93073 ) ) ;
#31850 = CARTESIAN_POINT ( 'NONE',  ( -21.47443924280258187, -0.1944818460393343829, 11.49999999999999645 ) ) ;
#31852 = DIRECTION ( 'NONE',  ( -1.000000000000000000, 0.000000000000000000, 0.000000000000000000 ) ) ;
#31853 = CARTESIAN_POINT ( 'NONE',  ( -61.55970306133350078, -23.73791477778911840, 11.05961554403170766 ) ) ;
#31854 = VERTEX_POINT ( 'NONE', #3851 ) ;
#31855 = CARTESIAN_POINT ( 'NONE',  ( -17.23291202157775359, 11.51834372740795231, -1.500000000000002220 ) ) ;
#31856 = ADVANCED_FACE ( 'NONE', ( #18058 ), #57145, .F. ) ;
#31857 = VERTEX_POINT ( 'NONE', #58140 ) ;
#31859 = EDGE_LOOP ( 'NONE', ( #23836, #25906, #29946, #64706 ) ) ;
#31858 = LINE ( 'NONE', #17627, #55589 ) ;
#31860 = CARTESIAN_POINT ( 'NONE',  ( -111.5553594392847714, -23.96169478059714564, 10.65365249895717348 ) ) ;
#31861 = DIRECTION ( 'NONE',  ( -3.773278334453079030E-23, 0.9999999999976377785, 2.173523156925979128E-06 ) ) ;
#31862 = ORIENTED_EDGE ( 'NONE', *, *, #32762, .F. ) ;
#31863 = ORIENTED_EDGE ( 'NONE', *, *, #66367, .F. ) ;
#31864 = CARTESIAN_POINT ( 'NONE',  ( -126.6228709571500559, -29.50250786944525672, 11.44777988621622633 ) ) ;
#31865 = CARTESIAN_POINT ( 'NONE',  ( -42.59366545525777781, -24.15620529776628089, 10.23563542870661358 ) ) ;
#31866 = CARTESIAN_POINT ( 'NONE',  ( -29.52342969602818812, -25.05915383044238354, 2.942153679875703531 ) ) ;
#31867 = CARTESIAN_POINT ( 'NONE',  ( 21.95769793831392036, 2.030053023538682222, 11.49999999999999645 ) ) ;
#31868 = CARTESIAN_POINT ( 'NONE',  ( -89.51816229286842486, -23.73791477778911840, 11.05961554403170410 ) ) ;
#31869 = CARTESIAN_POINT ( 'NONE',  ( 0.2737972009257602091, 22.58959237946467624, 11.49999999999998934 ) ) ;
#31870 = VECTOR ( 'NONE', #8000, 1000.000000000000114 ) ;
#31871 = CARTESIAN_POINT ( 'NONE',  ( -5.787726610425443674, -20.20099407548119075, -1.500000000000002220 ) ) ;
#31872 = CARTESIAN_POINT ( 'NONE',  ( 6.792576760808763936, -6.376774720514415407, 20.16775508794004779 ) ) ;
#31874 = ORIENTED_EDGE ( 'NONE', *, *, #75100, .T. ) ;
#31873 = CARTESIAN_POINT ( 'NONE',  ( -46.65381096568098229, -23.73791477778911840, 11.05961554403171299 ) ) ;
#31875 = ORIENTED_EDGE ( 'NONE', *, *, #42646, .F. ) ;
#31876 = LINE ( 'NONE', #92261, #96824 ) ;
#31877 = CARTESIAN_POINT ( 'NONE',  ( -112.6228709571500559, -23.47593901973091235, -1.443836447538999312 ) ) ;
#31878 = ORIENTED_EDGE ( 'NONE', *, *, #23941, .T. ) ;
#31879 = CARTESIAN_POINT ( 'NONE',  ( 15.93590435955092843, -13.91358336426615239, 11.49999999999998934 ) ) ;
#31880 = CARTESIAN_POINT ( 'NONE',  ( -117.6228709571500559, -29.50248528299804818, 1.056150453629045360 ) ) ;
#31881 = CARTESIAN_POINT ( 'NONE',  ( -62.62287095715004881, -24.64965695001468404, 8.947790433994185832 ) ) ;
#31882 = DIRECTION ( 'NONE',  ( -1.000000000000000000, -3.773278334444167608E-23, -8.201307833595939069E-29 ) ) ;
#31883 = DIRECTION ( 'NONE',  ( -3.773278334453079030E-23, 0.9999999999976377785, 2.173523156925979128E-06 ) ) ;
#31884 = CARTESIAN_POINT ( 'NONE',  ( -19.37210865224160017, -5.965225279485592225, -21.60955166348795586 ) ) ;
#31885 = CARTESIAN_POINT ( 'NONE',  ( -0.9539927174334467130, 22.11892580961223587, -1.500000000000002220 ) ) ;
#31886 = CARTESIAN_POINT ( 'NONE',  ( -8.119068529101312492, -10.01380310104339344, 1.305235352931652715 ) ) ;
#31887 = ORIENTED_EDGE ( 'NONE', *, *, #80354, .T. ) ;
#31888 = CARTESIAN_POINT ( 'NONE',  ( 6.437068816671457583, -5.965225279485592225, -28.37834077173919667 ) ) ;
#31889 = CARTESIAN_POINT ( 'NONE',  ( -64.62287095715007013, -23.95044443724992078, 10.65354141964650125 ) ) ;
#31890 = CARTESIAN_POINT ( 'NONE',  ( -40.29378138501845541, -25.30381737957640098, 5.537529357773589567 ) ) ;
#31891 = VECTOR ( 'NONE', #2843, 1000.000000000000000 ) ;
#31892 = DIRECTION ( 'NONE',  ( 3.773278334444167608E-23, -1.000000000000000000, 0.000000000000000000 ) ) ;
#31893 = DIRECTION ( 'NONE',  ( 0.000000000000000000, 0.000000000000000000, 1.000000000000000000 ) ) ;
#31894 = CARTESIAN_POINT ( 'NONE',  ( -19.46337940159461866, -0.4807646128305608779, 11.49999999999998934 ) ) ;
#31895 = CARTESIAN_POINT ( 'NONE',  ( -3.722501342491481235, -21.08806747394077519, -1.500000000000002220 ) ) ;
#31896 = CARTESIAN_POINT ( 'NONE',  ( 30.93860345374796594, 6.475225279485573360, 25.41160796525321430 ) ) ;
#31897 = CARTESIAN_POINT ( 'NONE',  ( -60.49711091220426340, -24.40133493613624083, 9.663955038888266458 ) ) ;
#31898 = CARTESIAN_POINT ( 'NONE',  ( -53.01255352321339842, 14.82721238576592704, 35.59556822165056644 ) ) ;
#31899 = CARTESIAN_POINT ( 'NONE',  ( -37.52287095715006870, -23.47593901973090524, -1.443836447538997314 ) ) ;
#31900 = CARTESIAN_POINT ( 'NONE',  ( 9.008567143757492346, 20.83016157428379955, -1.500000000000002220 ) ) ;
#31901 = AXIS2_PLACEMENT_3D ( 'NONE', #3760, #9349, #96103 ) ;
#31902 = CARTESIAN_POINT ( 'NONE',  ( -103.6228709571500985, -24.34917612406838572, 0.1852690917426675354 ) ) ;
#31903 = DIRECTION ( 'NONE',  ( 0.000000000000000000, 0.000000000000000000, -1.000000000000000000 ) ) ;
#31904 = CARTESIAN_POINT ( 'NONE',  ( -14.63867168220055781, -13.42826565525684579, 11.49999999999999645 ) ) ;
#31905 = CARTESIAN_POINT ( 'NONE',  ( 5.326923076923078426, -6.376774720514420736, 20.76772836538461320 ) ) ;
#31906 = EDGE_CURVE ( 'NONE', #45969, #49424, #13222, .T. ) ;
#31907 = VECTOR ( 'NONE', #36603, 1000.000000000000000 ) ;
#31908 = CARTESIAN_POINT ( 'NONE',  ( -115.5895376238167245, -23.47596703998600631, 11.44779298504227683 ) ) ;
#31909 = CARTESIAN_POINT ( 'NONE',  ( -98.52287095715006160, -23.47596703998600631, 11.44779298504228215 ) ) ;
#31910 = ORIENTED_EDGE ( 'NONE', *, *, #53502, .F. ) ;
#31911 = CARTESIAN_POINT ( 'NONE',  ( 30.51738178340319152, 4.795593857178634956, 19.84760796525322135 ) ) ;
#31912 = CARTESIAN_POINT ( 'NONE',  ( -6.680782769985652791, -5.876774720514411854, 19.46295461892502132 ) ) ;
#31913 = EDGE_CURVE ( 'NONE', #44056, #26199, #58628, .T. ) ;
#31914 = CARTESIAN_POINT ( 'NONE',  ( -75.55620429048340725, -24.99132157543166954, 2.256160258750667946 ) ) ;
#31915 = CARTESIAN_POINT ( 'NONE',  ( -20.21959982808627032, -7.803091810188320210, -1.500000000000002220 ) ) ;
#31916 = CARTESIAN_POINT ( 'NONE',  ( -56.49248187012878475, -24.51419770103157347, 9.386484678747180510 ) ) ;
#31918 = CIRCLE ( 'NONE', #96738, 1.530000000000002469 ) ;
#31917 = CARTESIAN_POINT ( 'NONE',  ( 16.96702763494397104, -9.608290155750392358, -1.500000000000002220 ) ) ;
#31919 = EDGE_CURVE ( 'NONE', #62364, #38339, #28813, .T. ) ;
#31920 = CARTESIAN_POINT ( 'NONE',  ( -65.62287095715005592, -29.50247984919015209, -1.443849546365055359 ) ) ;
#31921 = ORIENTED_EDGE ( 'NONE', *, *, #40680, .T. ) ;
#31922 = EDGE_CURVE ( 'NONE', #1781, #76018, #43410, .T. ) ;
#31923 = CARTESIAN_POINT ( 'NONE',  ( 16.53694760393551988, -11.94906295602464397, 11.49999999999999645 ) ) ;
#31924 = CARTESIAN_POINT ( 'NONE',  ( -80.58711764223190244, -24.63355581998386157, 0.9682620441943954326 ) ) ;
#31925 = EDGE_CURVE ( 'NONE', #72799, #83369, #23838, .T. ) ;
#31926 = LINE ( 'NONE', #54773, #1061 ) ;
#31927 = ORIENTED_EDGE ( 'NONE', *, *, #52288, .F. ) ;
#31928 = CARTESIAN_POINT ( 'NONE',  ( -0.09721816884246162194, -21.79143440635900220, 10.49653219292474482 ) ) ;
#31929 = CARTESIAN_POINT ( 'NONE',  ( 33.10022444407529463, 4.633339536272139902, -11.64480304263449106 ) ) ;
#31930 = CARTESIAN_POINT ( 'NONE',  ( -48.99007696559036162, -25.25214574776337528, 5.618156514524055289 ) ) ;
#31931 = CARTESIAN_POINT ( 'NONE',  ( -40.58148300679458487, -24.73531770709094957, 8.716586749053510275 ) ) ;
#31932 = CARTESIAN_POINT ( 'NONE',  ( -1.022535880784302353, -5.876774720514415407, 19.99258394656883908 ) ) ;
#31933 = CARTESIAN_POINT ( 'NONE',  ( 17.77915467781788195, 9.360003092772107181, -1.500000000000002220 ) ) ;
#31934 = PLANE ( 'NONE',  #80794 ) ;
#31935 = ORIENTED_EDGE ( 'NONE', *, *, #11464, .F. ) ;
#31936 = DIRECTION ( 'NONE',  ( -0.000000000000000000, -1.000000000000000000, -0.000000000000000000 ) ) ;
#31937 = AXIS2_PLACEMENT_3D ( 'NONE', #59086, #4294, #65714 ) ;
#31938 = CARTESIAN_POINT ( 'NONE',  ( -17.89994474767736676, -14.32179853049041363, 11.49999999999999645 ) ) ;
#31939 = CARTESIAN_POINT ( 'NONE',  ( 6.262736145392394427, -21.83385498489561272, 11.49999999999998934 ) ) ;
#31940 = ORIENTED_EDGE ( 'NONE', *, *, #3278, .T. ) ;
#31941 = CARTESIAN_POINT ( 'NONE',  ( -45.52287095715007581, -24.15431212366390668, -0.2830839119429377493 ) ) ;
#31942 = LINE ( 'NONE', #6599, #93306 ) ;
#31943 = FACE_OUTER_BOUND ( 'NONE', #8653, .T. ) ;
#31944 = VECTOR ( 'NONE', #9406, 1000.000000000000000 ) ;
#31945 = CARTESIAN_POINT ( 'NONE',  ( -30.57287095715005520, -25.00045060868233904, 2.199475715307360968 ) ) ;
#31946 = CARTESIAN_POINT ( 'NONE',  ( -128.6237108470990336, -24.35071581493544102, 9.817618358456018157 ) ) ;
#31947 = CARTESIAN_POINT ( 'NONE',  ( -58.56686834977553247, -23.48783264082477018, -1.443836473390093689 ) ) ;
#31948 = ORIENTED_EDGE ( 'NONE', *, *, #49612, .T. ) ;
#31949 = CARTESIAN_POINT ( 'NONE',  ( 18.38310620586021571, 8.829655622120887060, -1.500000000000002220 ) ) ;
#31950 = ORIENTED_EDGE ( 'NONE', *, *, #10588, .T. ) ;
#31951 = CARTESIAN_POINT ( 'NONE',  ( -5.582908757718670678, 22.30220962497079285, -1.500000000000002220 ) ) ;
#31952 = LINE ( 'NONE', #2016, #47028 ) ;
#31953 = LINE ( 'NONE', #16221, #25873 ) ;
#31954 = ORIENTED_EDGE ( 'NONE', *, *, #22910, .F. ) ;
#31955 = CARTESIAN_POINT ( 'NONE',  ( -114.5228709571500616, -24.51387760970725083, 9.387446482453398744 ) ) ;
#31956 = VECTOR ( 'NONE', #21755, 1000.000000000000000 ) ;
#31957 = CARTESIAN_POINT ( 'NONE',  ( 0.02224039135773677595, -0.3828044741864776723, -0.3828044741864797262 ) ) ;
#31959 = ORIENTED_EDGE ( 'NONE', *, *, #60526, .F. ) ;
#31958 = CARTESIAN_POINT ( 'NONE',  ( 1.434216325579209750, -21.26356369375713484, 11.49999999999999645 ) ) ;
#31960 = EDGE_LOOP ( 'NONE', ( #15001, #81754, #7989, #46929 ) ) ;
#31961 = CARTESIAN_POINT ( 'NONE',  ( -13.35739915041183323, 17.77566839534079435, -1.500000000000002220 ) ) ;
#31962 = CARTESIAN_POINT ( 'NONE',  ( 18.09409571311175569, -9.955296453752364272, 11.49999999999998934 ) ) ;
#31963 = ADVANCED_FACE ( 'NONE', ( #35790 ), #44405, .T. ) ;
#31964 = VECTOR ( 'NONE', #22928, 1000.000000000000114 ) ;
#31965 = ORIENTED_EDGE ( 'NONE', *, *, #64466, .T. ) ;
#31966 = CARTESIAN_POINT ( 'NONE',  ( -108.9567485977555634, -25.31627131983182721, 4.232820541622530186 ) ) ;
#31967 = EDGE_CURVE ( 'NONE', #10120, #11757, #75331, .T. ) ;
#31968 = FACE_OUTER_BOUND ( 'NONE', #87595, .T. ) ;
#31969 = ORIENTED_EDGE ( 'NONE', *, *, #74633, .T. ) ;
#31970 = FACE_OUTER_BOUND ( 'NONE', #4399, .T. ) ;
#31971 = VECTOR ( 'NONE', #21746, 1000.000000000000000 ) ;
#31972 = VERTEX_POINT ( 'NONE', #92057 ) ;
#31973 = DIRECTION ( 'NONE',  ( -3.773278334453079618E-23, 0.9999999999976377785, 2.173523156925979975E-06 ) ) ;
#31974 = B_SPLINE_CURVE_WITH_KNOTS ( 'NONE', 3,
 ( #90, #39145, #45272, #53884, #16308, #60997 ),
 .UNSPECIFIED., .F., .F.,
 ( 4, 2, 4 ),
 ( 0.000000000000000000, 0.001380764517854764098, 0.002761529035709528197 ),
 .UNSPECIFIED. ) ;
#31975 = CARTESIAN_POINT ( 'NONE',  ( 12.53797248504841910, 0.3587747205144256601, -28.12591401903467059 ) ) ;
#31976 = CARTESIAN_POINT ( 'NONE',  ( -0.6367455441941621830, -20.85161220577290919, -1.500000000000002220 ) ) ;
#31977 = CARTESIAN_POINT ( 'NONE',  ( 21.05697796394607835, 5.830696701215154043, 11.49999999999999645 ) ) ;
#31978 = DIRECTION ( 'NONE',  ( -0.000000000000000000, 1.000000000000000000, 0.000000000000000000 ) ) ;
#31979 = DIRECTION ( 'NONE',  ( 0.8813259582271224524, 0.000000000000000000, -0.4725087886537610027 ) ) ;
#31980 = CARTESIAN_POINT ( 'NONE',  ( 18.89768980500364037, -12.13386209897132773, 11.49999999999998934 ) ) ;
#31981 = CARTESIAN_POINT ( 'NONE',  ( -118.5210650335506699, -23.73791477778912551, 11.05961554403169878 ) ) ;
#31982 = CARTESIAN_POINT ( 'NONE',  ( -58.52287095715006870, -23.96127896941631974, -0.6493128931038022467 ) ) ;
#31983 = CARTESIAN_POINT ( 'NONE',  ( 4.885870204371583370, -5.876774720514420736, 20.85936027411790405 ) ) ;
#31984 = ORIENTED_EDGE ( 'NONE', *, *, #9163, .F. ) ;
#31985 = ORIENTED_EDGE ( 'NONE', *, *, #21599, .T. ) ;
#31986 = ORIENTED_EDGE ( 'NONE', *, *, #50384, .T. ) ;
#31987 = ORIENTED_EDGE ( 'NONE', *, *, #42038, .T. ) ;
#31988 = CARTESIAN_POINT ( 'NONE',  ( -19.74196057798672399, -8.316236533413031040, -1.500000000000002220 ) ) ;
#31989 = CARTESIAN_POINT ( 'NONE',  ( -18.60458529277170214, -12.42720982490441095, 11.49999999999999645 ) ) ;
#31990 = ORIENTED_EDGE ( 'NONE', *, *, #76209, .T. ) ;
#31991 = CARTESIAN_POINT ( 'NONE',  ( -20.97943885474387216, 2.004451313549292735, -1.500000000000002220 ) ) ;
#31992 = CARTESIAN_POINT ( 'NONE',  ( 4.667937696307308926, 1.310567935391715899, -2.677392948487098267E-15 ) ) ;
#31993 = CARTESIAN_POINT ( 'NONE',  ( 16.68016870136555596, 10.92824754362290385, -1.500000000000002220 ) ) ;
#31994 = CYLINDRICAL_SURFACE ( 'NONE', #69700, 1.149999999999998135 ) ;
#31995 = CARTESIAN_POINT ( 'NONE',  ( -43.52287095715006160, -23.48786465467240347, 11.44779295918255180 ) ) ;
#31996 = CARTESIAN_POINT ( 'NONE',  ( 19.49364837986538745, 10.19379059548657551, -1.500000000000002220 ) ) ;
#31997 = CARTESIAN_POINT ( 'NONE',  ( -6.720452724358975338, -5.876774720514411854, 19.46153846153846700 ) ) ;
#31998 = ORIENTED_EDGE ( 'NONE', *, *, #1446, .F. ) ;
#31999 = PLANE ( 'NONE',  #45363 ) ;
#32000 = CARTESIAN_POINT ( 'NONE',  ( -70.52287095715007581, -23.47593901973090524, -1.443836447538997092 ) ) ;
#32001 = CARTESIAN_POINT ( 'NONE',  ( -11.21968731015968856, -17.59241007644406096, 11.49999999999999645 ) ) ;
#32002 = AXIS2_PLACEMENT_3D ( 'NONE', #75772, #84394, #44848 ) ;
#32003 = LINE ( 'NONE', #54352, #13856 ) ;
#32004 = DIRECTION ( 'NONE',  ( -3.773278334453079618E-23, 0.9999999999976377785, 2.173523156925979975E-06 ) ) ;
#32005 = AXIS2_PLACEMENT_3D ( 'NONE', #73577, #88807, #18774 ) ;
#32006 = CARTESIAN_POINT ( 'NONE',  ( -90.55620429048339304, -25.00158670708909625, 2.256160236439166855 ) ) ;
#32007 = CARTESIAN_POINT ( 'NONE',  ( 5.124585555570928541, 20.71496159572455653, -1.500000000000002220 ) ) ;
#32008 = LINE ( 'NONE', #15776, #79045 ) ;
#32009 = CARTESIAN_POINT ( 'NONE',  ( -50.40445135320379677, -25.19502912051677868, 3.293943094755626078 ) ) ;
#32010 = CARTESIAN_POINT ( 'NONE',  ( -96.52287095715001897, -24.66019654487199730, 8.947790411086115725 ) ) ;
#32011 = CARTESIAN_POINT ( 'NONE',  ( -54.62287095715005592, -29.50248528299804818, 1.056150453629033370 ) ) ;
#32012 = CARTESIAN_POINT ( 'NONE',  ( 3.584315319034878211, 22.25550262085195286, -1.500000000000002220 ) ) ;
#32013 = DIRECTION ( 'NONE',  ( 0.000000000000000000, -0.9999999999976377785, -2.173523156925979975E-06 ) ) ;
#32014 = VERTEX_POINT ( 'NONE', #20543 ) ;
#32015 = LINE ( 'NONE', #32519, #82219 ) ;
#32016 = CARTESIAN_POINT ( 'NONE',  ( -68.22287095715010707, -23.47593901973090524, -1.443836447538997980 ) ) ;
#32017 = CARTESIAN_POINT ( 'NONE',  ( 3.778003860535555702, 19.31821889988591323, 11.49999999999999645 ) ) ;
#32018 = PLANE ( 'NONE',  #24413 ) ;
#32019 = DIRECTION ( 'NONE',  ( -1.000000000000000000, -3.773278334444166432E-23, -8.201307841325785021E-29 ) ) ;
#32020 = ORIENTED_EDGE ( 'NONE', *, *, #51359, .F. ) ;
#32021 = CARTESIAN_POINT ( 'NONE',  ( -111.5228709571500616, -24.33832256527048088, 0.1851278514138661180 ) ) ;
#32022 = CARTESIAN_POINT ( 'NONE',  ( 13.91401389203221406, 5.965225279485572685, 158.0376437107427137 ) ) ;
#32023 = CARTESIAN_POINT ( 'NONE',  ( -105.5228709571500758, -23.48786465467241769, 11.44779295918253936 ) ) ;
#32024 = VECTOR ( 'NONE', #14778, 1000.000000000000000 ) ;
#32025 = B_SPLINE_CURVE_WITH_KNOTS ( 'NONE', 3,
 ( #92596, #23074, #16468, #85994, #38814, #8370 ),
 .UNSPECIFIED., .F., .F.,
 ( 4, 2, 4 ),
 ( 0.000000000000000000, 0.001380901958385388545, 0.002761803916770777089 ),
 .UNSPECIFIED. ) ;
#32026 = CARTESIAN_POINT ( 'NONE',  ( -77.62287095715009855, -23.47596703998600631, 11.44779298504227683 ) ) ;
#32027 = CARTESIAN_POINT ( 'NONE',  ( 19.69962056004252560, 1.334664424591413434, -1.500000000000002220 ) ) ;
#32028 = ORIENTED_EDGE ( 'NONE', *, *, #45111, .F. ) ;
#32029 = EDGE_CURVE ( 'NONE', #32857, #27239, #44906, .T. ) ;
#32030 = CARTESIAN_POINT ( 'NONE',  ( 7.460719433876314532, 6.376774720514426953, -25.14146935902945046 ) ) ;
#32031 = ADVANCED_FACE ( 'NONE', ( #37283 ), #21043, .F. ) ;
#32032 = VECTOR ( 'NONE', #40330, 1000.000000000000000 ) ;
#32033 = APPROVAL_DATE_TIME ( #58266, #75393 ) ;
#32034 = VERTEX_POINT ( 'NONE', #51517 ) ;
#32035 = DIRECTION ( 'NONE',  ( 1.000000000000000000, 0.000000000000000000, 0.000000000000000000 ) ) ;
#32036 = CARTESIAN_POINT ( 'NONE',  ( -107.6228709571500985, -23.96127896941632685, -0.6493128931037773777 ) ) ;
#32037 = CARTESIAN_POINT ( 'NONE',  ( -70.35895856474229504, -25.30161620421289470, 5.313173632321669615 ) ) ;
#32038 = CARTESIAN_POINT ( 'NONE',  ( -99.52287095715006160, -29.50247984919015209, -1.443849546365050029 ) ) ;
#32039 = CARTESIAN_POINT ( 'NONE',  ( -85.62287095715004170, -23.48783264082478794, -1.443836473390063713 ) ) ;
#32040 = VECTOR ( 'NONE', #72466, 1000.000000000000000 ) ;
#32041 = DIRECTION ( 'NONE',  ( -1.000000000000000000, 0.000000000000000000, 0.000000000000000000 ) ) ;
#32042 = LINE ( 'NONE', #39148, #72150 ) ;
#32043 = CARTESIAN_POINT ( 'NONE',  ( -6.099057486122481997, -19.05896565686126110, -1.500000000000002220 ) ) ;
#32044 = ADVANCED_FACE ( 'NONE', ( #36290 ), #68234, .T. ) ;
#32045 = CARTESIAN_POINT ( 'NONE',  ( -58.62287095715004170, -23.72747288104442021, -1.053458166803663110 ) ) ;
#32046 = CARTESIAN_POINT ( 'NONE',  ( -24.97666371003640506, 0.3587747205143964613, -15.72894043976419454 ) ) ;
#32047 = ORIENTED_EDGE ( 'NONE', *, *, #48420, .F. ) ;
#32048 = DIRECTION ( 'NONE',  ( 0.000000000000000000, 0.000000000000000000, -1.000000000000000000 ) ) ;
#32049 = CARTESIAN_POINT ( 'NONE',  ( -65.05438548721848235, 3.316774720514426456, 29.49402280011861777 ) ) ;
#32050 = CARTESIAN_POINT ( 'NONE',  ( -35.60242693951278170, -24.15503026093914940, -0.2815557561904327155 ) ) ;
#32051 = CARTESIAN_POINT ( 'NONE',  ( -108.5228709571500758, -23.47593901973090524, -1.443836447538996204 ) ) ;
#32052 = CARTESIAN_POINT ( 'NONE',  ( -119.1722404401672577, -25.37154127157532102, 4.079011290487098762 ) ) ;
#32053 = CARTESIAN_POINT ( 'NONE',  ( -83.55852065756700142, -23.73766607897670511, -1.055555164236456900 ) ) ;
#32054 = CARTESIAN_POINT ( 'NONE',  ( -9.278253834636469577, -5.876774720514426953, 18.51871304725684553 ) ) ;
#32055 = CARTESIAN_POINT ( 'NONE',  ( -98.87653003804196317, -25.11539320716599732, 2.804431449967498491 ) ) ;
#32056 = VERTEX_POINT ( 'NONE', #29661 ) ;
#32057 = CARTESIAN_POINT ( 'NONE',  ( 0.7445296356392017145, -20.29553345556499622, 11.49999999999998934 ) ) ;
#32058 = CARTESIAN_POINT ( 'NONE',  ( 29.57907552799942508, 3.316774720514426456, 29.21818156447044501 ) ) ;
#32059 = VECTOR ( 'NONE', #84532, 1000.000000000000114 ) ;
#32060 = CARTESIAN_POINT ( 'NONE',  ( -59.59290457170049393, -24.15620529776628445, 10.23563542870661180 ) ) ;
#32061 = EDGE_LOOP ( 'NONE', ( #51287, #3589, #70679, #64457 ) ) ;
#32063 = EDGE_CURVE ( 'NONE', #47977, #6026, #5828, .T. ) ;
#32062 = CARTESIAN_POINT ( 'NONE',  ( 31.10870921191468597, -5.152774720514429418, -4.748485609378566785 ) ) ;
#32064 = CARTESIAN_POINT ( 'NONE',  ( -19.13055903301823335, -6.388282315271819556, -1.500000000000002220 ) ) ;
#32065 = CARTESIAN_POINT ( 'NONE',  ( -0.2625952501129409367, 21.13516572482953748, 11.49999999999999645 ) ) ;
#32066 = CARTESIAN_POINT ( 'NONE',  ( 0.7503028313155074569, 22.12739137992853955, 11.49999999999998934 ) ) ;
#32067 = EDGE_CURVE ( 'NONE', #63660, #67290, #76814, .T. ) ;
#32068 = CARTESIAN_POINT ( 'NONE',  ( 7.805751503010069037, -19.01748540344778959, -1.500000000000002220 ) ) ;
#32069 = CARTESIAN_POINT ( 'NONE',  ( 15.03220655128660255, 5.152774720514423201, -26.94699118253568315 ) ) ;
#32070 = ORIENTED_EDGE ( 'NONE', *, *, #34769, .T. ) ;
#32071 = DIRECTION ( 'NONE',  ( -3.773278334453079618E-23, 0.9999999999976377785, 2.173523156925979975E-06 ) ) ;
#32072 = ORIENTED_EDGE ( 'NONE', *, *, #31698, .T. ) ;
#32073 = DIRECTION ( 'NONE',  ( -1.000000000000000000, -9.637352644315600173E-17, 0.000000000000000000 ) ) ;
#32074 = CARTESIAN_POINT ( 'NONE',  ( -109.5228709571500616, -23.47596703998600631, 11.44779298504228038 ) ) ;
#32075 = EDGE_LOOP ( 'NONE', ( #29833, #53034, #30712, #77616, #38579, #74501, #79789, #30975 ) ) ;
#32076 = ORIENTED_EDGE ( 'NONE', *, *, #97324, .F. ) ;
#32077 = ORIENTED_EDGE ( 'NONE', *, *, #73998, .T. ) ;
#32078 = CARTESIAN_POINT ( 'NONE',  ( -111.0603964109058808, -25.15397636573018403, 3.025211319968325263 ) ) ;
#32079 = CARTESIAN_POINT ( 'NONE',  ( 6.963174204274080736, -5.876774720514415407, 20.29202897614545975 ) ) ;
#32080 = CARTESIAN_POINT ( 'NONE',  ( -68.54453206456847170, -24.35071581493542681, 9.817618358456032368 ) ) ;
#32081 = CARTESIAN_POINT ( 'NONE',  ( 16.32338804990218151, -12.73490195939593406, -1.500000000000002220 ) ) ;
#32082 = CARTESIAN_POINT ( 'NONE',  ( 20.80172415560569021, 6.174449132348904357, 11.49999999999999645 ) ) ;
#32083 = ORIENTED_EDGE ( 'NONE', *, *, #6185, .F. ) ;
#32084 = CARTESIAN_POINT ( 'NONE',  ( -8.160000000000000142, 8.793627758918228565, -2.994553991265763049 ) ) ;
#32085 = CARTESIAN_POINT ( 'NONE',  ( -4.141025641025642301, -6.376774720514411854, 19.63681891025641235 ) ) ;
#32086 = CARTESIAN_POINT ( 'NONE',  ( -13.97600220251353953, -17.46790257487896270, 11.49999999999998934 ) ) ;
#32087 = AXIS2_PLACEMENT_3D ( 'NONE', #83435, #12925, #52006 ) ;
#32088 = CARTESIAN_POINT ( 'NONE',  ( -47.62839470087014604, -24.51419770103156637, 9.386484678747176957 ) ) ;
#32089 = CARTESIAN_POINT ( 'NONE',  ( -101.5228709571500758, -23.47596703998600631, 11.44779298504228215 ) ) ;
#32090 = VERTEX_POINT ( 'NONE', #52012 ) ;
#32091 = CARTESIAN_POINT ( 'NONE',  ( -118.1689436852049226, -25.31364285773404887, 6.500980107507735362 ) ) ;
#32092 = CARTESIAN_POINT ( 'NONE',  ( -35.66629286559531664, -23.85049219812685095, 10.88485053497527488 ) ) ;
#32093 = ORIENTED_EDGE ( 'NONE', *, *, #52409, .F. ) ;
#32094 = LINE ( 'NONE', #16369, #26319 ) ;
#32095 = AXIS2_PLACEMENT_3D ( 'NONE', #23172, #7457, #47541 ) ;
#32096 = APPROVAL ( #69337, 'UNSPECIFIED' ) ;
#32097 = ORIENTED_EDGE ( 'NONE', *, *, #43162, .T. ) ;
#32098 = LINE ( 'NONE', #55958, #4987 ) ;
#32099 = CARTESIAN_POINT ( 'NONE',  ( 21.14167878903947084, -0.5806874866175276706, -1.500000000000002220 ) ) ;
#32100 = ORIENTED_EDGE ( 'NONE', *, *, #5944, .T. ) ;
#32101 = CARTESIAN_POINT ( 'NONE',  ( -50.53935553097652900, -24.52300882791529801, 0.6510814631126389251 ) ) ;
#32102 = CARTESIAN_POINT ( 'NONE',  ( -18.25314811174894913, -11.95880190493418738, 11.49999999999998934 ) ) ;
#32103 = CARTESIAN_POINT ( 'NONE',  ( -95.62287095715005592, -29.50249982740957577, 7.747779886224967605 ) ) ;
#32104 = AXIS2_PLACEMENT_3D ( 'NONE', #51275, #82217, #81725 ) ;
#32105 = CARTESIAN_POINT ( 'NONE',  ( -107.5228709571500616, -24.50216790748204332, 0.6166512839542614977 ) ) ;
#32106 = DIRECTION ( 'NONE',  ( 0.000000000000000000, 0.000000000000000000, 1.000000000000000000 ) ) ;
#32107 = CARTESIAN_POINT ( 'NONE',  ( -21.66901994843296819, -2.608494568651300138, -1.500000000000002220 ) ) ;
#32108 = CARTESIAN_POINT ( 'NONE',  ( -95.52287095715006160, -25.00158670708909980, 2.256160236439166411 ) ) ;
#32109 = VERTEX_POINT ( 'NONE', #29163 ) ;
#32110 = CARTESIAN_POINT ( 'NONE',  ( 7.433267315672343223, -5.876774720514418959, 20.43888261666079842 ) ) ;
#32111 = DIRECTION ( 'NONE',  ( -3.773278334453079030E-23, 0.9999999999976377785, 2.173523156925979128E-06 ) ) ;
#32112 = EDGE_LOOP ( 'NONE', ( #92903, #8626, #63235, #33329 ) ) ;
#32113 = EDGE_CURVE ( 'NONE', #6026, #34128, #11571, .T. ) ;
#32114 = CARTESIAN_POINT ( 'NONE',  ( -83.52287095715006160, -29.50248528299804818, 1.056150453629038477 ) ) ;
#32115 = B_SPLINE_CURVE_WITH_KNOTS ( 'NONE', 3,
 ( #41851, #65201, #80894, #26612 ),
 .UNSPECIFIED., .F., .F.,
 ( 4, 4 ),
 ( 0.08055752415614364503, 0.08956395542825920653 ),
 .UNSPECIFIED. ) ;
#32116 = VERTEX_POINT ( 'NONE', #76320 ) ;
#32117 = VECTOR ( 'NONE', #81721, 1000.000000000000000 ) ;
#32118 = ORIENTED_EDGE ( 'NONE', *, *, #76134, .T. ) ;
#32119 = CARTESIAN_POINT ( 'NONE',  ( -27.68651082257923335, -24.77145582263907286, 2.274903367125437281 ) ) ;
#32120 = CARTESIAN_POINT ( 'NONE',  ( -82.51746576141199796, -23.73766607897671577, -1.055555164236435362 ) ) ;
#32121 = CARTESIAN_POINT ( 'NONE',  ( 6.411417644607832145, 20.24884965431308714, -1.500000000000002220 ) ) ;
#32122 = CARTESIAN_POINT ( 'NONE',  ( -94.52217265877372654, -23.48783264082477018, -1.443836473390086805 ) ) ;
#32123 = CARTESIAN_POINT ( 'NONE',  ( -30.60993385648455956, -24.45056191361606679, 9.787827635114012992 ) ) ;
#32124 = PLANE ( 'NONE',  #58344 ) ;
#32125 = CARTESIAN_POINT ( 'NONE',  ( -65.05438548721848235, 6.475225279485573360, 0.7300228001186309656 ) ) ;
#32126 = CARTESIAN_POINT ( 'NONE',  ( -0.1161231997828221785, -19.40653004597026410, 11.49999999999998934 ) ) ;
#32127 = FACE_OUTER_BOUND ( 'NONE', #23317, .T. ) ;
#32128 = EDGE_LOOP ( 'NONE', ( #70904, #98328 ) ) ;
#32129 = CARTESIAN_POINT ( 'NONE',  ( -17.32436372870746055, -8.985247798433253053, 11.49999999999999645 ) ) ;
#32130 = CARTESIAN_POINT ( 'NONE',  ( -36.52287095715006870, -24.64898659630367916, 1.056161002820819261 ) ) ;
#32131 = EDGE_CURVE ( 'NONE', #11284, #19353, #81247, .T. ) ;
#32132 = CARTESIAN_POINT ( 'NONE',  ( -107.6228709571500701, -24.65952944569304961, 1.056160979905703901 ) ) ;
#32133 = VERTEX_POINT ( 'NONE', #22033 ) ;
#32134 = CARTESIAN_POINT ( 'NONE',  ( -103.6228709571500559, -23.47593901973091235, -1.443836447539001089 ) ) ;
#32135 = CARTESIAN_POINT ( 'NONE',  ( -113.6228709571500417, -23.47596703998600631, 11.44779298504227860 ) ) ;
#32136 = LINE ( 'NONE', #46874, #81186 ) ;
#32137 = CARTESIAN_POINT ( 'NONE',  ( -93.59740417728193052, -23.73791477778911840, 11.05961554403170410 ) ) ;
#32138 = CARTESIAN_POINT ( 'NONE',  ( -16.89733858281218204, -10.06102416988892934, 11.49999999999998934 ) ) ;
#32139 = B_SPLINE_SURFACE_WITH_KNOTS ( 'NONE', 3, 1, ( 
 ( #58847, #60358 ),
 ( #29883, #75047 ),
 ( #59339, #60852 ),
 ( #19762, #67458 ),
 ( #81682, #98383 ),
 ( #38992, #15154 ),
 ( #70453, #69449 ),
 ( #68948, #69944 ),
 ( #76538, #85672 ),
 ( #62863, #23762 ),
 ( #92276, #14654 ),
 ( #22753, #53737 ),
 ( #45618, #99872 ),
 ( #46120, #938 ),
 ( #61851, #30380 ),
 ( #8042, #9045 ),
 ( #37999, #77045 ),
 ( #47624, #22252 ),
 ( #93272, #39997 ) ),
 .UNSPECIFIED., .F., .F., .F.,
 ( 4, 1, 1, 1, 1, 1, 1, 1, 1, 1, 1, 1, 1, 1, 1, 1, 4 ),
 ( 2, 2 ),
 ( 0.000000000000000000, 0.05885358602866869876, 0.1163154589633517422, 0.1726748434114566133, 0.2287803868809005492, 0.2845803591252761278, 0.3402565063845458537, 0.3966298050124581476, 0.4535072628751937174, 0.5123181897799959916, 0.5726484440568331280, 0.6360219358218018870, 0.7023629463891940539, 0.7714830560569314599, 0.8441844774899029957, 0.9200697939721571572, 1.000000000000000000 ),
 ( 0.000000000000000000, 1.000000000000000000 ),
 .UNSPECIFIED. ) ;
#32140 = ORIENTED_EDGE ( 'NONE', *, *, #77702, .F. ) ;
#32141 = CARTESIAN_POINT ( 'NONE',  ( 21.52761780497506905, -1.784033869580059939, 11.49999999999998934 ) ) ;
#32142 = CARTESIAN_POINT ( 'NONE',  ( 0.2450472757604428842, -5.405843919193451086, 9.000000000000000000 ) ) ;
#32143 = CARTESIAN_POINT ( 'NONE',  ( -121.6228709571500417, -24.64898659630368627, 1.056161002820833028 ) ) ;
#32144 = CARTESIAN_POINT ( 'NONE',  ( -22.67921066581790868, 4.291001918001082771, -1.500000000000002220 ) ) ;
#32145 = EDGE_CURVE ( 'NONE', #38706, #46190, #59134, .T. ) ;
#32146 = B_SPLINE_CURVE_WITH_KNOTS ( 'NONE', 3,
 ( #20599, #91605, #37340, #66807 ),
 .UNSPECIFIED., .F., .F.,
 ( 4, 4 ),
 ( 0.7203002732715262368, 0.7293067045436417706 ),
 .UNSPECIFIED. ) ;
#32147 = APPLICATION_PROTOCOL_DEFINITION ( 'international standard', 'config_control_design', 1994, #80333 ) ;
#32148 = CARTESIAN_POINT ( 'NONE',  ( 3.036358173076929123, -6.376774720514420736, 20.87990785256409865 ) ) ;
#32149 = DIRECTION ( 'NONE',  ( -3.773278334453079030E-23, 0.9999999999976377785, 2.173523156925979128E-06 ) ) ;
#32150 = CARTESIAN_POINT ( 'NONE',  ( -121.5181176591963066, -24.66019654487200441, 8.947790411086119278 ) ) ;
#32151 = CARTESIAN_POINT ( 'NONE',  ( -64.62287095715005592, -24.51387760970723662, 9.387446482453425389 ) ) ;
#32152 = CARTESIAN_POINT ( 'NONE',  ( -111.1265005993262491, -25.29823862383007338, 3.068069378922468893 ) ) ;
#32153 = CARTESIAN_POINT ( 'NONE',  ( -124.5895376238167387, -23.48786465467241769, 11.44779295918253759 ) ) ;
#32154 = B_SPLINE_CURVE_WITH_KNOTS ( 'NONE', 3,
 ( #21281, #46016, #93163, #46507 ),
 .UNSPECIFIED., .F., .F.,
 ( 4, 4 ),
 ( 0.000000000000000000, 9.999999999998897304E-05 ),
 .UNSPECIFIED. ) ;
#32155 = CARTESIAN_POINT ( 'NONE',  ( -49.55620429048340014, -23.47593901973091235, -1.443836447539009749 ) ) ;
#32156 = CARTESIAN_POINT ( 'NONE',  ( -6.132916590032589710, 18.96384228413732842, 11.49999999999998934 ) ) ;
#32157 = ADVANCED_FACE ( 'NONE', ( #83948 ), #45403, .F. ) ;
#32158 = CARTESIAN_POINT ( 'NONE',  ( -75.57899585548300081, -25.00182538069147142, 7.747789668545045139 ) ) ;
#32159 = CARTESIAN_POINT ( 'NONE',  ( -15.51018552496569392, -12.33189742059753868, -1.500000000000002220 ) ) ;
#32160 = VERTEX_POINT ( 'NONE', #28671 ) ;
#32161 = AXIS2_PLACEMENT_3D ( 'NONE', #10575, #88710, #81593 ) ;
#32162 = CARTESIAN_POINT ( 'NONE',  ( 0.09189959430841809773, -5.876774720514410966, 19.67013632031035542 ) ) ;
#32163 = CARTESIAN_POINT ( 'NONE',  ( -39.89740106121153929, -25.29116539929970386, 2.930847754509050329 ) ) ;
#32164 = PLANE ( 'NONE',  #89658 ) ;
#32165 = CARTESIAN_POINT ( 'NONE',  ( -9.423985339279758122, -18.44656043379632848, 11.49999999999999645 ) ) ;
#32166 = DIRECTION ( 'NONE',  ( 0.000000000000000000, 0.000000000000000000, 1.000000000000000000 ) ) ;
#32167 = CARTESIAN_POINT ( 'NONE',  ( -40.62287095715004170, -24.99132157543083466, 2.256160258750667502 ) ) ;
#32168 = B_SPLINE_CURVE_WITH_KNOTS ( 'NONE', 3,
 ( #73066, #73556, #81666, #58342, #65967, #53221 ),
 .UNSPECIFIED., .F., .F.,
 ( 4, 2, 4 ),
 ( 6.391158118958419274E-06, 0.001387004593080783327, 0.002767618028042608501 ),
 .UNSPECIFIED. ) ;
#32169 = CARTESIAN_POINT ( 'NONE',  ( -15.20078144808659992, 16.97451310947862169, 11.49999999999999645 ) ) ;
#32170 = ORIENTED_EDGE ( 'NONE', *, *, #13469, .F. ) ;
#32171 = FACE_OUTER_BOUND ( 'NONE', #69309, .T. ) ;
#32172 = CARTESIAN_POINT ( 'NONE',  ( -69.47493225014638085, -25.19029820154286980, 6.676482576448054651 ) ) ;
#32173 = ORIENTED_EDGE ( 'NONE', *, *, #73825, .F. ) ;
#32174 = AXIS2_PLACEMENT_3D ( 'NONE', #28807, #21185, #14575 ) ;
#32175 = CARTESIAN_POINT ( 'NONE',  ( -0.5548696950099620828, -20.20177982057877841, -1.500000000000002220 ) ) ;
#32176 = LINE ( 'NONE', #63149, #3093 ) ;
#32177 = CARTESIAN_POINT ( 'NONE',  ( -49.52287095715006160, -24.65952944569304606, 1.056160979905693686 ) ) ;
#32178 = ORIENTED_EDGE ( 'NONE', *, *, #60820, .T. ) ;
#32179 = LINE ( 'NONE', #46915, #25791 ) ;
#32180 = CARTESIAN_POINT ( 'NONE',  ( -17.45619364963476627, 14.87644265977633573, -1.500000000000002220 ) ) ;
#32181 = CARTESIAN_POINT ( 'NONE',  ( -41.72781200478040375, -25.23288469818084678, 3.583692438795834434 ) ) ;
#32182 = CARTESIAN_POINT ( 'NONE',  ( -3.121018476474317183, -19.76494895549465980, -1.500000000000002220 ) ) ;
#32183 = VECTOR ( 'NONE', #40171, 1000.000000000000000 ) ;
#32184 = CARTESIAN_POINT ( 'NONE',  ( -36.62287095715005592, -24.64965695001467694, 8.947790433994187609 ) ) ;
#32185 = CARTESIAN_POINT ( 'NONE',  ( -20.97355972163249049, 0.1317905507124840780, 11.49999999999999645 ) ) ;
#32186 = CARTESIAN_POINT ( 'NONE',  ( -86.62287095715001328, -24.50321055353805377, 9.387540953477522265 ) ) ;
#32187 = CARTESIAN_POINT ( 'NONE',  ( -124.5915507283297217, -23.48783264082478084, -1.443836473390086361 ) ) ;
#32188 = CARTESIAN_POINT ( 'NONE',  ( -21.92701646642465008, -2.088449908657787457, 11.49999999999998934 ) ) ;
#32189 = DIRECTION ( 'NONE',  ( 0.000000000000000000, 1.000000000000000000, 0.000000000000000000 ) ) ;
#32191 = EDGE_LOOP ( 'NONE', ( #12605, #49867, #38094, #83238 ) ) ;
#32190 = ADVANCED_FACE ( 'NONE', ( #7313 ), #82942, .F. ) ;
#32192 = DIRECTION ( 'NONE',  ( 0.9762960071199348056, 0.2164396139380966033, 0.000000000000000000 ) ) ;
#32193 = FACE_OUTER_BOUND ( 'NONE', #69599, .T. ) ;
#32194 = ORIENTED_EDGE ( 'NONE', *, *, #35701, .F. ) ;
#32195 = CARTESIAN_POINT ( 'NONE',  ( 22.81105451610979173, -1.684774720501991396, -18.46691820600746681 ) ) ;
#32196 = ORIENTED_EDGE ( 'NONE', *, *, #54068, .F. ) ;
#32197 = ORIENTED_EDGE ( 'NONE', *, *, #69521, .F. ) ;
#32198 = CARTESIAN_POINT ( 'NONE',  ( 0.000000000000000000, -6.943225279485572443, -1.149999999999999911 ) ) ;
#32199 = CARTESIAN_POINT ( 'NONE',  ( -2.701720430790311767, -5.965225279485594001, -28.90526747363640681 ) ) ;
#32200 = LINE ( 'NONE', #47441, #19562 ) ;
#32201 = CARTESIAN_POINT ( 'NONE',  ( 17.38039551199336685, -10.77953091123627694, -1.500000000000002220 ) ) ;
#32202 = B_SPLINE_CURVE_WITH_KNOTS ( 'NONE', 3,
 ( #94337, #17215, #92447, #32951 ),
 .UNSPECIFIED., .F., .F.,
 ( 4, 4 ),
 ( 0.000000000000000000, 0.0001000000000000028644 ),
 .UNSPECIFIED. ) ;
#32203 = ORIENTED_EDGE ( 'NONE', *, *, #28611, .T. ) ;
#32204 = CARTESIAN_POINT ( 'NONE',  ( -79.52287095715010423, -23.72747288104470087, -1.053458166803226792 ) ) ;
#32205 = CARTESIAN_POINT ( 'NONE',  ( -10.30858931494281450, 5.088649829473331110, 28.47370074478044444 ) ) ;
#32206 = CARTESIAN_POINT ( 'NONE',  ( 8.971512145086530055, -9.528487854913503696, 1.500000000000002220 ) ) ;
#32207 = CARTESIAN_POINT ( 'NONE',  ( -8.840690135214121170, 20.45858245768130956, 11.49999999999998934 ) ) ;
#32208 = B_SPLINE_CURVE_WITH_KNOTS ( 'NONE', 3,
 ( #5064, #59357, #66000, #88314 ),
 .UNSPECIFIED., .F., .F.,
 ( 4, 4 ),
 ( 0.3900644599606266083, 0.3990708912327424196 ),
 .UNSPECIFIED. ) ;
#32209 = CARTESIAN_POINT ( 'NONE',  ( -70.38567012983610027, -25.13346044137653124, 7.099803150338960478 ) ) ;
#32210 = CARTESIAN_POINT ( 'NONE',  ( -88.62287095715004170, -23.48786465467241769, 11.44779295918254114 ) ) ;
#32211 = ORIENTED_EDGE ( 'NONE', *, *, #27628, .T. ) ;
#32212 = CARTESIAN_POINT ( 'NONE',  ( -103.6228709571500559, -29.50247984919015209, -1.443849546365050029 ) ) ;
#32213 = CARTESIAN_POINT ( 'NONE',  ( -118.5228709571500758, -24.64898659630368627, 1.056161002820833028 ) ) ;
#32214 = CARTESIAN_POINT ( 'NONE',  ( -19.76906661924035191, -6.534152953431121347, 11.49999999999998934 ) ) ;
#32215 = ORIENTED_EDGE ( 'NONE', *, *, #78973, .T. ) ;
#32217 = ORIENTED_EDGE ( 'NONE', *, *, #21128, .F. ) ;
#32216 = DIRECTION ( 'NONE',  ( 0.9831680378442393398, 0.000000000000000000, 0.1827036106964188000 ) ) ;
#32218 = EDGE_CURVE ( 'NONE', #77901, #81257, #78286, .T. ) ;
#32219 = EDGE_LOOP ( 'NONE', ( #30005, #62025, #96011, #7014 ) ) ;
#32220 = CARTESIAN_POINT ( 'NONE',  ( -50.99155954085787812, -25.12217837880228188, 6.987757997958206069 ) ) ;
#32221 = CARTESIAN_POINT ( 'NONE',  ( -19.40065202112720755, 8.109199488025859992, -1.500000000000002220 ) ) ;
#32222 = EDGE_LOOP ( 'NONE', ( #62296, #51441, #25266, #53614 ) ) ;
#32223 = FACE_OUTER_BOUND ( 'NONE', #50196, .T. ) ;
#32224 = AXIS2_PLACEMENT_3D ( 'NONE', #60904, #43180, #60411 ) ;
#32225 = CARTESIAN_POINT ( 'NONE',  ( -9.940598223437577374, -5.876774720514426953, 22.08128695274315945 ) ) ;
#32226 = CARTESIAN_POINT ( 'NONE',  ( 7.227401621296005274, -3.316774720515020203, -27.22638491047315767 ) ) ;
#32227 = ADVANCED_FACE ( 'NONE', ( #67748 ), #45897, .T. ) ;
#32228 = AXIS2_PLACEMENT_3D ( 'NONE', #82667, #29379, #83663 ) ;
#32229 = CARTESIAN_POINT ( 'NONE',  ( -86.51068774892489444, -24.15620529776628445, 10.23563542870660292 ) ) ;
#32230 = CARTESIAN_POINT ( 'NONE',  ( -60.62287095715002039, -24.82576562982391621, 8.398263435472967942 ) ) ;
#32231 = CARTESIAN_POINT ( 'NONE',  ( -65.62287095715007013, -24.52323809116985132, 9.355190652339423707 ) ) ;
#32233 = ORIENTED_EDGE ( 'NONE', *, *, #53751, .F. ) ;
#32232 = CARTESIAN_POINT ( 'NONE',  ( 22.14152233036116257, 1.636640089565777334, 11.49999999999999645 ) ) ;
#32234 = CARTESIAN_POINT ( 'NONE',  ( -20.77875734969026311, -3.316774720514426456, 29.49402280011862487 ) ) ;
#32235 = CARTESIAN_POINT ( 'NONE',  ( -54.52287095715006870, -24.64898659630367916, 1.056161002820821038 ) ) ;
#32236 = VERTEX_POINT ( 'NONE', #24540 ) ;
#32237 = CARTESIAN_POINT ( 'NONE',  ( -12.01393383709116947, -19.22582291892495121, 11.49999999999998934 ) ) ;
#32238 = EDGE_CURVE ( 'NONE', #5385, #19525, #83147, .T. ) ;
#32239 = CIRCLE ( 'NONE', #24125, 251.4258649670780699 ) ;
#32240 = EDGE_CURVE ( 'NONE', #93259, #68647, #54012, .T. ) ;
#32242 = ORIENTED_EDGE ( 'NONE', *, *, #89842, .T. ) ;
#32241 = CARTESIAN_POINT ( 'NONE',  ( 22.02124265030973760, 7.743225279485574042, 13.95402280011862395 ) ) ;
#32243 = ORIENTED_EDGE ( 'NONE', *, *, #60074, .F. ) ;
#32244 = ADVANCED_FACE ( 'NONE', ( #70725 ), #31653, .F. ) ;
#32245 = AXIS2_PLACEMENT_3D ( 'NONE', #59264, #66890, #44033 ) ;
#32246 = LINE ( 'NONE', #1808, #83721 ) ;
#32247 = CARTESIAN_POINT ( 'NONE',  ( 20.05498121024909253, 1.910150955369836812, -1.500000000000002220 ) ) ;
#32248 = CARTESIAN_POINT ( 'NONE',  ( 32.53135143123563466, -5.965225279485572685, 6.926385399448451885 ) ) ;
#32249 = ORIENTED_EDGE ( 'NONE', *, *, #58304, .F. ) ;
#32250 = AXIS2_PLACEMENT_3D ( 'NONE', #76221, #27332, #3011 ) ;
#32252 = B_SPLINE_CURVE_WITH_KNOTS ( 'NONE', 3,
 ( #55065, #63183, #87508, #17993 ),
 .UNSPECIFIED., .F., .F.,
 ( 4, 4 ),
 ( 0.000000000000000000, 9.999999999998897304E-05 ),
 .UNSPECIFIED. ) ;
#32251 = DIRECTION ( 'NONE',  ( -0.9994733861282923959, -0.000000000000000000, -0.03244919754393515293 ) ) ;
#32253 = CARTESIAN_POINT ( 'NONE',  ( -20.38924965233672282, -9.335317855073830273, -1.500000000000002220 ) ) ;
#32254 = ADVANCED_FACE ( 'NONE', ( #23525 ), #50749, .T. ) ;
#32255 = VERTEX_POINT ( 'NONE', #86944 ) ;
#32256 = VERTEX_POINT ( 'NONE', #31155 ) ;
#32257 = CARTESIAN_POINT ( 'NONE',  ( -112.5504983259648384, -24.66019654487200086, 8.947790411086112172 ) ) ;
#32258 = CARTESIAN_POINT ( 'NONE',  ( -94.59133804672956103, -24.15620529776628089, 10.23563542870660470 ) ) ;
#32259 = CARTESIAN_POINT ( 'NONE',  ( -70.62287095715005592, -29.50248528299804818, 1.056150453629036701 ) ) ;
#32260 = DIRECTION ( 'NONE',  ( 0.000000000000000000, -1.000000000000000000, 0.000000000000000000 ) ) ;
#32261 = CARTESIAN_POINT ( 'NONE',  ( -71.70841769935766763, -25.24715640642683923, 6.192981443001071895 ) ) ;
#32262 = CARTESIAN_POINT ( 'NONE',  ( -19.30006219055749739, -3.230038287793697283, 11.49999999999998934 ) ) ;
#32263 = CARTESIAN_POINT ( 'NONE',  ( -5.023036858974361252, -5.876774720514410077, 19.14743589743590846 ) ) ;
#32264 = ORIENTED_EDGE ( 'NONE', *, *, #47520, .F. ) ;
#32265 = CARTESIAN_POINT ( 'NONE',  ( 16.66814584454133907, -13.58961022886752978, 11.49999999999998934 ) ) ;
#32266 = CARTESIAN_POINT ( 'NONE',  ( -2.794793911895765870, -6.376774720514417183, 20.33046051580616265 ) ) ;
#32267 = CARTESIAN_POINT ( 'NONE',  ( -19.69812919673063689, 0.3587747205143964613, -22.00173861453436430 ) ) ;
#32268 = CARTESIAN_POINT ( 'NONE',  ( -113.5228709571500758, -24.51387760970726504, 9.387446482453402297 ) ) ;
#32269 = CARTESIAN_POINT ( 'NONE',  ( -70.62287095715005592, -25.00182538069145011, 7.747789668545097541 ) ) ;
#32270 = CARTESIAN_POINT ( 'NONE',  ( 20.38051395842347802, -10.57019977742728578, -1.500000000000002220 ) ) ;
#32271 = ADVANCED_FACE ( 'NONE', ( #38766 ), #79328, .T. ) ;
#32272 = VECTOR ( 'NONE', #33785, 1000.000000000000114 ) ;
#32273 = EDGE_CURVE ( 'NONE', #73900, #21630, #37141, .T. ) ;
#32274 = PERSON_AND_ORGANIZATION ( #70597, #27821 ) ;
#32275 = FACE_OUTER_BOUND ( 'NONE', #2394, .T. ) ;
#32276 = CARTESIAN_POINT ( 'NONE',  ( -92.62287095715005592, -24.64898659630368627, 1.056161002820827921 ) ) ;
#32277 = CARTESIAN_POINT ( 'NONE',  ( -13.93161493328335432, -14.37010051631055418, 11.49999999999999645 ) ) ;
#32278 = LINE ( 'NONE', #23145, #4098 ) ;
#32279 = DIRECTION ( 'NONE',  ( -1.000000000000000000, 0.000000000000000000, -0.000000000000000000 ) ) ;
#32280 = CARTESIAN_POINT ( 'NONE',  ( 4.967948717948723392, -5.876774720514415407, 20.00140224358974095 ) ) ;
#32281 = LINE ( 'NONE', #331, #1876 ) ;
#32282 = ORIENTED_EDGE ( 'NONE', *, *, #47135, .T. ) ;
#32283 = CARTESIAN_POINT ( 'NONE',  ( -50.62287095715005592, -23.85229601348995487, 10.88205029486209341 ) ) ;
#32284 = EDGE_CURVE ( 'NONE', #26504, #84981, #15507, .T. ) ;
#32285 = CARTESIAN_POINT ( 'NONE',  ( 5.219777686717518961, -21.12652377152128480, 11.49999999999998934 ) ) ;
#32286 = FACE_OUTER_BOUND ( 'NONE', #89354, .T. ) ;
#32287 = CARTESIAN_POINT ( 'NONE',  ( 0.7877182283408599162, 19.66719298131377514, -1.500000000000002220 ) ) ;
#32288 = DIRECTION ( 'NONE',  ( -1.000000000000000000, 0.000000000000000000, -0.000000000000000000 ) ) ;
#32289 = EDGE_CURVE ( 'NONE', #21092, #45475, #19108, .T. ) ;
#32290 = EDGE_CURVE ( 'NONE', #39981, #56283, #97057, .T. ) ;
#32291 = CARTESIAN_POINT ( 'NONE',  ( -109.7735670026218173, -25.31698141328030260, 5.109898621226075299 ) ) ;
#32292 = DATE_AND_TIME ( #1357, #28039 ) ;
#32293 = CARTESIAN_POINT ( 'NONE',  ( -91.50434982067550038, -24.66019654487199730, 8.947790411086115725 ) ) ;
#32294 = CARTESIAN_POINT ( 'NONE',  ( 13.91401389203221406, -6.475225279485573360, 158.0376437107427137 ) ) ;
#32295 = CARTESIAN_POINT ( 'NONE',  ( -17.31529204923715071, 11.11782870402162260, 11.49999999999999645 ) ) ;
#32296 = CARTESIAN_POINT ( 'NONE',  ( 4.487249349319938574, -6.376774720514420736, 21.01618089687719504 ) ) ;
#32297 = CARTESIAN_POINT ( 'NONE',  ( -120.5177549675304647, -24.63355581998386157, 0.9682620441943888823 ) ) ;
#32298 = CARTESIAN_POINT ( 'NONE',  ( -8.787219534579676861, -20.84281209399103929, 11.49999999999999645 ) ) ;
#32299 = VERTEX_POINT ( 'NONE', #35171 ) ;
#32300 = CARTESIAN_POINT ( 'NONE',  ( -46.62287095715004170, -23.73907113216991860, -1.053371485793232587 ) ) ;
#32301 = LINE ( 'NONE', #9966, #36458 ) ;
#32302 = CARTESIAN_POINT ( 'NONE',  ( -125.5903894658442255, -24.15602025860897584, 10.28564288303534013 ) ) ;
#32303 = CARTESIAN_POINT ( 'NONE',  ( 31.55236408230781819, 5.965225279485572685, 19.84760796525321780 ) ) ;
#32304 = AXIS2_PLACEMENT_3D ( 'NONE', #80678, #58848, #3567 ) ;
#32305 = CARTESIAN_POINT ( 'NONE',  ( -25.59878527050454622, -24.61459625492054215, 6.005086935496544598 ) ) ;
#32306 = CARTESIAN_POINT ( 'NONE',  ( -41.62287095715006302, -24.66019654487199020, 8.947790411086135265 ) ) ;
#32307 = AXIS2_PLACEMENT_3D ( 'NONE', #86881, #79263, #87383 ) ;
#32308 = ORIENTED_EDGE ( 'NONE', *, *, #7281, .T. ) ;
#32309 = CARTESIAN_POINT ( 'NONE',  ( -79.36292229018619082, -25.31596392387344352, 5.750285860338011368 ) ) ;
#32310 = CARTESIAN_POINT ( 'NONE',  ( 16.54545882101025711, 15.75737887292823558, -1.500000000000002220 ) ) ;
#32311 = CARTESIAN_POINT ( 'NONE',  ( -104.5228709571500758, -24.50216790748206108, 0.6166512839542541702 ) ) ;
#32312 = AXIS2_PLACEMENT_3D ( 'NONE', #55413, #8229, #93448 ) ;
#32313 = CARTESIAN_POINT ( 'NONE',  ( -115.5228709571500758, -24.14406661686763655, 10.28769366194076795 ) ) ;
#32314 = CARTESIAN_POINT ( 'NONE',  ( -63.61015071180399616, -23.48786465467241413, 11.44779295918254824 ) ) ;
#32315 = CARTESIAN_POINT ( 'NONE',  ( 18.89768980500364037, -12.13386209897132773, 11.49999999999999645 ) ) ;
#32316 = ORIENTED_EDGE ( 'NONE', *, *, #21124, .F. ) ;
#32317 = VECTOR ( 'NONE', #12094, 1000.000000000000000 ) ;
#32318 = DIRECTION ( 'NONE',  ( -3.773278334453079618E-23, 0.9999999999976377785, 2.173523156925979975E-06 ) ) ;
#32319 = CARTESIAN_POINT ( 'NONE',  ( -19.17877449816284496, 10.63638241594707345, -1.500000000000002220 ) ) ;
#32320 = CARTESIAN_POINT ( 'NONE',  ( -5.457842845122470976, -6.376774720514411854, 19.25892998154168367 ) ) ;
#32322 = CARTESIAN_POINT ( 'NONE',  ( -44.64054216518013618, -24.15620529776627734, 10.23563542870660470 ) ) ;
#32321 = AXIS2_PLACEMENT_3D ( 'NONE', #78766, #72189, #56971 ) ;
#32323 = DIRECTION ( 'NONE',  ( 0.000000000000000000, -1.000000000000000000, 0.000000000000000000 ) ) ;
#32324 = ORIENTED_EDGE ( 'NONE', *, *, #6230, .F. ) ;
#32325 = CARTESIAN_POINT ( 'NONE',  ( -112.6228709571500701, -23.48786465467241769, 11.44779295918254114 ) ) ;
#32326 = LINE ( 'NONE', #79499, #20307 ) ;
#32327 = VERTEX_POINT ( 'NONE', #81834 ) ;
#32328 = CARTESIAN_POINT ( 'NONE',  ( -0.3173379506236611580, 20.48240526196808631, 11.49999999999998934 ) ) ;
#32329 = ORIENTED_EDGE ( 'NONE', *, *, #43718, .T. ) ;
#32330 = ORIENTED_EDGE ( 'NONE', *, *, #22731, .T. ) ;
#32331 = ORIENTED_EDGE ( 'NONE', *, *, #53877, .F. ) ;
#32332 = ORIENTED_EDGE ( 'NONE', *, *, #79863, .F. ) ;
#32333 = CARTESIAN_POINT ( 'NONE',  ( -14.58522200957802184, -17.87834940746265389, 11.49999999999998934 ) ) ;
#32334 = LINE ( 'NONE', #94729, #60071 ) ;
#32335 = CARTESIAN_POINT ( 'NONE',  ( -20.07547297788957152, 3.163885811906596679, -1.500000000000002220 ) ) ;
#32336 = ORIENTED_EDGE ( 'NONE', *, *, #12411, .T. ) ;
#32337 = CARTESIAN_POINT ( 'NONE',  ( -50.62287095715005592, -29.50250243563736774, 8.947779886222146928 ) ) ;
#32338 = CARTESIAN_POINT ( 'NONE',  ( -72.52287095715007581, -23.47593901973090169, -1.443836447538996870 ) ) ;
#32339 = CARTESIAN_POINT ( 'NONE',  ( -101.5115004759412187, -25.24062753727274355, 6.352195226156559293 ) ) ;
#32340 = CARTESIAN_POINT ( 'NONE',  ( 4.572862496014544753, -6.376774720514408301, 19.20224321281611068 ) ) ;
#32342 = ORIENTED_EDGE ( 'NONE', *, *, #12441, .T. ) ;
#32341 = CARTESIAN_POINT ( 'NONE',  ( -15.31780299886000485, -15.04297462106122474, 11.49999999999999645 ) ) ;
#32343 = CARTESIAN_POINT ( 'NONE',  ( -75.60360656315280892, -23.85016227208580730, -0.8807180028928284221 ) ) ;
#32344 = CARTESIAN_POINT ( 'NONE',  ( -104.6228709571500985, -24.33832256526968862, 0.1851278514119912566 ) ) ;
#32345 = VERTEX_POINT ( 'NONE', #49907 ) ;
#32346 = CARTESIAN_POINT ( 'NONE',  ( 18.38559056850662543, 9.607341378227904016, -1.500000000000002220 ) ) ;
#32347 = ORIENTED_EDGE ( 'NONE', *, *, #50736, .F. ) ;
#32349 = EDGE_LOOP ( 'NONE', ( #1882, #96805, #35131, #34727 ) ) ;
#32348 = LINE ( 'NONE', #70926, #94461 ) ;
#32350 = ADVANCED_FACE ( 'NONE', ( #79826 ), #27559, .T. ) ;
#32351 = CARTESIAN_POINT ( 'NONE',  ( -111.5588673000302293, -23.48786465467241769, 11.44779295918254114 ) ) ;
#32352 = CARTESIAN_POINT ( 'NONE',  ( -57.52287095715005449, -29.50250243563736774, 8.947779886222145151 ) ) ;
#32353 = ORIENTED_EDGE ( 'NONE', *, *, #62859, .T. ) ;
#32354 = ORIENTED_EDGE ( 'NONE', *, *, #33564, .T. ) ;
#32355 = ADVANCED_FACE ( 'NONE', ( #19925 ), #3237, .F. ) ;
#32356 = CARTESIAN_POINT ( 'NONE',  ( 0.000000000000000000, -5.356774720514425603, 0.000000000000000000 ) ) ;
#32357 = CARTESIAN_POINT ( 'NONE',  ( -125.6228709571500559, -24.99132157543083821, 2.256160258750667502 ) ) ;
#32358 = CARTESIAN_POINT ( 'NONE',  ( -29.26457644120217338, -24.94536068527088091, 2.458381786851871365 ) ) ;
#32359 = CARTESIAN_POINT ( 'NONE',  ( -19.13726171168348245, 10.91495894028074432, 11.49999999999999645 ) ) ;
#32360 = EDGE_CURVE ( 'NONE', #19500, #95501, #5808, .T. ) ;
#32361 = CARTESIAN_POINT ( 'NONE',  ( -89.64225548740091654, -23.48786465467241058, 11.44779295918254114 ) ) ;
#32362 = CARTESIAN_POINT ( 'NONE',  ( -13.16310354753345990, -18.33534949228788236, -1.500000000000002220 ) ) ;
#32363 = EDGE_CURVE ( 'NONE', #21350, #67214, #50894, .T. ) ;
#32364 = CARTESIAN_POINT ( 'NONE',  ( 17.94697546605861760, -10.91086909363634838, -1.500000000000002220 ) ) ;
#32365 = ADVANCED_FACE ( 'NONE', ( #95062 ), #87447, .T. ) ;
#32367 = ORIENTED_EDGE ( 'NONE', *, *, #72374, .F. ) ;
#32366 = CARTESIAN_POINT ( 'NONE',  ( 2.230654205607476737, -2.168404344971008868E-16, 0.1647943925233645579 ) ) ;
#32368 = ORIENTED_EDGE ( 'NONE', *, *, #89197, .F. ) ;
#32369 = EDGE_CURVE ( 'NONE', #34608, #40266, #10827, .T. ) ;
#32370 = CARTESIAN_POINT ( 'NONE',  ( 0.03625801282051022839, -6.376774720514410077, 19.27714342948718240 ) ) ;
#32371 = CIRCLE ( 'NONE', #61569, 0.5999999999999998668 ) ;
#32372 = CARTESIAN_POINT ( 'NONE',  ( -7.749999999999996447, 25.69999999999999574, 0.000000000000000000 ) ) ;
#32373 = ORIENTED_EDGE ( 'NONE', *, *, #7207, .F. ) ;
#32374 = CARTESIAN_POINT ( 'NONE',  ( 18.68757921870947669, -9.911485057863893999, 11.49999999999998934 ) ) ;
#32375 = DIRECTION ( 'NONE',  ( -0.06283980576413537855, -0.000000000000000000, -0.9980236263794188822 ) ) ;
#32376 = CARTESIAN_POINT ( 'NONE',  ( -51.92774333234893192, -25.26040843124357238, 6.302625152703366318 ) ) ;
#32378 = CARTESIAN_POINT ( 'NONE',  ( -121.5908097599731548, -23.96119346886880663, -0.6495511937832033622 ) ) ;
#32377 = AXIS2_PLACEMENT_3D ( 'NONE', #40186, #41192, #8233 ) ;
#32379 = FACE_OUTER_BOUND ( 'NONE', #49060, .T. ) ;
#32380 = LINE ( 'NONE', #94272, #22730 ) ;
#32381 = CARTESIAN_POINT ( 'NONE',  ( 19.22371909900314435, 11.20011194808016342, -1.500000000000002220 ) ) ;
#32382 = CARTESIAN_POINT ( 'NONE',  ( -49.72218425784361528, -25.13941470960068969, 7.443037641556777828 ) ) ;
#32383 = EDGE_CURVE ( 'NONE', #24606, #65803, #47357, .T. ) ;
#32384 = ORIENTED_EDGE ( 'NONE', *, *, #46800, .T. ) ;
#32385 = CARTESIAN_POINT ( 'NONE',  ( 11.54156857142115911, 3.316774720514427344, -28.05134709678029381 ) ) ;
#32386 = CARTESIAN_POINT ( 'NONE',  ( -37.54586441416935827, -24.15543982623907127, -0.2315651400026566831 ) ) ;
#32387 = CARTESIAN_POINT ( 'NONE',  ( -43.62287095715004881, -23.73907113216990439, -1.053371485793232587 ) ) ;
#32388 = AXIS2_PLACEMENT_3D ( 'NONE', #98866, #69807, #93128 ) ;
#32389 = CARTESIAN_POINT ( 'NONE',  ( -100.5064038502849115, -24.83618233451451118, 1.606449574219533050 ) ) ;
#32390 = CARTESIAN_POINT ( 'NONE',  ( 14.76093561896379214, -5.965225279485572685, -26.55548769130089681 ) ) ;
#32391 = EDGE_CURVE ( 'NONE', #81403, #20070, #48900, .T. ) ;
#32392 = CIRCLE ( 'NONE', #45367, 2.249999999999998668 ) ;
#32393 = CARTESIAN_POINT ( 'NONE',  ( 8.918240691521024388, 17.32521578647535776, -1.500000000000002220 ) ) ;
#32394 = AXIS2_PLACEMENT_3D ( 'NONE', #75729, #89978, #27589 ) ;
#32395 = CARTESIAN_POINT ( 'NONE',  ( -3.722501342491481235, -21.08806747394077519, 11.49999999999998934 ) ) ;
#32396 = CARTESIAN_POINT ( 'NONE',  ( 9.950000000000006395, 0.000000000000000000, 18.35000000000000142 ) ) ;
#32397 = CARTESIAN_POINT ( 'NONE',  ( -60.48527586300784264, -24.83644354574317603, 8.397322867105112110 ) ) ;
#32398 = CARTESIAN_POINT ( 'NONE',  ( -100.6228709571500701, -23.85229601348997264, 10.88205029486208275 ) ) ;
#32399 = CARTESIAN_POINT ( 'NONE',  ( -100.8624150394625616, -25.27359993006566441, 3.378658782965809682 ) ) ;
#32400 = CARTESIAN_POINT ( 'NONE',  ( 0.6941480231959694658, 22.73124288027050710, -1.500000000000002220 ) ) ;
#32401 = ADVANCED_FACE ( 'NONE', ( #18929 ), #80842, .F. ) ;
#32402 = B_SPLINE_CURVE_WITH_KNOTS ( 'NONE', 3,
 ( #13488, #20603, #75384, #67806, #91116, #21591 ),
 .UNSPECIFIED., .F., .F.,
 ( 4, 2, 4 ),
 ( 6.391158118969315506E-06, 0.001387004593080787881, 0.002767618028042606766 ),
 .UNSPECIFIED. ) ;
#32403 = AXIS2_PLACEMENT_3D ( 'NONE', #59334, #95894, #74556 ) ;
#32404 = CARTESIAN_POINT ( 'NONE',  ( -98.63811850894654754, -23.48783264082476308, -1.443836473390089914 ) ) ;
#32405 = DIRECTION ( 'NONE',  ( -0.000000000000000000, -1.000000000000000000, -0.000000000000000000 ) ) ;
#32406 = CARTESIAN_POINT ( 'NONE',  ( -16.82575997001036328, 10.57904039763333159, 11.49999999999999645 ) ) ;
#32407 = CARTESIAN_POINT ( 'NONE',  ( -123.5222519426676371, -23.48786465467241413, 11.44779295918253759 ) ) ;
#32408 = DIRECTION ( 'NONE',  ( 1.526034937513432889E-15, 0.000000000000000000, 1.000000000000000000 ) ) ;
#32409 = DIRECTION ( 'NONE',  ( -0.9978940991575084851, -0.000000000000000000, -0.06486421869277853025 ) ) ;
#32410 = VERTEX_POINT ( 'NONE', #43286 ) ;
#32411 = CARTESIAN_POINT ( 'NONE',  ( -23.71328795744024021, -5.965225279485594001, -17.58350715675015152 ) ) ;
#32412 = CARTESIAN_POINT ( 'NONE',  ( -6.680782769985652791, -6.376774720514411854, 19.46295461892502132 ) ) ;
#32413 = CARTESIAN_POINT ( 'NONE',  ( -80.62287095715005592, -29.50250243563736774, 8.947779886222141599 ) ) ;
#32414 = CARTESIAN_POINT ( 'NONE',  ( -5.395268184683536639, 21.00466093859614958, -1.500000000000002220 ) ) ;
#32415 = DIRECTION ( 'NONE',  ( -1.000000000000000000, -3.773278334444166432E-23, -8.201307841325785021E-29 ) ) ;
#32416 = CARTESIAN_POINT ( 'NONE',  ( -15.63568348323273227, -11.59263941501104966, -1.500000000000002220 ) ) ;
#32417 = CARTESIAN_POINT ( 'NONE',  ( -55.63763619402278948, -24.52399227489126687, 9.353111116836526406 ) ) ;
#32418 = ADVANCED_FACE ( 'NONE', ( #41278 ), #74238, .T. ) ;
#32419 = ORIENTED_EDGE ( 'NONE', *, *, #83815, .T. ) ;
#32420 = CARTESIAN_POINT ( 'NONE',  ( 18.16468007720714795, -9.286844270591712913, 11.49999999999999645 ) ) ;
#32421 = CARTESIAN_POINT ( 'NONE',  ( -87.62287095715004170, -29.50250243563736774, 8.947779886222139822 ) ) ;
#32422 = EDGE_CURVE ( 'NONE', #94339, #15795, #36654, .T. ) ;
#32423 = CARTESIAN_POINT ( 'NONE',  ( -24.90875734969025501, 3.316774720514426456, 29.49402280011862487 ) ) ;
#32424 = ORIENTED_EDGE ( 'NONE', *, *, #26170, .F. ) ;
#32425 = CARTESIAN_POINT ( 'NONE',  ( -78.98769050135813075, -25.22659656181679821, 6.389866568871956254 ) ) ;
#32426 = CARTESIAN_POINT ( 'NONE',  ( -95.52287095715007581, -23.84081130425358097, 10.88220057483157888 ) ) ;
#32427 = CARTESIAN_POINT ( 'NONE',  ( 30.56847537397349157, -4.007320673719170223, 25.16530555504002820 ) ) ;
#32428 = CARTESIAN_POINT ( 'NONE',  ( -49.29568538784691611, -25.25138839280181102, 5.964271804705676416 ) ) ;
#32429 = CARTESIAN_POINT ( 'NONE',  ( -1.044871794871793602, -5.876774720514418071, 20.44941907051282115 ) ) ;
#32430 = CARTESIAN_POINT ( 'NONE',  ( 15.80722972286721983, -12.41807379269815215, 11.49999999999998934 ) ) ;
#32431 = CARTESIAN_POINT ( 'NONE',  ( -89.55620429048339304, -24.66019654487199375, 8.947790411086124607 ) ) ;
#32432 = EDGE_LOOP ( 'NONE', ( #91859, #90705, #10657, #40136 ) ) ;
#32433 = CARTESIAN_POINT ( 'NONE',  ( -66.56566600343955997, -23.48786465467241058, 11.44779295918254824 ) ) ;
#32434 = CARTESIAN_POINT ( 'NONE',  ( -11.38079350637645959, -19.95400817559217899, 11.49999999999999645 ) ) ;
#32435 = CARTESIAN_POINT ( 'NONE',  ( 10.71911242904675987, 20.06137936439360203, 11.49999999999998934 ) ) ;
#32436 = ORIENTED_EDGE ( 'NONE', *, *, #75003, .F. ) ;
#32437 = DIRECTION ( 'NONE',  ( 0.000000000000000000, 0.000000000000000000, 1.000000000000000000 ) ) ;
#32438 = CARTESIAN_POINT ( 'NONE',  ( -75.62287095715004170, -25.00182538069145366, 7.747789668545099317 ) ) ;
#32439 = LINE ( 'NONE', #47676, #41960 ) ;
#32440 = CARTESIAN_POINT ( 'NONE',  ( 5.395440699609677537, 5.965225279485594001, -28.51842087987364138 ) ) ;
#32441 = AXIS2_PLACEMENT_3D ( 'NONE', #62044, #37203, #68156 ) ;
#32442 = CARTESIAN_POINT ( 'NONE',  ( -70.62287095715004170, -23.48786465467241058, 11.44779295918254469 ) ) ;
#32443 = FACE_OUTER_BOUND ( 'NONE', #93645, .T. ) ;
#32444 = CARTESIAN_POINT ( 'NONE',  ( -54.52287095715006870, -24.50216790748204332, 0.6166512839542456215 ) ) ;
#32445 = CARTESIAN_POINT ( 'NONE',  ( -99.04404089887771079, -25.31200610177687338, 5.494369131775782122 ) ) ;
#32446 = ORIENTED_EDGE ( 'NONE', *, *, #88733, .F. ) ;
#32447 = VECTOR ( 'NONE', #29458, 1000.000000000000000 ) ;
#32448 = CARTESIAN_POINT ( 'NONE',  ( 16.53694760393551988, -11.94906295602464397, -1.500000000000002220 ) ) ;
#32449 = B_SPLINE_CURVE_WITH_KNOTS ( 'NONE', 3,
 ( #47449, #32209, #24594, #93601, #8882, #2784, #70287, #8378, #94614, #48954, #2285, #23587, #24096, #79384 ),
 .UNSPECIFIED., .F., .F.,
 ( 4, 2, 2, 2, 2, 2, 4 ),
 ( 0.000000000000000000, 0.0001838514736245833582, 0.0003677029472491667164, 0.0007354058944983334328, 0.001103108841747500041, 0.001286960315372091476, 0.001470811788996682912 ),
 .UNSPECIFIED. ) ;
#32450 = ORIENTED_EDGE ( 'NONE', *, *, #6602, .T. ) ;
#32451 = CARTESIAN_POINT ( 'NONE',  ( -21.48638390452810043, -8.140844714011898020, -1.500000000000002220 ) ) ;
#32452 = CARTESIAN_POINT ( 'NONE',  ( -7.131053040288445999, -5.876774720514413630, 19.60308799987318196 ) ) ;
#32453 = VERTEX_POINT ( 'NONE', #74706 ) ;
#32454 = CARTESIAN_POINT ( 'NONE',  ( -102.5228709571501042, -24.66019654487200441, 8.947790411086119278 ) ) ;
#32455 = CARTESIAN_POINT ( 'NONE',  ( -8.676776695296464226, 18.57322330470350735, 2.100000000000000089 ) ) ;
#32456 = VECTOR ( 'NONE', #69938, 1000.000000000000114 ) ;
#32457 = CARTESIAN_POINT ( 'NONE',  ( -116.4728709572981558, -25.30561156865042349, 5.197853587462041070 ) ) ;
#32459 = ORIENTED_EDGE ( 'NONE', *, *, #25660, .F. ) ;
#32458 = CARTESIAN_POINT ( 'NONE',  ( -11.06822068739258391, -18.21809710261049275, 11.49999999999999645 ) ) ;
#32460 = AXIS2_PLACEMENT_3D ( 'NONE', #67412, #75493, #67916 ) ;
#32461 = VERTEX_POINT ( 'NONE', #90937 ) ;
#32462 = CARTESIAN_POINT ( 'NONE',  ( -10.71655374829924767, -19.46388382022006525, 11.49999999999998934 ) ) ;
#32463 = CARTESIAN_POINT ( 'NONE',  ( 19.46067915675286386, 6.892634557253153105, 11.49999999999998934 ) ) ;
#32464 = ORIENTED_EDGE ( 'NONE', *, *, #77949, .F. ) ;
#32465 = CARTESIAN_POINT ( 'NONE',  ( -6.369015873774380943, -5.876774720514413630, 19.23384392940399934 ) ) ;
#32466 = FACE_OUTER_BOUND ( 'NONE', #61200, .T. ) ;
#32467 = ORIENTED_EDGE ( 'NONE', *, *, #94038, .F. ) ;
#32468 = ADVANCED_FACE ( 'NONE', ( #82819 ), #21409, .F. ) ;
#32469 = CARTESIAN_POINT ( 'NONE',  ( -10.21384395349174490, -3.316774720514427344, 29.49402280011862487 ) ) ;
#32470 = VERTEX_POINT ( 'NONE', #75701 ) ;
#32472 = ADVANCED_FACE ( 'NONE', ( #37651 ), #67620, .T. ) ;
#32471 = CARTESIAN_POINT ( 'NONE',  ( -49.52287095715006160, -23.48783264082477018, -1.443836473390095465 ) ) ;
#32473 = FACE_OUTER_BOUND ( 'NONE', #83606, .T. ) ;
#32474 = CARTESIAN_POINT ( 'NONE',  ( 14.99592430652175956, 14.54719766626331889, -1.500000000000002220 ) ) ;
#32475 = CARTESIAN_POINT ( 'NONE',  ( -17.41291239988371231, 13.16847401419012975, 11.49999999999999645 ) ) ;
#32476 = EDGE_CURVE ( 'NONE', #65705, #88108, #45275, .T. ) ;
#32477 = CARTESIAN_POINT ( 'NONE',  ( -27.27372260060660736, -24.77993783887843904, 7.541612773693165295 ) ) ;
#32478 = DIRECTION ( 'NONE',  ( 0.000000000000000000, -2.173523156925979552E-06, 0.9999999999976378895 ) ) ;
#32479 = CARTESIAN_POINT ( 'NONE',  ( 17.90692129536829924, 13.62026984716248101, 11.49999999999998934 ) ) ;
#32480 = EDGE_CURVE ( 'NONE', #98958, #62104, #56582, .T. ) ;
#32481 = CARTESIAN_POINT ( 'NONE',  ( -118.5537731958665830, -24.35071581493543746, 9.817618358456021710 ) ) ;
#32482 = FACE_OUTER_BOUND ( 'NONE', #27139, .T. ) ;
#32483 = DIRECTION ( 'NONE',  ( -0.000000000000000000, -0.000000000000000000, -1.000000000000000000 ) ) ;
#32484 = ORIENTED_EDGE ( 'NONE', *, *, #79118, .T. ) ;
#32485 = B_SPLINE_CURVE_WITH_KNOTS ( 'NONE', 3,
 ( #4488, #57292, #97325, #88226 ),
 .UNSPECIFIED., .F., .F.,
 ( 4, 4 ),
 ( 0.3690289907973323125, 0.3700297378380976165 ),
 .UNSPECIFIED. ) ;
#32486 = EDGE_LOOP ( 'NONE', ( #74989, #33735, #35470, #45497 ) ) ;
#32487 = VERTEX_POINT ( 'NONE', #37153 ) ;
#32488 = B_SPLINE_CURVE_WITH_KNOTS ( 'NONE', 3,
 ( #84300, #47142, #64390, #94799 ),
 .UNSPECIFIED., .F., .F.,
 ( 4, 4 ),
 ( 0.1999286886604119962, 0.2089351199325275577 ),
 .UNSPECIFIED. ) ;
#32489 = CARTESIAN_POINT ( 'NONE',  ( -99.41830603981939873, -25.26221207296531546, 6.591151539727326814 ) ) ;
#32490 = EDGE_LOOP ( 'NONE', ( #12486, #50841, #25225, #48186, #67327 ) ) ;
#32491 = CARTESIAN_POINT ( 'NONE',  ( -3.722501342491481235, -21.08806747394077519, -1.500000000000002220 ) ) ;
#32492 = EDGE_CURVE ( 'NONE', #25133, #64522, #15390, .T. ) ;
#32493 = CARTESIAN_POINT ( 'NONE',  ( -1.374798071107336206, -22.32369649477951512, 11.49999999999999645 ) ) ;
#32494 = ORIENTED_EDGE ( 'NONE', *, *, #89088, .F. ) ;
#32495 = FACE_OUTER_BOUND ( 'NONE', #15598, .T. ) ;
#32496 = CARTESIAN_POINT ( 'NONE',  ( -14.29351441246084065, -15.47709782942846424, -1.500000000000002220 ) ) ;
#32497 = CARTESIAN_POINT ( 'NONE',  ( -30.53943611156634219, -24.75785870443472447, 8.640462295247353097 ) ) ;
#32498 = CARTESIAN_POINT ( 'NONE',  ( 8.914523860536577970, -17.85282776015759154, -1.500000000000002220 ) ) ;
#32499 = DIRECTION ( 'NONE',  ( 1.000000000000000000, 3.773278334444166432E-23, 8.201307841325785021E-29 ) ) ;
#32500 = CARTESIAN_POINT ( 'NONE',  ( 2.935461252226840401, -6.376774720514420736, 20.47627681611744777 ) ) ;
#32501 = CARTESIAN_POINT ( 'NONE',  ( -17.76638496452178018, -13.01238552544781335, -1.500000000000002220 ) ) ;
#32502 = CARTESIAN_POINT ( 'NONE',  ( -109.5228709571500616, -29.50248528299804818, 1.056150453629043584 ) ) ;
#32503 = VERTEX_POINT ( 'NONE', #30028 ) ;
#32504 = CARTESIAN_POINT ( 'NONE',  ( -65.57896135027826290, -24.92592662359561473, 8.075495903017998245 ) ) ;
#32505 = DIRECTION ( 'NONE',  ( 0.000000000000000000, 1.000000000000000000, 0.000000000000000000 ) ) ;
#32506 = CARTESIAN_POINT ( 'NONE',  ( -13.77211689728001964, -15.67653869864640903, 11.49999999999999645 ) ) ;
#32507 = FACE_OUTER_BOUND ( 'NONE', #61044, .T. ) ;
#32508 = CARTESIAN_POINT ( 'NONE',  ( -111.5228709571500616, -23.48786465467242479, 11.44779295918253936 ) ) ;
#32509 = CARTESIAN_POINT ( 'NONE',  ( -127.6228709571500559, -23.48783264082479505, -1.443836473390056829 ) ) ;
#32510 = CARTESIAN_POINT ( 'NONE',  ( -6.196366259867160942, 20.41550611124569059, 11.49999999999998934 ) ) ;
#32511 = LINE ( 'NONE', #41640, #90420 ) ;
#32512 = CARTESIAN_POINT ( 'NONE',  ( -66.62287095715005592, -23.47593901973091235, -1.443836447539006196 ) ) ;
#32513 = VECTOR ( 'NONE', #15489, 1000.000000000000114 ) ;
#32514 = PLANE ( 'NONE',  #42278 ) ;
#32515 = LINE ( 'NONE', #55872, #20004 ) ;
#32516 = CARTESIAN_POINT ( 'NONE',  ( -21.16606679798846358, 7.723709098063864076, -1.500000000000002220 ) ) ;
#32517 = FACE_OUTER_BOUND ( 'NONE', #24620, .T. ) ;
#32518 = ORIENTED_EDGE ( 'NONE', *, *, #71035, .T. ) ;
#32519 = CARTESIAN_POINT ( 'NONE',  ( 0.3910256410256383042, -5.876774720514409189, 19.19230769230768985 ) ) ;
#32520 = CARTESIAN_POINT ( 'NONE',  ( -122.6228709571500417, -23.47593901973091235, -1.443836447538997536 ) ) ;
#32521 = CARTESIAN_POINT ( 'NONE',  ( 16.13486940644654766, 11.28601765141728741, 11.49999999999999645 ) ) ;
#32522 = CARTESIAN_POINT ( 'NONE',  ( -89.52287095715006160, -24.65952944569304606, 1.056160979905700570 ) ) ;
#32523 = CARTESIAN_POINT ( 'NONE',  ( 0.000000000000000000, 0.000000000000000000, 9.000000000000000000 ) ) ;
#32524 = ORIENTED_EDGE ( 'NONE', *, *, #99137, .T. ) ;
#32525 = CARTESIAN_POINT ( 'NONE',  ( -99.59346018923595523, -23.96119346886881374, -0.6495511937831867089 ) ) ;
#32526 = CARTESIAN_POINT ( 'NONE',  ( -124.5228709571500616, -29.50248528299804818, 1.056150453629045360 ) ) ;
#32527 = PLANE ( 'NONE',  #52870 ) ;
#32528 = EDGE_CURVE ( 'NONE', #45070, #35025, #65208, .T. ) ;
#32529 = CARTESIAN_POINT ( 'NONE',  ( -41.32836283488544638, 4.132774720514426292, 39.26872235229541985 ) ) ;
#32530 = CARTESIAN_POINT ( 'NONE',  ( -8.281543130087330340, -17.94227898472161797, -1.500000000000002220 ) ) ;
#32531 = CIRCLE ( 'NONE', #48777, 28.96799999999999287 ) ;
#32532 = VERTEX_POINT ( 'NONE', #61001 ) ;
#32533 = VECTOR ( 'NONE', #33715, 1000.000000000000114 ) ;
#32534 = CARTESIAN_POINT ( 'NONE',  ( -13.29518446780263119, -15.22762515321373478, 11.49999999999999645 ) ) ;
#32535 = CARTESIAN_POINT ( 'NONE',  ( -112.6228709571500417, -24.66019654487199730, 8.947790411086124607 ) ) ;
#32536 = ADVANCED_FACE ( 'NONE', ( #91935 ), #22406, .T. ) ;
#32537 = EDGE_CURVE ( 'NONE', #33122, #24488, #48960, .T. ) ;
#32538 = ORIENTED_EDGE ( 'NONE', *, *, #95128, .T. ) ;
#32539 = CARTESIAN_POINT ( 'NONE',  ( -67.62287095715007013, -23.73907113216991860, -1.053371485793226814 ) ) ;
#32540 = CARTESIAN_POINT ( 'NONE',  ( -70.04721975296412495, -25.30058798389317332, 5.351639246407742689 ) ) ;
#32541 = CARTESIAN_POINT ( 'NONE',  ( -88.88918693012689687, -25.25185156220469551, 6.255794136723666909 ) ) ;
#32542 = CARTESIAN_POINT ( 'NONE',  ( -82.62287095715005592, -23.47593901973091235, -1.443836447539004642 ) ) ;
#32543 = DIRECTION ( 'NONE',  ( 0.000000000000000000, -0.9999999999976377785, -2.173523156925979128E-06 ) ) ;
#32544 = CARTESIAN_POINT ( 'NONE',  ( -11.64875734969026233, -0.3587747205144265483, 31.02402280011862246 ) ) ;
#32545 = CARTESIAN_POINT ( 'NONE',  ( -10.28607412905329532, -17.16720287211733975, 11.49999999999998934 ) ) ;
#32546 = LINE ( 'NONE', #39653, #20800 ) ;
#32547 = CARTESIAN_POINT ( 'NONE',  ( -116.5534035506147177, -24.35071581493543746, 9.817618358456021710 ) ) ;
#32548 = ORIENTED_EDGE ( 'NONE', *, *, #81071, .T. ) ;
#32549 = CARTESIAN_POINT ( 'NONE',  ( -104.6228709571500559, -24.66019654487200086, 8.947790411086124607 ) ) ;
#32550 = CARTESIAN_POINT ( 'NONE',  ( -6.660000000000001030, 2.888964624466060727, -0.2527516539682188590 ) ) ;
#32551 = CARTESIAN_POINT ( 'NONE',  ( -35.46596725541123618, -25.00158670708910336, 2.256160236439224143 ) ) ;
#32552 = CARTESIAN_POINT ( 'NONE',  ( -82.52287095715006160, -24.64965694238407323, 8.947790433994198267 ) ) ;
#32553 = DIRECTION ( 'NONE',  ( 0.000000000000000000, 0.000000000000000000, -1.000000000000000000 ) ) ;
#32554 = CARTESIAN_POINT ( 'NONE',  ( -83.54433019474268463, -24.51314013834315375, 0.6176544820404104019 ) ) ;
#32555 = CARTESIAN_POINT ( 'NONE',  ( -3.054691362729579751, -5.876774720514413630, 19.78730719034165375 ) ) ;
#32556 = CARTESIAN_POINT ( 'NONE',  ( -31.62287095715005236, -24.65952944569304250, 1.056160979905689690 ) ) ;
#32557 = EDGE_LOOP ( 'NONE', ( #71740, #36862, #84863, #66478 ) ) ;
#32558 = CARTESIAN_POINT ( 'NONE',  ( -3.904290608643684379, -19.93223805144805283, 11.49999999999998934 ) ) ;
#32559 = CARTESIAN_POINT ( 'NONE',  ( -28.55620429048340370, -24.50151139823071489, 1.056161648317806234 ) ) ;
#32560 = CARTESIAN_POINT ( 'NONE',  ( -34.51266535100846511, -23.73766607897670866, -1.055555164236443133 ) ) ;
#32561 = CARTESIAN_POINT ( 'NONE',  ( -102.6228709571500559, -29.50250786944525672, 11.44777988621623166 ) ) ;
#32562 = ORIENTED_EDGE ( 'NONE', *, *, #66654, .T. ) ;
#32563 = EDGE_CURVE ( 'NONE', #69040, #25971, #89276, .T. ) ;
#32564 = DIRECTION ( 'NONE',  ( 0.4771587602595988020, 0.8788171126619706008, -0.000000000000000000 ) ) ;
#32565 = CARTESIAN_POINT ( 'NONE',  ( 16.36621611169882229, 11.82581248522330064, -1.500000000000002220 ) ) ;
#32566 = CARTESIAN_POINT ( 'NONE',  ( 15.93590435955092843, -13.91358336426615239, 11.49999999999999645 ) ) ;
#32567 = CARTESIAN_POINT ( 'NONE',  ( -18.17467834739497690, 12.62983929299386965, -1.500000000000002220 ) ) ;
#32568 = B_SPLINE_CURVE_WITH_KNOTS ( 'NONE', 3,
 ( #90950, #89955, #68125, #75223 ),
 .UNSPECIFIED., .F., .F.,
 ( 4, 4 ),
 ( 0.000000000000000000, 0.0001000000000000167422 ),
 .UNSPECIFIED. ) ;
#32569 = AXIS2_PLACEMENT_3D ( 'NONE', #60495, #4700, #19905 ) ;
#32570 = CARTESIAN_POINT ( 'NONE',  ( -20.56140336115741718, 0.6910293267889283664, 11.49999999999998934 ) ) ;
#32571 = DIRECTION ( 'NONE',  ( -3.773278334453079618E-23, 0.9999999999976377785, 2.173523156925979975E-06 ) ) ;
#32572 = VERTEX_POINT ( 'NONE', #70605 ) ;
#32573 = CARTESIAN_POINT ( 'NONE',  ( -94.55620429048339304, -24.66019654487199730, 8.947790411086124607 ) ) ;
#32574 = VERTEX_POINT ( 'NONE', #587 ) ;
#32575 = LINE ( 'NONE', #31573, #96517 ) ;
#32576 = LINE ( 'NONE', #71650, #22657 ) ;
#32577 = ORIENTED_EDGE ( 'NONE', *, *, #77412, .F. ) ;
#32579 = ORIENTED_EDGE ( 'NONE', *, *, #32067, .T. ) ;
#32578 = EDGE_CURVE ( 'NONE', #22171, #67798, #61503, .T. ) ;
#32580 = EDGE_LOOP ( 'NONE', ( #51837, #86845, #58955, #43680 ) ) ;
#32581 = CARTESIAN_POINT ( 'NONE',  ( -111.4896040003763602, -25.21196470494054509, 3.415743279166374435 ) ) ;
#32582 = CARTESIAN_POINT ( 'NONE',  ( 6.457852148677970305, -6.376774720514415407, 20.09052163342618158 ) ) ;
#32583 = CARTESIAN_POINT ( 'NONE',  ( 5.443272695963705665, -5.876774720514417183, 20.27301970143225418 ) ) ;
#32584 = CARTESIAN_POINT ( 'NONE',  ( 18.97174343470660318, 8.267356841975738391, -1.500000000000002220 ) ) ;
#32585 = CARTESIAN_POINT ( 'NONE',  ( 20.17453868081960167, 7.849935799312063089, 11.49999999999999645 ) ) ;
#32586 = ORIENTED_EDGE ( 'NONE', *, *, #59460, .T. ) ;
#32587 = EDGE_CURVE ( 'NONE', #37822, #68524, #51714, .T. ) ;
#32588 = CARTESIAN_POINT ( 'NONE',  ( -98.92106654937062160, -25.27789303035052271, 5.825687011034560214 ) ) ;
#32589 = CARTESIAN_POINT ( 'NONE',  ( 2.590388488674697953, -5.876774720514415407, 19.94764386045124027 ) ) ;
#32590 = CARTESIAN_POINT ( 'NONE',  ( 15.34105849444754455, 16.31744944422920440, -1.500000000000002220 ) ) ;
#32591 = EDGE_CURVE ( 'NONE', #29538, #52807, #39649, .T. ) ;
#32592 = CARTESIAN_POINT ( 'NONE',  ( -79.34796103478946350, -25.12205572456604941, 6.000420134665034766 ) ) ;
#32593 = CARTESIAN_POINT ( 'NONE',  ( -84.62359692944605172, -24.65952944569303895, 1.056160979905700348 ) ) ;
#32594 = ORIENTED_EDGE ( 'NONE', *, *, #36146, .F. ) ;
#32595 = CARTESIAN_POINT ( 'NONE',  ( 29.68604458549361169, 6.066877414785177614, 27.51520267613161153 ) ) ;
#32596 = VECTOR ( 'NONE', #87059, 1000.000000000000114 ) ;
#32597 = CARTESIAN_POINT ( 'NONE',  ( -120.6228709571500417, -24.92604778743018556, 8.074972756849359001 ) ) ;
#32598 = ADVANCED_FACE ( 'NONE', ( #40159 ), #77693, .F. ) ;
#32599 = AXIS2_PLACEMENT_3D ( 'NONE', #80569, #94792, #41519 ) ;
#32600 = VERTEX_POINT ( 'NONE', #46772 ) ;
#32601 = EDGE_CURVE ( 'NONE', #91107, #58389, #33476, .T. ) ;
#32602 = ORIENTED_EDGE ( 'NONE', *, *, #35579, .T. ) ;
#32603 = LINE ( 'NONE', #86390, #19843 ) ;
#32604 = EDGE_LOOP ( 'NONE', ( #81797, #61620, #90249, #60437 ) ) ;
#32605 = LINE ( 'NONE', #10271, #30915 ) ;
#32606 = CARTESIAN_POINT ( 'NONE',  ( 14.70648301983428397, -15.34743991077593250, -1.500000000000002220 ) ) ;
#32607 = VERTEX_POINT ( 'NONE', #100023 ) ;
#32608 = CARTESIAN_POINT ( 'NONE',  ( -50.60991848927657344, -23.85016227208579309, -0.8807180028928346394 ) ) ;
#32609 = CARTESIAN_POINT ( 'NONE',  ( -17.41291239988371231, 13.16847401419012975, -1.500000000000002220 ) ) ;
#32610 = CARTESIAN_POINT ( 'NONE',  ( -103.5979546920953993, -23.48786465467241413, 11.44779295918254292 ) ) ;
#32611 = CARTESIAN_POINT ( 'NONE',  ( -111.5228709571500616, -24.64898659630368627, 1.056161002820831474 ) ) ;
#32612 = CARTESIAN_POINT ( 'NONE',  ( -109.5895376238166961, -24.65952944569304606, 1.056160979905701014 ) ) ;
#32613 = CARTESIAN_POINT ( 'NONE',  ( -13.95179422449595208, 16.79422078803934326, -1.500000000000002220 ) ) ;
#32614 = CARTESIAN_POINT ( 'NONE',  ( -95.52287095715011844, -24.63287334234179937, 0.9662140553045371894 ) ) ;
#32615 = ORIENTED_EDGE ( 'NONE', *, *, #45236, .F. ) ;
#32616 = EDGE_CURVE ( 'NONE', #76295, #88312, #79483, .T. ) ;
#32617 = CARTESIAN_POINT ( 'NONE',  ( 26.51188133999063723, 5.098757596203291165, -7.190425899444944591 ) ) ;
#32618 = CARTESIAN_POINT ( 'NONE',  ( -85.49847897960830778, -24.83644354573578994, 8.397322867130101898 ) ) ;
#32619 = ORIENTED_EDGE ( 'NONE', *, *, #67108, .T. ) ;
#32620 = VERTEX_POINT ( 'NONE', #78199 ) ;
#32621 = ORIENTED_EDGE ( 'NONE', *, *, #94899, .F. ) ;
#32622 = FACE_OUTER_BOUND ( 'NONE', #54980, .T. ) ;
#32623 = DIRECTION ( 'NONE',  ( 1.000000000000000000, 0.000000000000000000, 0.000000000000000000 ) ) ;
#32624 = CARTESIAN_POINT ( 'NONE',  ( -21.08002519818654363, -2.465602145356518893, -1.500000000000002220 ) ) ;
#32625 = CARTESIAN_POINT ( 'NONE',  ( -94.54934828576006112, -24.34968618360933945, 0.1864209137778860548 ) ) ;
#32626 = PLANE ( 'NONE',  #44660 ) ;
#32627 = CARTESIAN_POINT ( 'NONE',  ( -44.52287095715006160, -23.48786465467241058, 11.44779295918255180 ) ) ;
#32628 = CARTESIAN_POINT ( 'NONE',  ( -127.6228709571500275, -24.66019654487199730, 8.947790411086121054 ) ) ;
#32629 = CARTESIAN_POINT ( 'NONE',  ( -4.539579955115475407, -18.87035741768621122, 11.49999999999998934 ) ) ;
#32630 = CARTESIAN_POINT ( 'NONE',  ( -45.57314457103787930, -25.00158670708910691, 2.256160236439225031 ) ) ;
#32631 = ORIENTED_EDGE ( 'NONE', *, *, #25014, .F. ) ;
#32632 = CARTESIAN_POINT ( 'NONE',  ( 4.865394487973861537, 18.91859722749940786, 11.49999999999999645 ) ) ;
#32633 = DIRECTION ( 'NONE',  ( -0.000000000000000000, -0.000000000000000000, -1.000000000000000000 ) ) ;
#32634 = B_SPLINE_CURVE_WITH_KNOTS ( 'NONE', 3,
 ( #10029, #88165, #71947, #87660 ),
 .UNSPECIFIED., .F., .F.,
 ( 4, 4 ),
 ( 2.775557561562891351E-17, 0.001846153846153872347 ),
 .UNSPECIFIED. ) ;
#32635 = LINE ( 'NONE', #33646, #80435 ) ;
#32636 = EDGE_CURVE ( 'NONE', #88018, #17782, #24922, .T. ) ;
#32637 = ORIENTED_EDGE ( 'NONE', *, *, #76248, .T. ) ;
#32638 = CARTESIAN_POINT ( 'NONE',  ( 4.854822496258163866, -5.876774720514421624, 20.96950945262037891 ) ) ;
#32639 = CARTESIAN_POINT ( 'NONE',  ( -79.62287095715005592, -29.50250786944525672, 11.44777988621623521 ) ) ;
#32640 = FACE_OUTER_BOUND ( 'NONE', #66078, .T. ) ;
#32641 = EDGE_CURVE ( 'NONE', #13991, #98207, #38646, .T. ) ;
#32642 = PLANE ( 'NONE',  #52591 ) ;
#32643 = CARTESIAN_POINT ( 'NONE',  ( 18.24227566675094181, -7.298356753547692755, -1.500000000000002220 ) ) ;
#32644 = ORIENTED_EDGE ( 'NONE', *, *, #58844, .F. ) ;
#32645 = VECTOR ( 'NONE', #94553, 1000.000000000000000 ) ;
#32646 = CARTESIAN_POINT ( 'NONE',  ( -90.52287095715006160, -24.63345952396256067, 9.038047939301504741 ) ) ;
#32647 = FACE_OUTER_BOUND ( 'NONE', #59595, .T. ) ;
#32648 = DATE_AND_TIME ( #63627, #76474 ) ;
#32649 = ADVANCED_FACE ( 'NONE', ( #86329 ), #7191, .T. ) ;
#32650 = CARTESIAN_POINT ( 'NONE',  ( -125.5228709571500616, -25.00182538069146077, 7.747789668545104647 ) ) ;
#32651 = CARTESIAN_POINT ( 'NONE',  ( 4.373554412633047228, -6.376774720514422512, 21.19197260575996822 ) ) ;
#32652 = CARTESIAN_POINT ( 'NONE',  ( -76.52287095715003318, -24.34917612406836795, 0.1852690917426554063 ) ) ;
#32653 = CARTESIAN_POINT ( 'NONE',  ( -104.5228709571500758, -24.64965694238407323, 8.947790433994194714 ) ) ;
#32655 = B_SPLINE_CURVE_WITH_KNOTS ( 'NONE', 3,
 ( #46756, #92411, #68095, #15790, #83805, #99018 ),
 .UNSPECIFIED., .F., .F.,
 ( 4, 2, 4 ),
 ( 0.000000000000000000, 0.001380901958385387677, 0.002761803916770775354 ),
 .UNSPECIFIED. ) ;
#32654 = CARTESIAN_POINT ( 'NONE',  ( 5.811591729264017125, -5.876774720514421624, 21.22699980322195046 ) ) ;
#32656 = CARTESIAN_POINT ( 'NONE',  ( -129.6235880454576090, -24.34968618360934656, 0.1864209137778921610 ) ) ;
#32657 = CARTESIAN_POINT ( 'NONE',  ( -114.5568549121452264, -23.73791477778912196, 11.05961554403169700 ) ) ;
#32658 = CARTESIAN_POINT ( 'NONE',  ( -10.02925392579303576, -17.20239368982820238, 11.49999999999998934 ) ) ;
#32659 = EDGE_CURVE ( 'NONE', #24865, #43572, #30535, .T. ) ;
#32660 = CARTESIAN_POINT ( 'NONE',  ( -75.52207690583590249, -23.48786465467241058, 11.44779295918254824 ) ) ;
#32661 = CARTESIAN_POINT ( 'NONE',  ( -19.21288746854601115, 4.878285775029977955, -1.500000000000002220 ) ) ;
#32662 = ORIENTED_EDGE ( 'NONE', *, *, #60456, .T. ) ;
#32663 = CARTESIAN_POINT ( 'NONE',  ( -122.5228709571500616, -23.72773821059536914, 11.05748984161097326 ) ) ;
#32664 = VECTOR ( 'NONE', #28041, 1000.000000000000114 ) ;
#32665 = APPROVAL_PERSON_ORGANIZATION ( #41397, #48847, #95680 ) ;
#32666 = CARTESIAN_POINT ( 'NONE',  ( -51.48549811542276444, -25.22876079287771134, 6.454949072762300233 ) ) ;
#32667 = CARTESIAN_POINT ( 'NONE',  ( -92.52287095715006160, -29.50250243563736774, 8.947779886222139822 ) ) ;
#32668 = CARTESIAN_POINT ( 'NONE',  ( -20.39401028033356766, -3.670942005906183692, 11.49999999999999645 ) ) ;
#32669 = CARTESIAN_POINT ( 'NONE',  ( 24.50102500000003758, -9.528487854913448629, -1.499999999999996003 ) ) ;
#32670 = B_SPLINE_CURVE_WITH_KNOTS ( 'NONE', 3,
 ( #61109, #13910, #60616, #12913 ),
 .UNSPECIFIED., .F., .F.,
 ( 4, 4 ),
 ( 0.09056467001404970574, 0.09957110128616525335 ),
 .UNSPECIFIED. ) ;
#32671 = PRODUCT_RELATED_PRODUCT_CATEGORY ( 'detail', '', ( #2853 ) ) ;
#32672 = CARTESIAN_POINT ( 'NONE',  ( -78.52287095715009002, -24.33927499327854349, 9.819080762295801179 ) ) ;
#32673 = CARTESIAN_POINT ( 'NONE',  ( 22.69831151501224298, -1.600861625767590724, 11.49999999999999645 ) ) ;
#32674 = EDGE_LOOP ( 'NONE', ( #72007, #41244, #81939, #50832 ) ) ;
#32675 = CARTESIAN_POINT ( 'NONE',  ( -69.64018546353763384, -23.96119346886880308, -0.6495511937832122440 ) ) ;
#32676 = DIRECTION ( 'NONE',  ( 0.000000000000000000, 1.000000000000000000, 0.000000000000000000 ) ) ;
#32677 = ORIENTED_EDGE ( 'NONE', *, *, #79220, .F. ) ;
#32678 = CARTESIAN_POINT ( 'NONE',  ( -19.95319933381289701, -3.276446921841525306, -1.500000000000002220 ) ) ;
#32679 = CARTESIAN_POINT ( 'NONE',  ( 6.561060095583167495, -6.376774720514427841, 21.83518827598938117 ) ) ;
#32680 = CARTESIAN_POINT ( 'NONE',  ( -97.62287095715002749, -23.95044443724992078, 10.65354141964649592 ) ) ;
#32681 = ORIENTED_EDGE ( 'NONE', *, *, #62771, .T. ) ;
#32682 = LINE ( 'NONE', #93570, #56595 ) ;
#32683 = CARTESIAN_POINT ( 'NONE',  ( -9.034649315346676701, 21.08484869742704504, -1.500000000000002220 ) ) ;
#32684 = CARTESIAN_POINT ( 'NONE',  ( 6.573941812937369455, 0.2639660507643281639, 9.334907998774166978E-16 ) ) ;
#32685 = CARTESIAN_POINT ( 'NONE',  ( 19.98059151383774434, -0.7942727526097331792, -1.500000000000002220 ) ) ;
#32686 = CARTESIAN_POINT ( 'NONE',  ( -4.621320343559261801, 12.74999999999999645, 0.000000000000000000 ) ) ;
#32687 = CARTESIAN_POINT ( 'NONE',  ( 17.27681320446407298, 11.92757687370068886, 11.49999999999999645 ) ) ;
#32688 = CARTESIAN_POINT ( 'NONE',  ( -29.71670104680227453, -25.18823541688493250, 6.230496314888496201 ) ) ;
#32689 = CARTESIAN_POINT ( 'NONE',  ( 1.000208336950358934, 2.877919977996279334E-16, -2.349999999999999645 ) ) ;
#32690 = CARTESIAN_POINT ( 'NONE',  ( 6.148021820315829444, -21.18842874637755358, -1.500000000000002220 ) ) ;
#32691 = DIRECTION ( 'NONE',  ( 0.000000000000000000, 0.000000000000000000, -1.000000000000000000 ) ) ;
#32692 = EDGE_LOOP ( 'NONE', ( #166, #88318, #19354, #69687 ) ) ;
#32693 = VECTOR ( 'NONE', #51718, 1000.000000000000114 ) ;
#32694 = DIRECTION ( 'NONE',  ( 0.000000000000000000, -2.173523156925980399E-06, 0.9999999999976378895 ) ) ;
#32695 = CARTESIAN_POINT ( 'NONE',  ( -49.52164473449563076, -25.27344882170398321, 3.857971157315336797 ) ) ;
#32696 = CARTESIAN_POINT ( 'NONE',  ( -46.62287095715004170, -23.48783264082478439, -1.443836473390070818 ) ) ;
#32697 = ORIENTED_EDGE ( 'NONE', *, *, #858, .T. ) ;
#32698 = CARTESIAN_POINT ( 'NONE',  ( 2.884397429187188333, -6.376774720514406525, 18.67943752795919110 ) ) ;
#32699 = VERTEX_POINT ( 'NONE', #38142 ) ;
#32700 = ORIENTED_EDGE ( 'NONE', *, *, #4063, .T. ) ;
#32701 = EDGE_CURVE ( 'NONE', #60701, #23124, #49314, .T. ) ;
#32702 = FACE_OUTER_BOUND ( 'NONE', #72427, .T. ) ;
#32703 = B_SPLINE_CURVE_WITH_KNOTS ( 'NONE', 3,
 ( #84182, #59872, #44636, #60379 ),
 .UNSPECIFIED., .F., .F.,
 ( 4, 4 ),
 ( 0.000000000000000000, 9.999999999999592548E-05 ),
 .UNSPECIFIED. ) ;
#32704 = DIRECTION ( 'NONE',  ( 1.000000000000000000, 3.773278334444166432E-23, 8.201307841325785021E-29 ) ) ;
#32705 = LINE ( 'NONE', #26096, #146 ) ;
#32706 = CARTESIAN_POINT ( 'NONE',  ( 4.814550503181614260, -19.98661186389175271, -1.500000000000002220 ) ) ;
#32707 = VERTEX_POINT ( 'NONE', #24425 ) ;
#32708 = CARTESIAN_POINT ( 'NONE',  ( -99.38719565547299339, -25.28133435936707585, 5.772806929394654674 ) ) ;
#32709 = CARTESIAN_POINT ( 'NONE',  ( -44.59358526570461834, -24.15543982623906416, -0.2315651400026670914 ) ) ;
#32710 = CARTESIAN_POINT ( 'NONE',  ( -83.52287095715006160, -24.65952944569304606, 1.056160979905698794 ) ) ;
#32711 = CARTESIAN_POINT ( 'NONE',  ( -0.5504121640580519337, 22.28327991085032878, -1.500000000000002220 ) ) ;
#32712 = CARTESIAN_POINT ( 'NONE',  ( -0.05081623857416536771, -22.39214385819348507, 8.640809912072072052 ) ) ;
#32713 = DIRECTION ( 'NONE',  ( -3.773278334453079030E-23, 0.9999999999976377785, 2.173523156925979128E-06 ) ) ;
#32714 = EDGE_LOOP ( 'NONE', ( #40778, #60651, #34888, #83469 ) ) ;
#32715 = CARTESIAN_POINT ( 'NONE',  ( -68.62287095715005592, -23.48786465467241058, 11.44779295918254647 ) ) ;
#32716 = CARTESIAN_POINT ( 'NONE',  ( -124.6228709571500843, -24.50216790748206108, 0.6166512839542565017 ) ) ;
#32717 = EDGE_CURVE ( 'NONE', #41799, #33481, #25026, .T. ) ;
#32718 = CARTESIAN_POINT ( 'NONE',  ( -8.730572200882948053, 18.91488879456464289, -1.500000000000002220 ) ) ;
#32719 = CIRCLE ( 'NONE', #16484, 1.000000000000000000 ) ;
#32720 = ADVANCED_FACE ( 'NONE', ( #22897 ), #92, .T. ) ;
#32721 = ORIENTED_EDGE ( 'NONE', *, *, #43319, .T. ) ;
#32723 = ORIENTED_EDGE ( 'NONE', *, *, #87456, .T. ) ;
#32722 = CARTESIAN_POINT ( 'NONE',  ( -0.4453066574538939171, -6.376774720514410077, 19.14913681718892491 ) ) ;
#32724 = ORIENTED_EDGE ( 'NONE', *, *, #8136, .T. ) ;
#32725 = CARTESIAN_POINT ( 'NONE',  ( -69.21490423241783674, -25.25935235714723959, 7.033986463589522842 ) ) ;
#32726 = CARTESIAN_POINT ( 'NONE',  ( -4.359323203648655998, -20.60729432550360585, -1.500000000000002220 ) ) ;
#32727 = ORIENTED_EDGE ( 'NONE', *, *, #1189, .T. ) ;
#32728 = CARTESIAN_POINT ( 'NONE',  ( 4.784292611718075072, -6.376774720514426953, -25.54547254883186014 ) ) ;
#32729 = CARTESIAN_POINT ( 'NONE',  ( -53.52287095715006870, -23.47596703998600631, 11.44779298504229104 ) ) ;
#32730 = CARTESIAN_POINT ( 'NONE',  ( 7.227401621481964966, -5.356774720515139698, -27.22638491171618824 ) ) ;
#32731 = CARTESIAN_POINT ( 'NONE',  ( -101.6955034991685238, -25.03152311293479571, 6.928826238582348473 ) ) ;
#32732 = CARTESIAN_POINT ( 'NONE',  ( -109.9583214895175871, -25.12701665469254664, 2.868629235022660762 ) ) ;
#32733 = LINE ( 'NONE', #79405, #28559 ) ;
#32734 = CARTESIAN_POINT ( 'NONE',  ( -57.52287095715005449, -24.65952944569304606, 1.056160979905695463 ) ) ;
#32736 = ORIENTED_EDGE ( 'NONE', *, *, #38409, .F. ) ;
#32735 = CARTESIAN_POINT ( 'NONE',  ( 17.16062296631688255, 14.07911611715085876, 11.49999999999999645 ) ) ;
#32737 = EDGE_CURVE ( 'NONE', #45268, #62158, #51641, .T. ) ;
#32738 = DIRECTION ( 'NONE',  ( 0.000000000000000000, 0.000000000000000000, 1.000000000000000000 ) ) ;
#32739 = CARTESIAN_POINT ( 'NONE',  ( 30.53060340732036337, 1.477225279485574028, 3.744237563515920634E-15 ) ) ;
#32740 = ORIENTED_EDGE ( 'NONE', *, *, #58743, .F. ) ;
#32741 = CARTESIAN_POINT ( 'NONE',  ( -16.57510365746454184, 15.48777146884464884, -1.500000000000002220 ) ) ;
#32743 = ORIENTED_EDGE ( 'NONE', *, *, #98921, .T. ) ;
#32742 = CARTESIAN_POINT ( 'NONE',  ( -118.6228709571500701, -23.47596703998600631, 11.44779298504227683 ) ) ;
#32744 = AXIS2_PLACEMENT_3D ( 'NONE', #4725, #60019, #83831 ) ;
#32745 = ORIENTED_EDGE ( 'NONE', *, *, #95204, .T. ) ;
#32746 = APPROVAL_PERSON_ORGANIZATION ( #43402, #77331, #89566 ) ;
#32747 = DIRECTION ( 'NONE',  ( 1.000000000000000000, 0.000000000000000000, 0.000000000000000000 ) ) ;
#32748 = CARTESIAN_POINT ( 'NONE',  ( 16.24926901856429140, 11.90123039513101411, 11.49999999999998934 ) ) ;
#32749 = CARTESIAN_POINT ( 'NONE',  ( -51.52287095715009713, -23.95044443724991723, 10.65354141964648882 ) ) ;
#32750 = ORIENTED_EDGE ( 'NONE', *, *, #93546, .F. ) ;
#32751 = B_SPLINE_CURVE_WITH_KNOTS ( 'NONE', 3,
 ( #15116, #68906, #90747, #53196 ),
 .UNSPECIFIED., .F., .F.,
 ( 4, 4 ),
 ( 0.000000000000000000, 1.000000000000000000 ),
 .UNSPECIFIED. ) ;
#32752 = CARTESIAN_POINT ( 'NONE',  ( -130.5728709571500303, -24.37317526135185375, 9.969885471561841683 ) ) ;
#32753 = CARTESIAN_POINT ( 'NONE',  ( 1.926536275058113867, -22.33200895297504474, -1.500000000000002220 ) ) ;
#32754 = EDGE_CURVE ( 'NONE', #15615, #7760, #85316, .T. ) ;
#32755 = ORIENTED_EDGE ( 'NONE', *, *, #94896, .F. ) ;
#32756 = VERTEX_POINT ( 'NONE', #56905 ) ;
#32757 = CARTESIAN_POINT ( 'NONE',  ( -112.6256775209500063, -24.35071581493543391, 9.817618358456018157 ) ) ;
#32758 = CARTESIAN_POINT ( 'NONE',  ( -4.929522925832174884, 0.3587747205143967943, -28.63504101147569614 ) ) ;
#32759 = CARTESIAN_POINT ( 'NONE',  ( -117.6228709571500559, -23.47593901973091235, -1.443836447538997536 ) ) ;
#32760 = CARTESIAN_POINT ( 'NONE',  ( 31.50024378385495893, 5.449202613762975211, -3.047402719862319032 ) ) ;
#32761 = FACE_OUTER_BOUND ( 'NONE', #18318, .T. ) ;
#32762 = EDGE_CURVE ( 'NONE', #1499, #48074, #2113, .T. ) ;
#32763 = CARTESIAN_POINT ( 'NONE',  ( -16.94305004876727239, 9.801747318927828800, -1.500000000000002220 ) ) ;
#32764 = CARTESIAN_POINT ( 'NONE',  ( -33.62287095715005592, -24.64898659630367206, 1.056161002820817485 ) ) ;
#32765 = EDGE_LOOP ( 'NONE', ( #77250, #21459, #84152, #12230 ) ) ;
#32766 = CARTESIAN_POINT ( 'NONE',  ( -7.189238790567602067, -20.27908067168375794, -1.500000000000002220 ) ) ;
#32767 = CARTESIAN_POINT ( 'NONE',  ( -128.5899664415713062, -23.96119346886882084, -0.6495511937831803806 ) ) ;
#32768 = CARTESIAN_POINT ( 'NONE',  ( -38.55620429048340014, -23.47593901973091235, -1.443836447539011525 ) ) ;
#32770 = B_SPLINE_CURVE_WITH_KNOTS ( 'NONE', 3,
 ( #26935, #41676, #72619, #3116 ),
 .UNSPECIFIED., .F., .F.,
 ( 4, 4 ),
 ( 0.000000000000000000, 0.0001000000000000028644 ),
 .UNSPECIFIED. ) ;
#32769 = CARTESIAN_POINT ( 'NONE',  ( -63.62287095715004881, -24.66019654487199020, 8.947790411086131712 ) ) ;
#32771 = CARTESIAN_POINT ( 'NONE',  ( -52.62287095715006302, -24.65952944569304250, 1.056160979905695685 ) ) ;
#32772 = CARTESIAN_POINT ( 'NONE',  ( 21.75204538223844963, -7.182240389990739438, -1.500000000000002220 ) ) ;
#32773 = EDGE_CURVE ( 'NONE', #67333, #73040, #50281, .T. ) ;
#32774 = EDGE_CURVE ( 'NONE', #27745, #59988, #89205, .T. ) ;
#32775 = VECTOR ( 'NONE', #23245, 1000.000000000000114 ) ;
#32776 = CALENDAR_DATE ( 2026, 9, 10 ) ;
#32777 = DIRECTION ( 'NONE',  ( 0.000000000000000000, -2.891205793294678819E-16, 1.000000000000000000 ) ) ;
#32778 = CARTESIAN_POINT ( 'NONE',  ( -89.62287095715004170, -29.50250243563736774, 8.947779886222139822 ) ) ;
#32779 = CARTESIAN_POINT ( 'NONE',  ( 4.692034869050136336, 19.47840706813412126, 11.49999999999999645 ) ) ;
#32780 = PLANE ( 'NONE',  #26825 ) ;
#32781 = CARTESIAN_POINT ( 'NONE',  ( 3.252401863874210264, -5.965225279485592225, -29.35688408629928858 ) ) ;
#32782 = CARTESIAN_POINT ( 'NONE',  ( -46.52287095715007581, -23.48783264082477018, -1.443836473390096797 ) ) ;
#32783 = CARTESIAN_POINT ( 'NONE',  ( -38.62287095715005592, -24.64965695001467694, 8.947790433994187609 ) ) ;
#32784 = CARTESIAN_POINT ( 'NONE',  ( -59.52287095715006160, -29.50248528299804818, 1.056150453629034924 ) ) ;
#32785 = CARTESIAN_POINT ( 'NONE',  ( -13.65724274058436194, -16.95215541261048742, -1.500000000000002220 ) ) ;
#32786 = CARTESIAN_POINT ( 'NONE',  ( -127.5228709571499763, -23.48783264082477373, -1.443836473390082586 ) ) ;
#32787 = CARTESIAN_POINT ( 'NONE',  ( 19.42422255247381457, -2.945173967302487039, -1.500000000000002220 ) ) ;
#32788 = FACE_OUTER_BOUND ( 'NONE', #30529, .T. ) ;
#32789 = CARTESIAN_POINT ( 'NONE',  ( -32.52287095715008292, -23.94994826722564696, -0.6494450866342749151 ) ) ;
#32790 = ITEM_DEFINED_TRANSFORMATION ( 'NONE', 'NONE', #32599,  #37391 ) ;
#32791 = VECTOR ( 'NONE', #22032, 1000.000000000000000 ) ;
#32793 = CARTESIAN_POINT ( 'NONE',  ( 15.97264540888995299, 3.316774720514426456, -27.93485543958162864 ) ) ;
#32792 = B_SPLINE_CURVE_WITH_KNOTS ( 'NONE', 3,
 ( #44016, #74948, #83058, #44523 ),
 .UNSPECIFIED., .F., .F.,
 ( 4, 4 ),
 ( 0.000000000000000000, 1.000000000000000000 ),
 .UNSPECIFIED. ) ;
#32794 = CARTESIAN_POINT ( 'NONE',  ( 2.649863049427662709, -5.876774720514420736, 20.71861240329949538 ) ) ;
#32795 = CARTESIAN_POINT ( 'NONE',  ( 8.954683214801249846, 18.48387022957959047, 11.49999999999999645 ) ) ;
#32796 = CARTESIAN_POINT ( 'NONE',  ( 4.573489327750471567, -5.876774720514419847, 20.79634280254998657 ) ) ;
#32797 = VECTOR ( 'NONE', #79089, 1000.000000000000114 ) ;
#32798 = ADVANCED_FACE ( 'NONE', ( #3609 ), #34054, .F. ) ;
#32799 = PLANE ( 'NONE',  #23718 ) ;
#32800 = ADVANCED_FACE ( 'NONE', ( #64028 ), #94943, .T. ) ;
#32801 = CARTESIAN_POINT ( 'NONE',  ( 22.57354875331468591, -1.174960877787051716, 11.49999999999999645 ) ) ;
#32802 = ORIENTED_EDGE ( 'NONE', *, *, #7607, .T. ) ;
#32803 = SHAPE_REPRESENTATION_RELATIONSHIP ( 'NONE' , 'NONE' ,  #36681, #67027 ) ;
#32804 = CARTESIAN_POINT ( 'NONE',  ( -69.86129607977629519, -25.12219122924749826, 7.001236562355686921 ) ) ;
#32805 = CARTESIAN_POINT ( 'NONE',  ( -26.95182783290497852, -24.79956601504498437, 7.385977329265138280 ) ) ;
#32806 = DIRECTION ( 'NONE',  ( 0.9921023176230514551, 0.000000000000000000, -0.1254312216594016816 ) ) ;
#32807 = CARTESIAN_POINT ( 'NONE',  ( -74.92287095715006728, -23.47593901973090524, -1.443836447538997980 ) ) ;
#32808 = CARTESIAN_POINT ( 'NONE',  ( 2.100208336950355914, 0.000000000000000000, 0.000000000000000000 ) ) ;
#32809 = CARTESIAN_POINT ( 'NONE',  ( -69.52287095715006160, -29.50248528299804818, 1.056150453629036701 ) ) ;
#32810 = EDGE_CURVE ( 'NONE', #32056, #39449, #65030, .T. ) ;
#32811 = ADVANCED_FACE ( 'NONE', ( #96945 ), #79713, .T. ) ;
#32812 = ORIENTED_EDGE ( 'NONE', *, *, #81393, .T. ) ;
#32813 = VECTOR ( 'NONE', #55884, 1000.000000000000000 ) ;
#32814 = CARTESIAN_POINT ( 'NONE',  ( -28.47875734969026240, -5.965225279485572685, 26.43402280011862615 ) ) ;
#32815 = CARTESIAN_POINT ( 'NONE',  ( -2.521034868938843765, 22.70145277337256218, 11.49999999999998934 ) ) ;
#32816 = LINE ( 'NONE', #72886, #13036 ) ;
#32817 = CARTESIAN_POINT ( 'NONE',  ( -65.62287095715005592, -29.50250786944525672, 11.44777988621623699 ) ) ;
#32818 = CARTESIAN_POINT ( 'NONE',  ( -3.826923076923074429, -5.876774720514426953, 21.75000000000000355 ) ) ;
#32819 = APPROVAL_PERSON_ORGANIZATION ( #43037, #54338, #19674 ) ;
#32820 = CARTESIAN_POINT ( 'NONE',  ( 9.993301969596378953, 20.15287186522775542, 11.49999999999999645 ) ) ;
#32821 = ORIENTED_EDGE ( 'NONE', *, *, #53376, .F. ) ;
#32822 = CARTESIAN_POINT ( 'NONE',  ( -38.62287095715005592, -23.47596703998600276, 11.44779298504227505 ) ) ;
#32823 = CARTESIAN_POINT ( 'NONE',  ( -12.87221125579857528, -17.80329210173279364, 11.49999999999998934 ) ) ;
#32824 = CARTESIAN_POINT ( 'NONE',  ( 32.42932432802503939, 0.3587747205144265483, -0.2107846672978405389 ) ) ;
#32825 = CARTESIAN_POINT ( 'NONE',  ( -44.64704844554334784, -23.96169478059712787, 10.65365249895718414 ) ) ;
#32826 = CARTESIAN_POINT ( 'NONE',  ( -56.62287095715005592, -23.48786465467241413, 11.44779295918254824 ) ) ;
#32827 = VECTOR ( 'NONE', #55628, 1000.000000000000000 ) ;
#32828 = ORIENTED_EDGE ( 'NONE', *, *, #96034, .F. ) ;
#32829 = CARTESIAN_POINT ( 'NONE',  ( 282.9764569301858046, 0.6647747205144264315, 20.79159422840526616 ) ) ;
#32830 = CARTESIAN_POINT ( 'NONE',  ( -41.62287095715006302, -29.50248528299804818, 1.056150453629031594 ) ) ;
#32831 = ORIENTED_EDGE ( 'NONE', *, *, #18729, .T. ) ;
#32832 = CARTESIAN_POINT ( 'NONE',  ( -19.82921842031888104, 5.099586017421429140, 11.49999999999998934 ) ) ;
#32833 = ORIENTED_EDGE ( 'NONE', *, *, #59185, .T. ) ;
#32834 = ORIENTED_EDGE ( 'NONE', *, *, #12946, .F. ) ;
#32836 = VERTEX_POINT ( 'NONE', #56407 ) ;
#32835 = AXIS2_PLACEMENT_3D ( 'NONE', #46835, #77753, #8267 ) ;
#32837 = ORIENTED_EDGE ( 'NONE', *, *, #50963, .T. ) ;
#32838 = EDGE_CURVE ( 'NONE', #14217, #31069, #54166, .T. ) ;
#32839 = CARTESIAN_POINT ( 'NONE',  ( 16.03631736716203449, -16.64276770305488284, -1.500000000000002220 ) ) ;
#32840 = CARTESIAN_POINT ( 'NONE',  ( -39.43510301730458423, -25.26871255744266875, 3.880430150159563940 ) ) ;
#32841 = CARTESIAN_POINT ( 'NONE',  ( -0.9335293527496063559, -20.33857301660709638, -1.500000000000002220 ) ) ;
#32842 = EDGE_LOOP ( 'NONE', ( #34543, #99734, #85633, #4315 ) ) ;
#32843 = LINE ( 'NONE', #63820, #86591 ) ;
#32844 = LINE ( 'NONE', #62815, #23912 ) ;
#32845 = SHAPE_REPRESENTATION ( 'oval head_am_B18.6.7M - M2.5 x 0.45 x 13 Type I Cross Recessed OHMS --13C', ( #37391 ), #82851 ) ;
#32846 = CARTESIAN_POINT ( 'NONE',  ( -78.62287095715004170, -24.65952944569304606, 1.056160979905698349 ) ) ;
#32847 = CARTESIAN_POINT ( 'NONE',  ( 4.653846153846159517, -5.876774720514416295, 19.99999999999999289 ) ) ;
#32849 = VERTEX_POINT ( 'NONE', #87326 ) ;
#32848 = CARTESIAN_POINT ( 'NONE',  ( 20.96596170256846747, -4.772324250704091497, 11.49999999999999645 ) ) ;
#32850 = CARTESIAN_POINT ( 'NONE',  ( -75.49753373454176142, -24.63355581998385802, 0.9682620441943947664 ) ) ;
#32851 = DIRECTION ( 'NONE',  ( 0.000000000000000000, 0.000000000000000000, 1.000000000000000000 ) ) ;
#32852 = VERTEX_POINT ( 'NONE', #26444 ) ;
#32853 = CARTESIAN_POINT ( 'NONE',  ( -10.32638548400381673, 17.97674989526738898, 11.49999999999998934 ) ) ;
#32854 = EDGE_CURVE ( 'NONE', #13179, #2429, #38324, .T. ) ;
#32855 = VERTEX_POINT ( 'NONE', #80220 ) ;
#32857 = VERTEX_POINT ( 'NONE', #35053 ) ;
#32856 = DIRECTION ( 'NONE',  ( -0.000000000000000000, -1.000000000000000000, -0.000000000000000000 ) ) ;
#32858 = AXIS2_PLACEMENT_3D ( 'NONE', #59601, #44375, #59106 ) ;
#32859 = B_SPLINE_SURFACE_WITH_KNOTS ( 'NONE', 3, 1, ( 
 ( #83261, #28473 ),
 ( #90876, #45213 ),
 ( #30476, #20351 ),
 ( #59439, #29466 ),
 ( #76139, #76633 ),
 ( #13740, #36587 ),
 ( #20856, #43713 ),
 ( #37592, #52325 ),
 ( #60451, #82761 ),
 ( #51830, #13242 ),
 ( #75149, #6636 ),
 ( #74648, #91371 ),
 ( #5639, #21847 ),
 ( #52821, #68542 ),
 ( #99475, #14742 ),
 ( #82266, #45707 ),
 ( #23346, #9138 ),
 ( #2047, #8648 ),
 ( #24860, #38590 ) ),
 .UNSPECIFIED., .F., .F., .F.,
 ( 4, 1, 1, 1, 1, 1, 1, 1, 1, 1, 1, 1, 1, 1, 1, 1, 4 ),
 ( 2, 2 ),
 ( 0.000000000000000000, 0.05456394950705841657, 0.1078262027811427159, 0.1619237085214018657, 0.2175097010530381569, 0.2744983327961385555, 0.3348147646240177133, 0.3975549470643523486, 0.4647545773561987947, 0.5329012097695247085, 0.6000972138233301445, 0.6653541614565452456, 0.7310836277242112047, 0.7968834939590061506, 0.8632915901470210596, 0.9308312175092489094, 0.9999999999999998890 ),
 ( 0.000000000000000000, 1.000000000000000000 ),
 .UNSPECIFIED. ) ;
#32860 = EDGE_CURVE ( 'NONE', #36340, #47644, #68368, .T. ) ;
#32861 = CARTESIAN_POINT ( 'NONE',  ( -82.52287095715006160, -24.64898659630367916, 1.056161002820826145 ) ) ;
#32862 = DIRECTION ( 'NONE',  ( -3.773278334453079618E-23, 0.9999999999976377785, 2.173523156925979975E-06 ) ) ;
#32863 = ORIENTED_EDGE ( 'NONE', *, *, #59817, .T. ) ;
#32864 = ORIENTED_EDGE ( 'NONE', *, *, #45108, .F. ) ;
#32865 = LINE ( 'NONE', #79022, #41330 ) ;
#32866 = CARTESIAN_POINT ( 'NONE',  ( -42.49244915491595975, -24.35071581493542681, 9.817618358456037697 ) ) ;
#32867 = FACE_OUTER_BOUND ( 'NONE', #15228, .T. ) ;
#32869 = EDGE_LOOP ( 'NONE', ( #55047, #2983, #24214, #88159, #37870, #48295, #63047 ) ) ;
#32868 = CARTESIAN_POINT ( 'NONE',  ( 21.11370014442628218, -6.196533921283487345, 11.49999999999999645 ) ) ;
#32870 = ADVANCED_FACE ( 'NONE', ( #41167 ), #17315, .T. ) ;
#32871 = CARTESIAN_POINT ( 'NONE',  ( -103.5195659409635454, -23.73766607897670156, -1.055555164236454901 ) ) ;
#32872 = AXIS2_PLACEMENT_3D ( 'NONE', #94474, #15837, #24460 ) ;
#32873 = CARTESIAN_POINT ( 'NONE',  ( -14.53490578827140212, -17.26895500059623956, -1.500000000000002220 ) ) ;
#32874 = CARTESIAN_POINT ( 'NONE',  ( 20.92198360912786015, -1.804805560479522342, -1.500000000000002220 ) ) ;
#32875 = EDGE_CURVE ( 'NONE', #65785, #85381, #35998, .T. ) ;
#32877 = ORIENTED_EDGE ( 'NONE', *, *, #52595, .F. ) ;
#32876 = DIRECTION ( 'NONE',  ( -0.09824042138329590335, 4.470611911092166224E-17, -0.9951627101165078093 ) ) ;
#32878 = VECTOR ( 'NONE', #53516, 1000.000000000000114 ) ;
#32879 = ORIENTED_EDGE ( 'NONE', *, *, #58494, .T. ) ;
#32880 = CARTESIAN_POINT ( 'NONE',  ( -58.62287095715004881, -23.48786465467241769, 11.44779295918254824 ) ) ;
#32881 = CARTESIAN_POINT ( 'NONE',  ( 5.550000000000004263, -2.000000000000001776, 24.00000000000000000 ) ) ;
#32882 = ORIENTED_EDGE ( 'NONE', *, *, #30426, .F. ) ;
#32883 = CARTESIAN_POINT ( 'NONE',  ( 19.97935793590388442, -6.945280299276400449, 11.49999999999998934 ) ) ;
#32884 = DIRECTION ( 'NONE',  ( -6.134397492798446498E-16, 0.1087265912856350547, 0.9940716917543757081 ) ) ;
#32885 = CARTESIAN_POINT ( 'NONE',  ( -58.85737199502123929, -25.27183489919805126, 3.712349809207164952 ) ) ;
#32886 = CARTESIAN_POINT ( 'NONE',  ( -121.5564787168670051, -23.73766607897670866, -1.055555164236450905 ) ) ;
#32887 = CARTESIAN_POINT ( 'NONE',  ( -6.989144439031651501, -5.876774720514410077, 19.51167604195716621 ) ) ;
#32888 = CARTESIAN_POINT ( 'NONE',  ( -4.621320343559618848, 12.50000000000004974, 2.100000000000000089 ) ) ;
#32889 = CARTESIAN_POINT ( 'NONE',  ( 21.63176498729014341, 4.993826359924048219, -1.500000000000002220 ) ) ;
#32890 = CARTESIAN_POINT ( 'NONE',  ( -114.5945979628053948, -23.48783264082478794, -1.443836473390062380 ) ) ;
#32891 = ORIENTED_EDGE ( 'NONE', *, *, #64031, .F. ) ;
#32892 = CARTESIAN_POINT ( 'NONE',  ( 6.437068816671457583, 5.965225279485592225, -28.37834077173919667 ) ) ;
#32893 = CARTESIAN_POINT ( 'NONE',  ( -64.62287095715007013, -24.50321055353804311, 9.387540953477527594 ) ) ;
#32894 = CARTESIAN_POINT ( 'NONE',  ( -126.6248978461467516, -23.73766607897670156, -1.055555164236450016 ) ) ;
#32895 = CARTESIAN_POINT ( 'NONE',  ( -40.43756433397305727, -25.11033443737753501, 2.832404817301930056 ) ) ;
#32896 = CARTESIAN_POINT ( 'NONE',  ( 27.53860345374771867, -1.682774720514426114, -9.482392034746242260 ) ) ;
#32897 = VECTOR ( 'NONE', #69606, 1000.000000000000000 ) ;
#32898 = EDGE_CURVE ( 'NONE', #19646, #60374, #72621, .T. ) ;
#32899 = CARTESIAN_POINT ( 'NONE',  ( -15.31790942089943286, 12.02624123284522106, -1.500000000000002220 ) ) ;
#32900 = LOCAL_TIME ( 0, 54, 15.00000000000000000, #66878 ) ;
#32901 = CARTESIAN_POINT ( 'NONE',  ( 1.185105815240312888, -21.37944065014308848, 11.49999999999998934 ) ) ;
#32902 = DIRECTION ( 'NONE',  ( 0.000000000000000000, -1.000000000000000000, 0.000000000000000000 ) ) ;
#32903 = CARTESIAN_POINT ( 'NONE',  ( -100.6228709571500417, -24.15516710230295061, 10.28746687063725673 ) ) ;
#32904 = CARTESIAN_POINT ( 'NONE',  ( -77.58473169878783438, -24.51314013834315375, 0.6176544820404131775 ) ) ;
#32905 = CARTESIAN_POINT ( 'NONE',  ( 21.64774270073068863, 7.000884456547583845, -1.500000000000002220 ) ) ;
#32906 = AXIS2_PLACEMENT_3D ( 'NONE', #6457, #60757, #22160 ) ;
#32907 = CARTESIAN_POINT ( 'NONE',  ( -102.6335671968240177, -23.73766607897671932, -1.055555164236430477 ) ) ;
#32908 = CARTESIAN_POINT ( 'NONE',  ( -95.62287095715005592, -29.50250243563736774, 8.947779886222138046 ) ) ;
#32909 = CARTESIAN_POINT ( 'NONE',  ( 18.78741845327603599, -6.401996767227196905, 11.49999999999999645 ) ) ;
#32910 = CARTESIAN_POINT ( 'NONE',  ( -123.5542511647627322, -24.51419770103158768, 9.386484678747160970 ) ) ;
#32911 = VECTOR ( 'NONE', #28376, 1000.000000000000000 ) ;
#32912 = CARTESIAN_POINT ( 'NONE',  ( 8.071512145086499501, -1.000000000000008882, 3.746884140868834923 ) ) ;
#32913 = FACE_OUTER_BOUND ( 'NONE', #29341, .T. ) ;
#32914 = ORIENTED_EDGE ( 'NONE', *, *, #67221, .F. ) ;
#32915 = DIRECTION ( 'NONE',  ( -0.7071067811865507924, 0.000000000000000000, 0.7071067811865442421 ) ) ;
#32916 = DIRECTION ( 'NONE',  ( 0.000000000000000000, 0.000000000000000000, 1.000000000000000000 ) ) ;
#32917 = CARTESIAN_POINT ( 'NONE',  ( -71.52287095715007581, -23.47596703998600631, 11.44779298504228748 ) ) ;
#32918 = CARTESIAN_POINT ( 'NONE',  ( 4.495418090846292181, 21.21921847905042569, -1.500000000000002220 ) ) ;
#32919 = CARTESIAN_POINT ( 'NONE',  ( -56.64375666506161622, -23.96169478059713498, 10.65365249895718236 ) ) ;
#32920 = CARTESIAN_POINT ( 'NONE',  ( -8.384790838521158918, 17.58144419890746235, -1.500000000000002220 ) ) ;
#32921 = LINE ( 'NONE', #62891, #94456 ) ;
#32922 = ORIENTED_EDGE ( 'NONE', *, *, #43712, .F. ) ;
#32923 = CARTESIAN_POINT ( 'NONE',  ( -5.688044216684545518, -19.60349290560521140, 11.49999999999999645 ) ) ;
#32924 = LINE ( 'NONE', #26312, #94232 ) ;
#32925 = LINE ( 'NONE', #40034, #67486 ) ;
#32926 = EDGE_CURVE ( 'NONE', #19038, #82004, #99127, .T. ) ;
#32927 = ORIENTED_EDGE ( 'NONE', *, *, #92795, .T. ) ;
#32928 = CARTESIAN_POINT ( 'NONE',  ( -41.43253813893231552, -25.26941562057272606, 3.941780839177481788 ) ) ;
#32929 = CARTESIAN_POINT ( 'NONE',  ( 33.60454178612405229, 3.597323055450746487, -11.40641020892026170 ) ) ;
#32930 = CARTESIAN_POINT ( 'NONE',  ( -76.52287095715007581, -24.65952944569304606, 1.056160979905698794 ) ) ;
#32931 = CARTESIAN_POINT ( 'NONE',  ( 19.75748517575715368, 5.965225279485572685, 28.87153971905864580 ) ) ;
#32932 = CARTESIAN_POINT ( 'NONE',  ( 14.76093561896379214, -3.316774720514426456, -28.39148769130089889 ) ) ;
#32933 = CARTESIAN_POINT ( 'NONE',  ( -0.6703829557040261733, 4.102177322343280252, -3.549999999999999378 ) ) ;
#32934 = AXIS2_PLACEMENT_3D ( 'NONE', #71794, #49466, #2289 ) ;
#32935 = VERTEX_POINT ( 'NONE', #29419 ) ;
#32936 = EDGE_CURVE ( 'NONE', #1896, #32707, #73295, .T. ) ;
#32937 = CARTESIAN_POINT ( 'NONE',  ( 0.000000000000000000, -2.056774720514426669, 0.000000000000000000 ) ) ;
#32938 = EDGE_CURVE ( 'NONE', #45070, #87231, #29449, .T. ) ;
#32939 = EDGE_CURVE ( 'NONE', #78152, #64814, #52272, .T. ) ;
#32940 = CARTESIAN_POINT ( 'NONE',  ( 6.461317529299694051, 22.01590093704556850, 11.49999999999999645 ) ) ;
#32941 = CARTESIAN_POINT ( 'NONE',  ( -4.508144621425604903, 22.28865971958312997, -1.500000000000002220 ) ) ;
#32942 = ORIENTED_EDGE ( 'NONE', *, *, #69592, .T. ) ;
#32943 = CARTESIAN_POINT ( 'NONE',  ( -119.5228709571500616, -23.48783264082477018, -1.443836473390082142 ) ) ;
#32944 = VECTOR ( 'NONE', #54026, 1000.000000000000114 ) ;
#32945 = DIRECTION ( 'NONE',  ( -3.773278334453079618E-23, 0.9999999999976377785, 2.173523156925979975E-06 ) ) ;
#32946 = CARTESIAN_POINT ( 'NONE',  ( -90.64712176407903144, -23.48783264082477018, -1.443836473390091912 ) ) ;
#32947 = EDGE_CURVE ( 'NONE', #86308, #69912, #45690, .T. ) ;
#32948 = CARTESIAN_POINT ( 'NONE',  ( 13.59451591917074431, 3.316774720514426456, -28.23515841827053308 ) ) ;
#32949 = CARTESIAN_POINT ( 'NONE',  ( -69.54083733670222500, -24.51419770103157347, 9.386484678747178734 ) ) ;
#32950 = CARTESIAN_POINT ( 'NONE',  ( -26.13079664625181309, -24.93797848278802576, 4.224548870800117761 ) ) ;
#32951 = CARTESIAN_POINT ( 'NONE',  ( -90.52287095715009002, -23.48783264082477373, -1.443836473390088582 ) ) ;
#32952 = CARTESIAN_POINT ( 'NONE',  ( -2.243088942307695177, -6.376774720514408301, 19.14743589743590491 ) ) ;
#32953 = ORIENTED_EDGE ( 'NONE', *, *, #21354, .T. ) ;
#32954 = CARTESIAN_POINT ( 'NONE',  ( -9.549598871097368047, 18.00506641634745009, 11.49999999999998934 ) ) ;
#32955 = ORIENTED_EDGE ( 'NONE', *, *, #62733, .F. ) ;
#32956 = EDGE_LOOP ( 'NONE', ( #75898, #61590, #62534, #96893 ) ) ;
#32957 = EDGE_CURVE ( 'NONE', #6738, #37215, #52894, .T. ) ;
#32958 = CARTESIAN_POINT ( 'NONE',  ( -15.77545706029219730, -16.76941864122914083, 11.49999999999998934 ) ) ;
#32959 = CARTESIAN_POINT ( 'NONE',  ( -1.438454482798693146, -6.376774720514410077, 19.55848054040323092 ) ) ;
#32960 = ORIENTED_EDGE ( 'NONE', *, *, #42529, .T. ) ;
#32961 = PLANE ( 'NONE',  #84992 ) ;
#32962 = CARTESIAN_POINT ( 'NONE',  ( 22.02124265030973760, -6.143225279485574397, 16.20402280011862217 ) ) ;
#32963 = AXIS2_PLACEMENT_3D ( 'NONE', #27311, #3983, #73988 ) ;
#32964 = EDGE_CURVE ( 'NONE', #68064, #99675, #5090, .T. ) ;
#32965 = CARTESIAN_POINT ( 'NONE',  ( -58.87764846857956513, -25.14083923594470704, 2.947789366366647901 ) ) ;
#32966 = FACE_OUTER_BOUND ( 'NONE', #50811, .T. ) ;
#32968 = EDGE_LOOP ( 'NONE', ( #50939, #850, #58038, #65121 ) ) ;
#32967 = CARTESIAN_POINT ( 'NONE',  ( -18.01091527469349529, -11.40912366963296698, 11.49999999999999645 ) ) ;
#32969 = ORIENTED_EDGE ( 'NONE', *, *, #24180, .F. ) ;
#32970 = CARTESIAN_POINT ( 'NONE',  ( 6.060481786824854389, 21.40074245971799627, 11.49999999999998934 ) ) ;
#32971 = CARTESIAN_POINT ( 'NONE',  ( -15.52656095410427817, -13.64048245868121434, 11.49999999999998934 ) ) ;
#32972 = EDGE_CURVE ( 'NONE', #29423, #40078, #4567, .T. ) ;
#32974 = VERTEX_POINT ( 'NONE', #20300 ) ;
#32973 = AXIS2_PLACEMENT_3D ( 'NONE', #38772, #47902, #16427 ) ;
#32975 = DIRECTION ( 'NONE',  ( -1.000000000000000000, 0.000000000000000000, 0.000000000000000000 ) ) ;
#32976 = FACE_BOUND ( 'NONE', #61444, .T. ) ;
#32977 = ORIENTED_EDGE ( 'NONE', *, *, #69583, .F. ) ;
#32978 = CARTESIAN_POINT ( 'NONE',  ( -79.55620429048337883, -23.48786465467241058, 11.44779295918254469 ) ) ;
#32979 = ORIENTED_EDGE ( 'NONE', *, *, #94823, .F. ) ;
#32980 = VECTOR ( 'NONE', #1188, 1000.000000000000114 ) ;
#32981 = CARTESIAN_POINT ( 'NONE',  ( -58.58749944175303170, -24.35071581493543036, 9.817618358456028815 ) ) ;
#32982 = CARTESIAN_POINT ( 'NONE',  ( -7.326923076923076650, -5.876774720514418071, 20.36318108974359831 ) ) ;
#32983 = CARTESIAN_POINT ( 'NONE',  ( -2.238888094254589234, -20.74146561784671761, -1.500000000000002220 ) ) ;
#32984 = CARTESIAN_POINT ( 'NONE',  ( 16.27406392464308027, 14.57352745747340172, 11.49999999999999645 ) ) ;
#32985 = EDGE_CURVE ( 'NONE', #57426, #35959, #75092, .T. ) ;
#32986 = CARTESIAN_POINT ( 'NONE',  ( -73.63047128846197609, -24.35071581493543036, 9.817618358456027039 ) ) ;
#32987 = CYLINDRICAL_SURFACE ( 'NONE', #35384, 1.999999999999999112 ) ;
#32988 = CARTESIAN_POINT ( 'NONE',  ( -20.52357230491503159, 9.176553703681571861, 11.49999999999998934 ) ) ;
#32989 = EDGE_CURVE ( 'NONE', #65105, #18022, #8462, .T. ) ;
#32990 = CARTESIAN_POINT ( 'NONE',  ( -118.5222382631839650, -23.48786465467241769, 11.44779295918253581 ) ) ;
#32991 = DIRECTION ( 'NONE',  ( -0.000000000000000000, 1.000000000000000000, -0.000000000000000000 ) ) ;
#32992 = CARTESIAN_POINT ( 'NONE',  ( 3.825380556292953482, -5.876774720514427841, 21.83927723428477208 ) ) ;
#32993 = ORIENTED_EDGE ( 'NONE', *, *, #95965, .T. ) ;
#32994 = VERTEX_POINT ( 'NONE', #29922 ) ;
#32995 = ORIENTED_EDGE ( 'NONE', *, *, #19735, .T. ) ;
#32996 = DIRECTION ( 'NONE',  ( -1.000000000000000000, -0.000000000000000000, -0.000000000000000000 ) ) ;
#32997 = ORIENTED_EDGE ( 'NONE', *, *, #65508, .T. ) ;
#32998 = CARTESIAN_POINT ( 'NONE',  ( 16.75108703964928480, -13.32659110743468212, -1.500000000000002220 ) ) ;
#32999 = CARTESIAN_POINT ( 'NONE',  ( -19.80502325505778671, 10.42642913751328670, 11.49999999999999645 ) ) ;
#33000 = ORIENTED_EDGE ( 'NONE', *, *, #5717, .T. ) ;
#33001 = CARTESIAN_POINT ( 'NONE',  ( -68.55620429048339304, -24.65952944569304606, 1.056160979905698794 ) ) ;
#33002 = CARTESIAN_POINT ( 'NONE',  ( 17.02745815656931683, -12.38318283856952107, -1.500000000000002220 ) ) ;
#33003 = CARTESIAN_POINT ( 'NONE',  ( -30.52452761580430263, -25.14647750993875519, 7.291421475381018702 ) ) ;
#33004 = CARTESIAN_POINT ( 'NONE',  ( -11.57717615966994273, 16.22069937712612031, -1.500000000000002220 ) ) ;
#33005 = CARTESIAN_POINT ( 'NONE',  ( -123.5228709571500616, -29.50248528299804818, 1.056150453629045360 ) ) ;
#33006 = CARTESIAN_POINT ( 'NONE',  ( -80.61306835763387824, -25.30877077354806914, 4.525992615401982277 ) ) ;
#33007 = CARTESIAN_POINT ( 'NONE',  ( 18.76863814860013235, 11.56883167669432133, -1.500000000000002220 ) ) ;
#33008 = VERTEX_POINT ( 'NONE', #44659 ) ;
#33009 = CARTESIAN_POINT ( 'NONE',  ( -65.53967300336732649, -24.63419186844611275, 9.035850630976918652 ) ) ;
#33010 = AXIS2_PLACEMENT_3D ( 'NONE', #29118, #11903, #81916 ) ;
#33011 = FACE_OUTER_BOUND ( 'NONE', #97005, .T. ) ;
#33012 = CARTESIAN_POINT ( 'NONE',  ( -20.82246440549779720, 1.468558417816581807, 11.49999999999999645 ) ) ;
#33013 = CARTESIAN_POINT ( 'NONE',  ( 29.64448763235240136, -5.625929005037784592, 28.17618604274316851 ) ) ;
#33014 = VECTOR ( 'NONE', #95227, 1000.000000000000114 ) ;
#33015 = DIRECTION ( 'NONE',  ( 0.000000000000000000, -0.9999999999976377785, -2.173523156925979975E-06 ) ) ;
#33016 = CARTESIAN_POINT ( 'NONE',  ( -127.5562042904834215, -23.48783264082479505, -1.443836473390056829 ) ) ;
#33017 = CARTESIAN_POINT ( 'NONE',  ( -21.31669061289120037, -0.5855882196083471714, -1.500000000000002220 ) ) ;
#33018 = CARTESIAN_POINT ( 'NONE',  ( -104.5228709571500758, -24.66019654487200441, 8.947790411086113949 ) ) ;
#33019 = CARTESIAN_POINT ( 'NONE',  ( -50.81798825283360799, -25.20438501375636875, 3.361021725245152858 ) ) ;
#33020 = CARTESIAN_POINT ( 'NONE',  ( -31.62287095715005236, -23.47596703998600276, 11.44779298504227505 ) ) ;
#33021 = CARTESIAN_POINT ( 'NONE',  ( -69.99162906124911387, -25.30188801935125653, 5.302352381037461093 ) ) ;
#33022 = CARTESIAN_POINT ( 'NONE',  ( -17.80605238980536953, 13.89162706601689479, -1.500000000000002220 ) ) ;
#33023 = CARTESIAN_POINT ( 'NONE',  ( -123.5895376238167245, -24.64898659630368627, 1.056161002820393158 ) ) ;
#33024 = ORIENTED_EDGE ( 'NONE', *, *, #21122, .F. ) ;
#33025 = DIRECTION ( 'NONE',  ( 2.439088438507244272E-15, -7.805083003223181985E-15, 1.000000000000000000 ) ) ;
#33026 = CARTESIAN_POINT ( 'NONE',  ( -31.65061454106520600, -23.96169478059712432, 10.65365249895719124 ) ) ;
#33027 = CARTESIAN_POINT ( 'NONE',  ( 9.442166470422634461, 17.27452087139410963, 11.49999999999999645 ) ) ;
#33028 = CARTESIAN_POINT ( 'NONE',  ( 1.255616527394258553, 17.95615290467683778, 9.000000000000000000 ) ) ;
#33029 = FACE_OUTER_BOUND ( 'NONE', #51558, .T. ) ;
#33030 = VERTEX_POINT ( 'NONE', #89337 ) ;
#33031 = CARTESIAN_POINT ( 'NONE',  ( -56.52287095715006870, -24.64898659630367916, 1.056161002820822592 ) ) ;
#33032 = CARTESIAN_POINT ( 'NONE',  ( -83.62287095715007013, -23.48786465467241769, 11.44779295918254469 ) ) ;
#33033 = DIRECTION ( 'NONE',  ( -0.1593164160933055740, 0.000000000000000000, 0.9872275723272646575 ) ) ;
#33034 = CARTESIAN_POINT ( 'NONE',  ( 5.097264368844747651, 3.299463065352477908, -27.56135813788838718 ) ) ;
#33035 = CARTESIAN_POINT ( 'NONE',  ( -81.62287095715005592, -29.50250243563736774, 8.947779886222141599 ) ) ;
#33036 = CYLINDRICAL_SURFACE ( 'NONE', #83732, 0.8160000000000007248 ) ;
#33037 = CARTESIAN_POINT ( 'NONE',  ( 17.61170953066113398, -8.936083093766256980, 11.49999999999998934 ) ) ;
#33038 = ORIENTED_EDGE ( 'NONE', *, *, #5033, .F. ) ;
#33039 = CARTESIAN_POINT ( 'NONE',  ( -11.13811422090317294, 16.88724661786912762, 11.49999999999999645 ) ) ;
#33040 = CARTESIAN_POINT ( 'NONE',  ( -112.6228709571500275, -24.51387760970725083, 9.387446482453412955 ) ) ;
#33041 = CIRCLE ( 'NONE', #11955, 3.060000000000000053 ) ;
#33042 = EDGE_LOOP ( 'NONE', ( #12736, #39353, #27115, #75126 ) ) ;
#33043 = CARTESIAN_POINT ( 'NONE',  ( -110.6228709571500701, -23.48783264082479505, -1.443836473390060160 ) ) ;
#33044 = CARTESIAN_POINT ( 'NONE',  ( -69.34448478228789270, -25.25183673717061694, 6.146172466399267620 ) ) ;
#33045 = CARTESIAN_POINT ( 'NONE',  ( -51.46011314183329688, -25.27661340440378623, 5.843653433976077949 ) ) ;
#33046 = DIRECTION ( 'NONE',  ( 0.000000000000000000, 0.9999999999976377785, 2.173523156925979128E-06 ) ) ;
#33047 = EDGE_CURVE ( 'NONE', #48489, #60457, #44458, .T. ) ;
#33048 = CARTESIAN_POINT ( 'NONE',  ( 8.160000000000000142, 8.786681894035815787, 6.233837718258663507 ) ) ;
#33049 = AXIS2_PLACEMENT_3D ( 'NONE', #75056, #28390, #5557 ) ;
#33050 = ADVANCED_FACE ( 'NONE', ( #82710 ), #27932, .F. ) ;
#33051 = B_SPLINE_CURVE_WITH_KNOTS ( 'NONE', 3,
 ( #36665, #29047, #60022, #90949 ),
 .UNSPECIFIED., .F., .F.,
 ( 4, 4 ),
 ( 0.000000000000000000, 0.0001002978970080628312 ),
 .UNSPECIFIED. ) ;
#33052 = CARTESIAN_POINT ( 'NONE',  ( -96.52287095715004739, -23.96127896941631974, -0.6493128931037976947 ) ) ;
#33053 = CARTESIAN_POINT ( 'NONE',  ( -1.591348192139008466, -19.94584644712825039, -1.500000000000002220 ) ) ;
#33054 = EDGE_CURVE ( 'NONE', #45090, #37127, #62605, .T. ) ;
#33055 = CARTESIAN_POINT ( 'NONE',  ( 3.509873074917118085, 5.965225279485572685, 29.15869884040363758 ) ) ;
#33056 = CARTESIAN_POINT ( 'NONE',  ( -116.5196406133853628, -23.96169478059713853, 10.65365249895717348 ) ) ;
#33057 = VERTEX_POINT ( 'NONE', #12194 ) ;
#33058 = EDGE_CURVE ( 'NONE', #46936, #55690, #58889, .T. ) ;
#33059 = ADVANCED_FACE ( 'NONE', ( #67014 ), #13187, .T. ) ;
#33060 = CARTESIAN_POINT ( 'NONE',  ( -79.54043201964276477, -24.66019654487199375, 8.947790411086119278 ) ) ;
#33061 = CARTESIAN_POINT ( 'NONE',  ( -35.48816746163671354, -24.40034930558991277, 0.3402023900116170063 ) ) ;
#33062 = CARTESIAN_POINT ( 'NONE',  ( -79.88885947674448573, -25.30549239610902390, 5.065442659042057372 ) ) ;
#33063 = DIRECTION ( 'NONE',  ( -0.000000000000000000, -1.000000000000000000, -0.000000000000000000 ) ) ;
#33064 = CARTESIAN_POINT ( 'NONE',  ( -84.62287095715005592, -29.50247984919015209, -1.443849546365053582 ) ) ;
#33065 = B_SPLINE_CURVE_WITH_KNOTS ( 'NONE', 3,
 ( #78011, #40478, #8523, #71431, #94752, #39969, #79529, #39473 ),
 .UNSPECIFIED., .F., .F.,
 ( 4, 2, 2, 4 ),
 ( 6.384118678600685898E-06, 0.002007151183507250615, 0.003007534715921577739, 0.004007918248335903995 ),
 .UNSPECIFIED. ) ;
#33066 = FACE_OUTER_BOUND ( 'NONE', #27465, .T. ) ;
#33067 = CARTESIAN_POINT ( 'NONE',  ( -49.88931575556473064, -25.19893203316160779, 3.394471111229040883 ) ) ;
#33068 = ORIENTED_EDGE ( 'NONE', *, *, #72028, .F. ) ;
#33069 = CARTESIAN_POINT ( 'NONE',  ( 19.35245777310151993, -6.127589836641541332, 11.49999999999998934 ) ) ;
#33070 = CARTESIAN_POINT ( 'NONE',  ( 31.68607835968445485, 4.403148666511627951, 29.28367637967570758 ) ) ;
#33071 = CARTESIAN_POINT ( 'NONE',  ( -34.47821653490140648, -24.65952944569304606, 1.056160979905694353 ) ) ;
#33072 = CARTESIAN_POINT ( 'NONE',  ( -107.5228709571500900, -24.51387760970725793, 9.387446482453409402 ) ) ;
#33073 = VERTEX_POINT ( 'NONE', #93313 ) ;
#33074 = CARTESIAN_POINT ( 'NONE',  ( -83.52287095715006160, -23.48786465467241769, 11.44779295918254469 ) ) ;
#33075 = EDGE_CURVE ( 'NONE', #68625, #73282, #40856, .T. ) ;
#33076 = AXIS2_PLACEMENT_3D ( 'NONE', #22564, #44444, #68275 ) ;
#33077 = CARTESIAN_POINT ( 'NONE',  ( -14.54676392617323266, -15.37779485849079464, 11.49999999999999645 ) ) ;
#33078 = CARTESIAN_POINT ( 'NONE',  ( 22.15222936869060177, 0.07132910108538677296, -1.500000000000002220 ) ) ;
#33079 = CARTESIAN_POINT ( 'NONE',  ( 18.12345787009687115, -9.690629616749632191, 11.49999999999998934 ) ) ;
#33080 = ORIENTED_EDGE ( 'NONE', *, *, #56427, .T. ) ;
#33081 = DIRECTION ( 'NONE',  ( 0.000000000000000000, 2.173523156925980399E-06, -0.9999999999976378895 ) ) ;
#33082 = ORIENTED_EDGE ( 'NONE', *, *, #9310, .T. ) ;
#33083 = CARTESIAN_POINT ( 'NONE',  ( -54.58739168452969892, -24.34968618360932879, 0.1864209137778771175 ) ) ;
#33084 = CARTESIAN_POINT ( 'NONE',  ( -85.92287095715006728, -23.47593901973090169, -1.443836447538997092 ) ) ;
#33085 = ORIENTED_EDGE ( 'NONE', *, *, #2142, .F. ) ;
#33086 = EDGE_LOOP ( 'NONE', ( #82157, #53953, #77529, #54315 ) ) ;
#33087 = ORIENTED_EDGE ( 'NONE', *, *, #76000, .F. ) ;
#33088 = CARTESIAN_POINT ( 'NONE',  ( -112.6228709571500417, -24.51283580621365843, 0.6167428607019777020 ) ) ;
#33089 = CARTESIAN_POINT ( 'NONE',  ( 6.658651924251966392, -6.376774720514415407, 20.11748569626183425 ) ) ;
#33090 = CARTESIAN_POINT ( 'NONE',  ( 5.495499487697820484, -6.376774720514418959, 20.18701882043406926 ) ) ;
#33091 = CARTESIAN_POINT ( 'NONE',  ( 18.79598114143782084, -8.675585332008726169, -1.500000000000002220 ) ) ;
#33092 = CARTESIAN_POINT ( 'NONE',  ( 2.186256072416925544, -21.55203199515037582, 11.49999999999999645 ) ) ;
#33093 = ORIENTED_EDGE ( 'NONE', *, *, #41956, .T. ) ;
#33094 = CARTESIAN_POINT ( 'NONE',  ( -60.52287095715006160, -23.48786465467241058, 11.44779295918254824 ) ) ;
#33095 = DIRECTION ( 'NONE',  ( -3.773278334453079618E-23, 0.9999999999976377785, 2.173523156925979975E-06 ) ) ;
#33096 = CARTESIAN_POINT ( 'NONE',  ( 18.65981798208652265, 12.38953945867474360, -1.500000000000002220 ) ) ;
#33097 = ADVANCED_FACE ( 'NONE', ( #55279 ), #70494, .T. ) ;
#33098 = DIRECTION ( 'NONE',  ( 3.773278334444167608E-23, -1.000000000000000000, 0.000000000000000000 ) ) ;
#33099 = CARTESIAN_POINT ( 'NONE',  ( 13.10664265030973930, 1.324225279485583551, -28.18129937516353678 ) ) ;
#33100 = ORIENTED_EDGE ( 'NONE', *, *, #7526, .F. ) ;
#33101 = CARTESIAN_POINT ( 'NONE',  ( 29.61836285113398048, 5.182350003425200136, 28.59212231372686119 ) ) ;
#33102 = CARTESIAN_POINT ( 'NONE',  ( -100.5228709571500900, -23.48783264082477018, -1.443836473390086583 ) ) ;
#33103 = VERTEX_POINT ( 'NONE', #77583 ) ;
#33104 = ORIENTED_EDGE ( 'NONE', *, *, #53083, .T. ) ;
#33105 = EDGE_CURVE ( 'NONE', #40854, #46960, #1490, .T. ) ;
#33106 = DIRECTION ( 'NONE',  ( -3.773278334453079618E-23, 0.9999999999976377785, 2.173523156925979975E-06 ) ) ;
#33107 = EDGE_LOOP ( 'NONE', ( #12325, #20356, #35249, #97269 ) ) ;
#33108 = DIRECTION ( 'NONE',  ( 0.000000000000000000, 0.000000000000000000, -1.000000000000000000 ) ) ;
#33109 = CARTESIAN_POINT ( 'NONE',  ( -3.247986963444697395, 20.98610878802851332, -1.500000000000002220 ) ) ;
#33110 = VERTEX_POINT ( 'NONE', #61393 ) ;
#33111 = CARTESIAN_POINT ( 'NONE',  ( -50.63203686936204662, -24.73486907724918282, 1.287355809206965684 ) ) ;
#33112 = CARTESIAN_POINT ( 'NONE',  ( -19.95566455537076678, 8.849265345510103131, 11.49999999999998934 ) ) ;
#33113 = CARTESIAN_POINT ( 'NONE',  ( -52.59321787669466630, -24.15620529776627734, 10.23563542870661003 ) ) ;
#33114 = CARTESIAN_POINT ( 'NONE',  ( -107.5228709571500616, -24.33832256527048798, 0.1851278514138657294 ) ) ;
#33115 = FACE_OUTER_BOUND ( 'NONE', #67545, .T. ) ;
#33116 = CARTESIAN_POINT ( 'NONE',  ( 12.66425630052701479, 17.85959152241435177, -1.500000000000002220 ) ) ;
#33117 = CARTESIAN_POINT ( 'NONE',  ( -30.57287095715006942, -24.99131595220528368, 7.800444815679671073 ) ) ;
#33118 = ORIENTED_EDGE ( 'NONE', *, *, #2081, .T. ) ;
#33119 = DIRECTION ( 'NONE',  ( 0.000000000000000000, -1.000000000000000000, 0.000000000000000000 ) ) ;
#33120 = CARTESIAN_POINT ( 'NONE',  ( -85.54876333844239866, -24.40133493613049964, 9.663955038902802386 ) ) ;
#33121 = EDGE_LOOP ( 'NONE', ( #11369, #28877, #5185, #69294 ) ) ;
#33122 = VERTEX_POINT ( 'NONE', #86213 ) ;
#33123 = ORIENTED_EDGE ( 'NONE', *, *, #27924, .F. ) ;
#33124 = LINE ( 'NONE', #85911, #92912 ) ;
#33125 = DIRECTION ( 'NONE',  ( -1.000000000000000000, 0.000000000000000000, -0.000000000000000000 ) ) ;
#33126 = CARTESIAN_POINT ( 'NONE',  ( -17.82860346875387947, 11.52481846644873187, 11.49999999999998934 ) ) ;
#33127 = DIRECTION ( 'NONE',  ( -0.000000000000000000, 1.000000000000000000, -0.000000000000000000 ) ) ;
#33128 = LINE ( 'NONE', #18897, #70585 ) ;
#33129 = AXIS2_PLACEMENT_3D ( 'NONE', #48788, #40664, #56404 ) ;
#33130 = CARTESIAN_POINT ( 'NONE',  ( 29.73860345376319358, 4.772789318458390717, -4.021180035034620737 ) ) ;
#33131 = LINE ( 'NONE', #62095, #58906 ) ;
#33132 = CARTESIAN_POINT ( 'NONE',  ( 15.36829964806744364, -11.83880051060199712, 11.49999999999998934 ) ) ;
#33133 = CARTESIAN_POINT ( 'NONE',  ( -45.48769855799984896, -24.52300882791528380, 0.6510814631126234930 ) ) ;
#33134 = ORIENTED_EDGE ( 'NONE', *, *, #37851, .T. ) ;
#33135 = CARTESIAN_POINT ( 'NONE',  ( -1.081029368968937421, 19.50181592447522050, 11.49999999999999645 ) ) ;
#33136 = CARTESIAN_POINT ( 'NONE',  ( 31.63608488009066733, -3.316774720514426456, 27.34773273846990094 ) ) ;
#33137 = CARTESIAN_POINT ( 'NONE',  ( -107.5562042904834072, -24.65952944569304961, 1.056160979905703456 ) ) ;
#33138 = ORIENTED_EDGE ( 'NONE', *, *, #25130, .F. ) ;
#33139 = VECTOR ( 'NONE', #73412, 1000.000000000000114 ) ;
#33140 = CARTESIAN_POINT ( 'NONE',  ( 4.967622410992271753, -5.876774720514415407, 20.05703257908297843 ) ) ;
#33141 = CARTESIAN_POINT ( 'NONE',  ( -119.5228709571500758, -24.64965694238408034, 8.947790433994191162 ) ) ;
#33142 = DIRECTION ( 'NONE',  ( 0.000000000000000000, 0.000000000000000000, -1.000000000000000000 ) ) ;
#33143 = CARTESIAN_POINT ( 'NONE',  ( -80.77473702827948898, -25.24813986770818630, 7.542257150238226515 ) ) ;
#33144 = CARTESIAN_POINT ( 'NONE',  ( 14.19269941865516671, -13.59168563846684563, -1.500000000000002220 ) ) ;
#33145 = ORIENTED_EDGE ( 'NONE', *, *, #48402, .F. ) ;
#33146 = DIRECTION ( 'NONE',  ( 3.773278334444167608E-23, -1.000000000000000000, 0.000000000000000000 ) ) ;
#33147 = CARTESIAN_POINT ( 'NONE',  ( 8.286623624103266097E-13, -23.05000000000000426, -1.500000000000002220 ) ) ;
#33148 = CALENDAR_DATE ( 2026, 9, 10 ) ;
#33149 = CARTESIAN_POINT ( 'NONE',  ( 7.749999999999998224, 24.84999999999999787, 0.000000000000000000 ) ) ;
#33150 = FACE_OUTER_BOUND ( 'NONE', #98888, .T. ) ;
#33151 = CARTESIAN_POINT ( 'NONE',  ( -40.52287095715005449, -29.50249982740957577, 7.747779886224967605 ) ) ;
#33152 = LINE ( 'NONE', #48897, #47697 ) ;
#33153 = CARTESIAN_POINT ( 'NONE',  ( -81.90251867898965088, -25.27183487616304447, 3.712349674769177987 ) ) ;
#33154 = EDGE_CURVE ( 'NONE', #1499, #82473, #32719, .T. ) ;
#33155 = PLANE ( 'NONE',  #87917 ) ;
#33156 = CARTESIAN_POINT ( 'NONE',  ( -73.52287095715004739, -24.35013146730203815, 9.818937971375099494 ) ) ;
#33157 = CARTESIAN_POINT ( 'NONE',  ( -48.87380231474225667, -25.25252557466923520, 6.137092008254006359 ) ) ;
#33158 = CARTESIAN_POINT ( 'NONE',  ( -10.29545327866581950, 17.06371652956568852, -1.500000000000002220 ) ) ;
#33159 = EDGE_CURVE ( 'NONE', #53307, #67032, #24311, .T. ) ;
#33160 = DIRECTION ( 'NONE',  ( 3.773278334444166432E-23, -1.000000000000000000, 0.000000000000000000 ) ) ;
#33161 = CARTESIAN_POINT ( 'NONE',  ( 1.822157996128044299, -19.77364354024053839, -1.500000000000002220 ) ) ;
#33162 = ORIENTED_EDGE ( 'NONE', *, *, #69819, .F. ) ;
#33163 = DIRECTION ( 'NONE',  ( 0.000000000000000000, 0.9999999999976377785, 2.173523156925979975E-06 ) ) ;
#33164 = ADVANCED_FACE ( 'NONE', ( #53274 ), #43475, .T. ) ;
#33165 = ADVANCED_FACE ( 'NONE', ( #49174 ), #95821, .F. ) ;
#33166 = CARTESIAN_POINT ( 'NONE',  ( 17.51792015816173986, 5.965225279485572685, 29.01255224319336889 ) ) ;
#33167 = VECTOR ( 'NONE', #84253, 1000.000000000000114 ) ;
#33168 = CARTESIAN_POINT ( 'NONE',  ( -42.62287095715004881, -24.64965695001467694, 8.947790433994187609 ) ) ;
#33169 = CARTESIAN_POINT ( 'NONE',  ( -2.730994233912177549, 20.60462238790213618, 11.49999999999999645 ) ) ;
#33170 = CARTESIAN_POINT ( 'NONE',  ( -81.64591219847839909, -23.48783264082478084, -1.443836473390067043 ) ) ;
#33171 = EDGE_CURVE ( 'NONE', #5284, #60317, #63897, .T. ) ;
#33172 = DIRECTION ( 'NONE',  ( -3.773278334453080206E-23, 0.9999999999976377785, 2.173523156925979975E-06 ) ) ;
#33173 = CARTESIAN_POINT ( 'NONE',  ( -9.359374538088376383, 20.77767741201286711, 11.49999999999999645 ) ) ;
#33174 = ORIENTED_EDGE ( 'NONE', *, *, #85670, .T. ) ;
#33175 = CARTESIAN_POINT ( 'NONE',  ( -112.5228709571500616, -23.47596703998600631, 11.44779298504228038 ) ) ;
#33176 = DIRECTION ( 'NONE',  ( 0.000000000000000000, -1.000000000000000000, 0.000000000000000000 ) ) ;
#33177 = ORIENTED_EDGE ( 'NONE', *, *, #64884, .F. ) ;
#33178 = CARTESIAN_POINT ( 'NONE',  ( -20.14672940031187665, -1.731937678239350298, 11.49999999999998934 ) ) ;
#33179 = EDGE_CURVE ( 'NONE', #20076, #52968, #71700, .T. ) ;
#33180 = CARTESIAN_POINT ( 'NONE',  ( -106.5228709571501327, -24.35013146730203815, 9.818937971375095941 ) ) ;
#33181 = CARTESIAN_POINT ( 'NONE',  ( -110.5228709571500332, -24.63345952396256422, 9.038047939301501188 ) ) ;
#33182 = EDGE_CURVE ( 'NONE', #57678, #60428, #17703, .T. ) ;
#33183 = CARTESIAN_POINT ( 'NONE',  ( 8.000000000000007105, -6.376774720514426953, 17.49999999999999645 ) ) ;
#33184 = ORIENTED_EDGE ( 'NONE', *, *, #19191, .F. ) ;
#33185 = DIRECTION ( 'NONE',  ( 0.5630016722799275897, -7.885106708985486076E-16, -0.8264557562326038109 ) ) ;
#33186 = B_SPLINE_CURVE_WITH_KNOTS ( 'NONE', 3,
 ( #78529, #30872, #55730, #46610 ),
 .UNSPECIFIED., .F., .F.,
 ( 4, 4 ),
 ( 0.000000000000000000, 1.000000000000000000 ),
 .UNSPECIFIED. ) ;
#33187 = CARTESIAN_POINT ( 'NONE',  ( -100.6228709571501128, -24.14321612903118464, -0.2833117244521107247 ) ) ;
#33188 = CARTESIAN_POINT ( 'NONE',  ( -19.87929632332335927, 2.386914507623989490, -1.500000000000002220 ) ) ;
#33189 = DIRECTION ( 'NONE',  ( 0.000000000000000000, 0.000000000000000000, 1.000000000000000000 ) ) ;
#33190 = CARTESIAN_POINT ( 'NONE',  ( -16.09219062524700661, 13.46031615953476468, 11.49999999999999645 ) ) ;
#33191 = CARTESIAN_POINT ( 'NONE',  ( 0.000000000000000000, 0.000000000000000000, 9.000000000000000000 ) ) ;
#33192 = CARTESIAN_POINT ( 'NONE',  ( -70.62368314357276233, -25.00182538069146787, 7.747789668545044250 ) ) ;
#33193 = CARTESIAN_POINT ( 'NONE',  ( -0.5447568859041533873, -22.05808898580190558, -1.500000000000002220 ) ) ;
#33194 = AXIS2_PLACEMENT_3D ( 'NONE', #80228, #57415, #65534 ) ;
#33195 = CARTESIAN_POINT ( 'NONE',  ( -59.52287095715009002, -23.47593901973090524, -1.443836447538997092 ) ) ;
#33196 = ORIENTED_EDGE ( 'NONE', *, *, #100143, .F. ) ;
#33197 = PLANE ( 'NONE',  #20841 ) ;
#33198 = LINE ( 'NONE', #54542, #20115 ) ;
#33199 = CARTESIAN_POINT ( 'NONE',  ( -72.52211250399544440, -23.48783264082477018, -1.443836473390095021 ) ) ;
#33200 = ORIENTED_EDGE ( 'NONE', *, *, #19968, .T. ) ;
#33201 = CARTESIAN_POINT ( 'NONE',  ( -92.62287095715005592, -23.47596703998600631, 11.44779298504227860 ) ) ;
#33202 = ORIENTED_EDGE ( 'NONE', *, *, #2856, .F. ) ;
#33203 = ORIENTED_EDGE ( 'NONE', *, *, #13158, .T. ) ;
#33204 = CARTESIAN_POINT ( 'NONE',  ( -79.52287095715010423, -23.47593901973090524, -1.443836447538996870 ) ) ;
#33205 = LINE ( 'NONE', #1765, #22713 ) ;
#33206 = CARTESIAN_POINT ( 'NONE',  ( -4.968349358974360364, -5.876774720514411854, 19.46153846153846700 ) ) ;
#33207 = CARTESIAN_POINT ( 'NONE',  ( -11.60840874443078263, -16.91462557209307960, -1.500000000000002220 ) ) ;
#33208 = ADVANCED_FACE ( 'NONE', ( #19190 ), #80596, .F. ) ;
#33209 = CIRCLE ( 'NONE', #60753, 3.500000000000000000 ) ;
#33210 = VERTEX_POINT ( 'NONE', #80099 ) ;
#33211 = CARTESIAN_POINT ( 'NONE',  ( -99.63518257809350587, -25.29661202606573411, 5.472634000556907630 ) ) ;
#33212 = CARTESIAN_POINT ( 'NONE',  ( 7.155337544004596317, -5.876774720514418071, 20.64714842558261765 ) ) ;
#33213 = CARTESIAN_POINT ( 'NONE',  ( 9.950000000000006395, 0.000000000000000000, 19.30000000000000071 ) ) ;
#33214 = CARTESIAN_POINT ( 'NONE',  ( -18.01732314745861530, 13.19606014829601826, -1.500000000000002220 ) ) ;
#33215 = CARTESIAN_POINT ( 'NONE',  ( -111.6228709571500559, -24.64965695001468404, 8.947790433994176951 ) ) ;
#33216 = DIRECTION ( 'NONE',  ( 1.000000000000000000, 3.773278334444166432E-23, 8.201307841325785021E-29 ) ) ;
#33217 = VERTEX_POINT ( 'NONE', #10089 ) ;
#33218 = CARTESIAN_POINT ( 'NONE',  ( -101.6228709571500559, -23.48783264082479505, -1.443836473390062380 ) ) ;
#33219 = CARTESIAN_POINT ( 'NONE',  ( 22.81105451610979173, 1.682774720514426114, -18.46691820600746681 ) ) ;
#33220 = CARTESIAN_POINT ( 'NONE',  ( -13.77211689728001964, -15.67653869864640903, -1.500000000000002220 ) ) ;
#33221 = ORIENTED_EDGE ( 'NONE', *, *, #59514, .F. ) ;
#33223 = ORIENTED_EDGE ( 'NONE', *, *, #61418, .T. ) ;
#33222 = FACE_OUTER_BOUND ( 'NONE', #97832, .T. ) ;
#33224 = EDGE_LOOP ( 'NONE', ( #48061, #22984, #65542, #90045 ) ) ;
#33225 = CARTESIAN_POINT ( 'NONE',  ( -70.28247728326880406, -25.03149372358761227, 7.560917013690431787 ) ) ;
#33226 = CARTESIAN_POINT ( 'NONE',  ( 5.245434476726341444, -20.39595507048906242, -1.500000000000002220 ) ) ;
#33227 = ADVANCED_FACE ( 'NONE', ( #42058 ), #41047, .T. ) ;
#33228 = EDGE_LOOP ( 'NONE', ( #60004, #83105, #43802, #69488 ) ) ;
#33229 = CARTESIAN_POINT ( 'NONE',  ( -85.62287095715004170, -23.48783264082478794, -1.443836473390063713 ) ) ;
#33230 = CARTESIAN_POINT ( 'NONE',  ( 8.160000000000000142, -2.191226316053958875E-18, 2.701633758479787833E-17 ) ) ;
#33231 = CARTESIAN_POINT ( 'NONE',  ( -120.5163168400560352, -25.00182538069147142, 7.747789668545046027 ) ) ;
#33232 = CARTESIAN_POINT ( 'NONE',  ( -86.51786200934954252, -23.73791477778911840, 11.05961554403170766 ) ) ;
#33233 = PLANE ( 'NONE',  #83779 ) ;
#33234 = CARTESIAN_POINT ( 'NONE',  ( -18.45943378446990835, 11.37049804852326140, -1.500000000000002220 ) ) ;
#33235 = DIRECTION ( 'NONE',  ( 0.000000000000000000, -1.000000000000000000, 0.000000000000000000 ) ) ;
#33237 = ORIENTED_EDGE ( 'NONE', *, *, #65059, .F. ) ;
#33236 = CARTESIAN_POINT ( 'NONE',  ( -12.31279356157217109, -18.55646752483835016, 11.49999999999999645 ) ) ;
#33238 = CARTESIAN_POINT ( 'NONE',  ( -51.52657066994672164, -25.31441930330192491, 6.155056426832686611 ) ) ;
#33239 = ADVANCED_FACE ( 'NONE', ( #87210 ), #76524, .F. ) ;
#33240 = DIRECTION ( 'NONE',  ( -0.000000000000000000, -1.000000000000000000, -0.000000000000000000 ) ) ;
#33241 = ORIENTED_EDGE ( 'NONE', *, *, #54991, .T. ) ;
#33243 = VERTEX_POINT ( 'NONE', #43914 ) ;
#33242 = CARTESIAN_POINT ( 'NONE',  ( -6.100820854657341918, -6.376774720514413630, 19.76359802465961124 ) ) ;
#33244 = ORIENTED_EDGE ( 'NONE', *, *, #18535, .F. ) ;
#33245 = AXIS2_PLACEMENT_3D ( 'NONE', #78200, #53887, #54892 ) ;
#33246 = CARTESIAN_POINT ( 'NONE',  ( 30.93898937471034216, -4.884441105398384941, -1.603546260404424606 ) ) ;
#33247 = CC_DESIGN_DATE_AND_TIME_ASSIGNMENT ( #44527, #99776, ( #44192 ) ) ;
#33248 = CARTESIAN_POINT ( 'NONE',  ( 9.931738293602487389, -17.53800358597336384, -1.500000000000002220 ) ) ;
#33249 = CARTESIAN_POINT ( 'NONE',  ( -126.5228709571500332, -24.50321055353804311, 9.387540953477511607 ) ) ;
#33250 = VERTEX_POINT ( 'NONE', #55783 ) ;
#33251 = CARTESIAN_POINT ( 'NONE',  ( -130.5728709571500872, -24.96453677868172605, 8.261112634458179116 ) ) ;
#33252 = CARTESIAN_POINT ( 'NONE',  ( -22.05133119090760019, 4.102169094691678453, -1.500000000000002220 ) ) ;
#33253 = EDGE_LOOP ( 'NONE', ( #13593, #39141, #92755, #60300 ) ) ;
#33254 = ORIENTED_EDGE ( 'NONE', *, *, #98023, .T. ) ;
#33255 = CARTESIAN_POINT ( 'NONE',  ( -34.52287095715006160, -24.64965694238575011, 8.947790433994207149 ) ) ;
#33256 = CARTESIAN_POINT ( 'NONE',  ( -101.5487862718491670, -24.51419770103158413, 9.386484678747175181 ) ) ;
#33257 = CARTESIAN_POINT ( 'NONE',  ( -110.5562042904833930, -25.00182538069145721, 7.747789668545099317 ) ) ;
#33258 = CARTESIAN_POINT ( 'NONE',  ( -48.92287095715006728, -23.47593901973090169, -1.443836447538997758 ) ) ;
#33259 = CARTESIAN_POINT ( 'NONE',  ( -63.91063458982754497, -25.14064729901805606, 2.712351064733618422 ) ) ;
#33260 = CARTESIAN_POINT ( 'NONE',  ( -18.73025074496528219, 5.678645368852136777, -1.500000000000002220 ) ) ;
#33261 = DIRECTION ( 'NONE',  ( 1.000000000000000000, -0.000000000000000000, 0.000000000000000000 ) ) ;
#33262 = ORIENTED_EDGE ( 'NONE', *, *, #26993, .T. ) ;
#33263 = CARTESIAN_POINT ( 'NONE',  ( 16.66814584454133907, -13.58961022886752978, -1.500000000000002220 ) ) ;
#33264 = FACE_OUTER_BOUND ( 'NONE', #85202, .T. ) ;
#33265 = CARTESIAN_POINT ( 'NONE',  ( -38.58953762381672448, -23.47593901973091235, -1.443836447539011525 ) ) ;
#33266 = CARTESIAN_POINT ( 'NONE',  ( -27.96875734969026084, 3.316774720514426456, 26.43402280011862615 ) ) ;
#33267 = CARTESIAN_POINT ( 'NONE',  ( -4.700032041049139409, -6.144890974841530351, -9.000000000000000000 ) ) ;
#33269 = AXIS2_PLACEMENT_3D ( 'NONE', #80233, #35067, #96457 ) ;
#33268 = CARTESIAN_POINT ( 'NONE',  ( 6.461317529299694051, 22.01590093704556850, -1.500000000000002220 ) ) ;
#33270 = PERSON_AND_ORGANIZATION ( #70597, #27821 ) ;
#33271 = DIRECTION ( 'NONE',  ( 0.000000000000000000, 1.000000000000000000, 0.000000000000000000 ) ) ;
#33272 = CARTESIAN_POINT ( 'NONE',  ( -70.60159577184752777, -25.31102706251628831, 5.335685664145170648 ) ) ;
#33273 = CARTESIAN_POINT ( 'NONE',  ( -19.48533387766964964, -5.011242947278518045, 11.49999999999999645 ) ) ;
#33274 = CARTESIAN_POINT ( 'NONE',  ( -68.55620429048340725, -23.47596703998600276, 11.44779298504227505 ) ) ;
#33275 = CARTESIAN_POINT ( 'NONE',  ( -32.52609515912349281, -24.66019654487198665, 8.947790411086131712 ) ) ;
#33276 = DIRECTION ( 'NONE',  ( -8.251522442585435191E-16, 0.9513357669802772199, -0.3081562241202470687 ) ) ;
#33277 = FACE_OUTER_BOUND ( 'NONE', #97143, .T. ) ;
#33278 = CARTESIAN_POINT ( 'NONE',  ( -40.62287095715004170, -24.99132157543083466, 2.256160258750667502 ) ) ;
#33279 = CARTESIAN_POINT ( 'NONE',  ( 19.67252036444665109, 2.607452956813616218, -1.500000000000002220 ) ) ;
#33280 = CARTESIAN_POINT ( 'NONE',  ( 3.675000000000004707, 1.999999999999998224, 19.19609335255483984 ) ) ;
#33281 = CARTESIAN_POINT ( 'NONE',  ( 14.19269941865516671, -13.59168563846684563, -1.500000000000002220 ) ) ;
#33282 = CIRCLE ( 'NONE', #88345, 1.835999999999993859 ) ;
#33283 = CARTESIAN_POINT ( 'NONE',  ( -42.64094106932928696, -24.15543982623907127, -0.2315651400026575435 ) ) ;
#33284 = B_SPLINE_CURVE_WITH_KNOTS ( 'NONE', 3,
 ( #82498, #12981, #52062, #47440 ),
 .UNSPECIFIED., .F., .F.,
 ( 4, 4 ),
 ( 0.5809148170514456533, 0.5899212483235611870 ),
 .UNSPECIFIED. ) ;
#33285 = CARTESIAN_POINT ( 'NONE',  ( -32.52287095715005449, -23.72747288104469732, -1.053458166803228346 ) ) ;
#33286 = EDGE_CURVE ( 'NONE', #5376, #65689, #88718, .T. ) ;
#33287 = CARTESIAN_POINT ( 'NONE',  ( 15.99992875909482137, 3.579156900695799060, -27.91088829768895963 ) ) ;
#33288 = CARTESIAN_POINT ( 'NONE',  ( -39.04303308397305727, -25.28006866179717349, 4.215216948383927686 ) ) ;
#33289 = CARTESIAN_POINT ( 'NONE',  ( 16.39479758508079144, -12.47777281027006424, 11.49999999999999645 ) ) ;
#33290 = CARTESIAN_POINT ( 'NONE',  ( 4.127208352283176396, -6.376774720514424288, 21.39624840817692686 ) ) ;
#33291 = EDGE_CURVE ( 'NONE', #4166, #13524, #50162, .T. ) ;
#33292 = CARTESIAN_POINT ( 'NONE',  ( -33.62287095715005592, -23.47596703998600276, 11.44779298504227505 ) ) ;
#33293 = CARTESIAN_POINT ( 'NONE',  ( -18.09186581907994196, -13.49991075323410250, 11.49999999999999645 ) ) ;
#33294 = ORIENTED_EDGE ( 'NONE', *, *, #61018, .F. ) ;
#33295 = CARTESIAN_POINT ( 'NONE',  ( -69.41396772704672458, -25.25639482192426044, 6.552775495269651529 ) ) ;
#33296 = CARTESIAN_POINT ( 'NONE',  ( -123.6228709571500559, -29.50248528299804818, 1.056150453629045360 ) ) ;
#33297 = CARTESIAN_POINT ( 'NONE',  ( -97.63537331154846299, -23.73766607897670156, -1.055555164236452237 ) ) ;
#33298 = CARTESIAN_POINT ( 'NONE',  ( -64.52287095715006160, -23.48783264082476308, -1.443836473390094355 ) ) ;
#33299 = EDGE_CURVE ( 'NONE', #75862, #48269, #24803, .T. ) ;
#33300 = CARTESIAN_POINT ( 'NONE',  ( -110.6228709571500701, -24.82576562982393042, 8.398263435472971494 ) ) ;
#33301 = CARTESIAN_POINT ( 'NONE',  ( 3.787259615384621192, -6.376774720514426065, 21.48076923076922640 ) ) ;
#33302 = EDGE_LOOP ( 'NONE', ( #16808, #24198, #15731, #68277 ) ) ;
#33303 = CARTESIAN_POINT ( 'NONE',  ( -80.39192082756260049, -25.31596222338272639, 4.967919814078590512 ) ) ;
#33304 = CARTESIAN_POINT ( 'NONE',  ( -7.631545101075025705, 21.52643039700453897, 11.49999999999998934 ) ) ;
#33305 = CARTESIAN_POINT ( 'NONE',  ( -111.2429372202815472, -25.24710330342993458, 3.804655253729887665 ) ) ;
#33306 = CARTESIAN_POINT ( 'NONE',  ( -115.5228709571500190, -24.82576562948886689, 8.398263436605494903 ) ) ;
#33307 = CARTESIAN_POINT ( 'NONE',  ( -82.50963591457735902, -24.15620529776628089, 10.23563542870660825 ) ) ;
#33308 = VECTOR ( 'NONE', #38284, 1000.000000000000000 ) ;
#33309 = CARTESIAN_POINT ( 'NONE',  ( -9.984083066403742990, 20.14924292131567185, 11.49999999999999645 ) ) ;
#33310 = EDGE_LOOP ( 'NONE', ( #20032, #85998, #25083, #96983 ) ) ;
#33311 = DIRECTION ( 'NONE',  ( -3.773278334453079618E-23, 0.9999999999976377785, 2.173523156925979975E-06 ) ) ;
#33312 = CARTESIAN_POINT ( 'NONE',  ( -21.51515180086577317, 4.489188270810763548, -1.500000000000002220 ) ) ;
#33313 = CARTESIAN_POINT ( 'NONE',  ( -41.52287095715006870, -29.50248528299804818, 1.056150453629031594 ) ) ;
#33314 = CARTESIAN_POINT ( 'NONE',  ( -34.60129046058678881, -23.96169478059712077, 10.65365249895718769 ) ) ;
#33315 = CARTESIAN_POINT ( 'NONE',  ( -68.93918693012690824, -25.24795196732124936, 6.184868460502651821 ) ) ;
#33316 = VERTEX_POINT ( 'NONE', #32931 ) ;
#33317 = CARTESIAN_POINT ( 'NONE',  ( -92.58953762381672448, -24.64898659630368627, 1.056161002820388717 ) ) ;
#33318 = CARTESIAN_POINT ( 'NONE',  ( 9.749999999999985789, 18.74999999999999645, 2.100000000000000089 ) ) ;
#33319 = ORIENTED_EDGE ( 'NONE', *, *, #46272, .F. ) ;
#33320 = CARTESIAN_POINT ( 'NONE',  ( -19.72667040167412722, -5.651925516699977337, -1.500000000000002220 ) ) ;
#33321 = ORIENTED_EDGE ( 'NONE', *, *, #60826, .T. ) ;
#33322 = ORIENTED_EDGE ( 'NONE', *, *, #82647, .F. ) ;
#33323 = VERTEX_POINT ( 'NONE', #64911 ) ;
#33324 = VERTEX_POINT ( 'NONE', #74844 ) ;
#33325 = CARTESIAN_POINT ( 'NONE',  ( -80.48900664166535535, -25.13313949306887807, 7.101635536975466678 ) ) ;
#33326 = CARTESIAN_POINT ( 'NONE',  ( 3.535601659403828201, -22.84449096179584160, 11.49999999999998934 ) ) ;
#33327 = DIRECTION ( 'NONE',  ( -0.000000000000000000, 1.000000000000000000, -0.000000000000000000 ) ) ;
#33328 = CARTESIAN_POINT ( 'NONE',  ( -18.82647582233506611, 7.659846263794035437, -1.500000000000002220 ) ) ;
#33329 = ORIENTED_EDGE ( 'NONE', *, *, #9701, .T. ) ;
#33330 = CARTESIAN_POINT ( 'NONE',  ( 29.75286985256398253, 5.302859984505953861, 26.69689370802097272 ) ) ;
#33331 = CARTESIAN_POINT ( 'NONE',  ( -29.58011630254760860, -24.43483877924948544, 9.386484716961753350 ) ) ;
#33332 = ADVANCED_FACE ( 'NONE', ( #48163 ), #19119, .T. ) ;
#33333 = FACE_OUTER_BOUND ( 'NONE', #99625, .T. ) ;
#33334 = CARTESIAN_POINT ( 'NONE',  ( -63.52287095715010423, -24.33927499327854349, 9.819080762295818943 ) ) ;
#33336 = ORIENTED_EDGE ( 'NONE', *, *, #26865, .F. ) ;
#33335 = CARTESIAN_POINT ( 'NONE',  ( -21.45671390985790694, -1.711987587955616119, 11.49999999999999645 ) ) ;
#33337 = CARTESIAN_POINT ( 'NONE',  ( -28.10168127693285101, -25.21531671887374060, 2.337526732200711166 ) ) ;
#33338 = DIRECTION ( 'NONE',  ( 0.000000000000000000, -2.173523156925980399E-06, 0.9999999999976378895 ) ) ;
#33339 = VERTEX_POINT ( 'NONE', #67262 ) ;
#33340 = CARTESIAN_POINT ( 'NONE',  ( -20.46667790307254009, -3.548193229090686796, 11.49999999999998934 ) ) ;
#33342 = EDGE_CURVE ( 'NONE', #98743, #49833, #95315, .T. ) ;
#33341 = ORIENTED_EDGE ( 'NONE', *, *, #64617, .T. ) ;
#33344 = ORIENTED_EDGE ( 'NONE', *, *, #97273, .F. ) ;
#33343 = CARTESIAN_POINT ( 'NONE',  ( -125.5202182622694949, -24.52300882791529801, 0.6510814631126508045 ) ) ;
#33345 = VECTOR ( 'NONE', #39305, 1000.000000000000000 ) ;
#33346 = CARTESIAN_POINT ( 'NONE',  ( -77.52287095715006160, -24.64898659630367916, 1.056161002820826145 ) ) ;
#33347 = CARTESIAN_POINT ( 'NONE',  ( -97.52287095715004739, -23.73934037231758154, 11.05740245334328797 ) ) ;
#33348 = VERTEX_POINT ( 'NONE', #98182 ) ;
#33349 = VERTEX_POINT ( 'NONE', #52523 ) ;
#33350 = CIRCLE ( 'NONE', #41476, 0.8500000000000017542 ) ;
#33351 = DIRECTION ( 'NONE',  ( -0.8899332505568755547, 9.913238957044378156E-07, -0.4560907909093217527 ) ) ;
#33352 = CARTESIAN_POINT ( 'NONE',  ( -68.62287095715002749, -23.73934037231756378, 11.05740245334329153 ) ) ;
#33353 = VECTOR ( 'NONE', #92539, 1000.000000000000000 ) ;
#33354 = CARTESIAN_POINT ( 'NONE',  ( -78.52287095715004739, -24.50216790748204332, 0.6166512839542561686 ) ) ;
#33356 = EDGE_LOOP ( 'NONE', ( #7956, #43923, #15015, #77542 ) ) ;
#33355 = CARTESIAN_POINT ( 'NONE',  ( 7.855769811932122870, -20.56199346058834720, 11.49999999999999645 ) ) ;
#33357 = CIRCLE ( 'NONE', #4179, 2.499999999999963141 ) ;
#33358 = CARTESIAN_POINT ( 'NONE',  ( -103.5492918164049598, -24.51314013834316086, 0.6176544820404170633 ) ) ;
#33359 = CARTESIAN_POINT ( 'NONE',  ( -16.99934442671578694, -14.85117937636706031, 11.49999999999998934 ) ) ;
#33360 = VECTOR ( 'NONE', #57528, 1000.000000000000000 ) ;
#33362 = ORIENTED_EDGE ( 'NONE', *, *, #45186, .F. ) ;
#33361 = CARTESIAN_POINT ( 'NONE',  ( 30.77564450787170003, -1.477225279485574028, -9.689394075852828081 ) ) ;
#33363 = VERTEX_POINT ( 'NONE', #22050 ) ;
#33364 = B_SPLINE_CURVE_WITH_KNOTS ( 'NONE', 3,
 ( #82354, #49938, #51419, #10857 ),
 .UNSPECIFIED., .F., .F.,
 ( 4, 4 ),
 ( 0.2406718578826401722, 0.2496782891547557337 ),
 .UNSPECIFIED. ) ;
#33365 = CARTESIAN_POINT ( 'NONE',  ( -79.52287095715006160, -29.50248528299804818, 1.056150453629038477 ) ) ;
#33366 = EDGE_CURVE ( 'NONE', #17742, #91875, #42524, .T. ) ;
#33367 = CARTESIAN_POINT ( 'NONE',  ( -57.49288415400445018, -24.51419770103157703, 9.386484678747175181 ) ) ;
#33368 = VERTEX_POINT ( 'NONE', #36303 ) ;
#33369 = CARTESIAN_POINT ( 'NONE',  ( -6.524719417830534773, 20.15472526627327454, 11.49999999999998934 ) ) ;
#33370 = CARTESIAN_POINT ( 'NONE',  ( -82.62287095715005592, -23.48783264082478084, -1.443836473390065933 ) ) ;
#33371 = CARTESIAN_POINT ( 'NONE',  ( -92.62287095715005592, -24.65952944569304606, 1.056160979905700348 ) ) ;
#33372 = DIRECTION ( 'NONE',  ( -3.773278334453079618E-23, 0.9999999999976377785, 2.173523156925979975E-06 ) ) ;
#33373 = CARTESIAN_POINT ( 'NONE',  ( -26.09636659181000695, -29.50249372523856195, 4.940277699495910113 ) ) ;
#33374 = CARTESIAN_POINT ( 'NONE',  ( -11.95080204275630464, 18.75100984808165094, -1.500000000000002220 ) ) ;
#33375 = CARTESIAN_POINT ( 'NONE',  ( -114.5530387260713638, -24.34968618360934300, 0.1864209137778971848 ) ) ;
#33376 = ORIENTED_EDGE ( 'NONE', *, *, #76585, .T. ) ;
#33377 = CARTESIAN_POINT ( 'NONE',  ( 11.54156857142115911, -3.316774720514427344, -28.05134709678029381 ) ) ;
#33378 = CARTESIAN_POINT ( 'NONE',  ( -30.57287095715006231, -23.47594215783195537, -5.102550391006585557E-05 ) ) ;
#33379 = CARTESIAN_POINT ( 'NONE',  ( -19.08929872761019908, -3.557156390981079053, 11.49999999999999645 ) ) ;
#33380 = ADVANCED_FACE ( 'NONE', ( #92563 ), #84954, .F. ) ;
#33381 = B_SPLINE_CURVE_WITH_KNOTS ( 'NONE', 3,
 ( #74515, #50689, #35468, #36452, #88252, #20219 ),
 .UNSPECIFIED., .F., .F.,
 ( 4, 2, 4 ),
 ( 0.000000000000000000, 0.001380901958385379220, 0.002761803916770758441 ),
 .UNSPECIFIED. ) ;
#33382 = CARTESIAN_POINT ( 'NONE',  ( 29.64064043116815128, -6.475225279485573360, 28.71191112024341408 ) ) ;
#33383 = DIRECTION ( 'NONE',  ( -0.000000000000000000, -1.000000000000000000, -0.000000000000000000 ) ) ;
#33384 = CARTESIAN_POINT ( 'NONE',  ( 15.68791110202092476, 11.56419973807686219, 11.49999999999998934 ) ) ;
#33385 = CARTESIAN_POINT ( 'NONE',  ( 16.75108703964928480, -13.32659110743468212, -1.500000000000002220 ) ) ;
#33386 = CARTESIAN_POINT ( 'NONE',  ( 9.782918536709168222, -0.6683258531633530231, 18.35000000000000142 ) ) ;
#33387 = CARTESIAN_POINT ( 'NONE',  ( -60.62371847853048479, -25.00182538069856619, 7.747789668514392325 ) ) ;
#33388 = DIRECTION ( 'NONE',  ( -2.006501617224642956E-17, 0.5416355246053408123, -0.8406134417706495610 ) ) ;
#33389 = CARTESIAN_POINT ( 'NONE',  ( -59.62287095715004881, -29.50250786944525672, 11.44777988621623876 ) ) ;
#33390 = CARTESIAN_POINT ( 'NONE',  ( 18.51665531608540860, 13.21585733361752801, -1.500000000000002220 ) ) ;
#33391 = CARTESIAN_POINT ( 'NONE',  ( 0.000000000000000000, -1.473225279485573802, 0.000000000000000000 ) ) ;
#33392 = CARTESIAN_POINT ( 'NONE',  ( -102.5109985006918976, -24.51314013834317151, 0.6176544820404245018 ) ) ;
#33393 = CARTESIAN_POINT ( 'NONE',  ( 15.32643653063177958, 2.682774720514426559, -27.14485409495429380 ) ) ;
#33394 = CARTESIAN_POINT ( 'NONE',  ( 9.006517291608927778, -17.75031788249398446, 11.49999999999999645 ) ) ;
#33395 = CARTESIAN_POINT ( 'NONE',  ( 5.873458226074941280, -6.376774720514413630, 19.84669099281175164 ) ) ;
#33396 = ADVANCED_FACE ( 'NONE', ( #5348 ), #82955, .T. ) ;
#33397 = DIRECTION ( 'NONE',  ( 1.000000000000000000, -0.000000000000000000, 0.000000000000000000 ) ) ;
#33398 = DIRECTION ( 'NONE',  ( 1.000000000000000000, 0.000000000000000000, -0.000000000000000000 ) ) ;
#33399 = ADVANCED_FACE ( 'NONE', ( #22540 ), #44421, .F. ) ;
#33400 = VERTEX_POINT ( 'NONE', #45912 ) ;
#33401 = CARTESIAN_POINT ( 'NONE',  ( -50.06403713569625324, -25.12896391188073508, 7.067345851436766857 ) ) ;
#33402 = CARTESIAN_POINT ( 'NONE',  ( -32.40341606139129738, -25.31600595412499644, 6.101236642668423471 ) ) ;
#33403 = DIRECTION ( 'NONE',  ( 0.000000000000000000, 1.000000000000000000, -0.000000000000000000 ) ) ;
#33404 = CARTESIAN_POINT ( 'NONE',  ( -15.38093110518717666, 15.28219592669002402, 11.49999999999998934 ) ) ;
#33405 = FACE_OUTER_BOUND ( 'NONE', #27267, .T. ) ;
#33406 = CARTESIAN_POINT ( 'NONE',  ( -17.86923650574433609, -7.721772263035739492, -1.500000000000002220 ) ) ;
#33407 = AXIS2_PLACEMENT_3D ( 'NONE', #81590, #82082, #43032 ) ;
#33408 = CARTESIAN_POINT ( 'NONE',  ( -93.52287095715009002, -23.48783264082477018, -1.443836473390088360 ) ) ;
#33409 = ORIENTED_EDGE ( 'NONE', *, *, #33990, .T. ) ;
#33410 = CARTESIAN_POINT ( 'NONE',  ( -20.15914900662387055, -2.930279687489938389, 11.49999999999999645 ) ) ;
#33411 = PLANE ( 'NONE',  #84529 ) ;
#33412 = EDGE_CURVE ( 'NONE', #75504, #54444, #80752, .T. ) ;
#33413 = AXIS2_PLACEMENT_3D ( 'NONE', #49678, #24816, #86224 ) ;
#33414 = CARTESIAN_POINT ( 'NONE',  ( -1.140932434931746582E-13, -5.876774720514426953, 21.78128695274321203 ) ) ;
#33415 = EDGE_CURVE ( 'NONE', #40153, #71923, #91074, .T. ) ;
#33416 = ORIENTED_EDGE ( 'NONE', *, *, #28030, .F. ) ;
#33417 = CARTESIAN_POINT ( 'NONE',  ( -79.45125215927727425, -25.10767898202385950, 7.188516721831696543 ) ) ;
#33418 = DIRECTION ( 'NONE',  ( 1.000000000000000000, -0.000000000000000000, -0.000000000000000000 ) ) ;
#33419 = CARTESIAN_POINT ( 'NONE',  ( 7.190659024148910561, -6.376774720514413630, 19.91543959911579620 ) ) ;
#33420 = CIRCLE ( 'NONE', #15592, 10.80000000000000782 ) ;
#33421 = CARTESIAN_POINT ( 'NONE',  ( -70.52287095715007581, -29.50249982740957577, 7.747779886224967605 ) ) ;
#33422 = AXIS2_PLACEMENT_3D ( 'NONE', #45264, #91924, #60501 ) ;
#33423 = DIRECTION ( 'NONE',  ( 0.000000000000000000, 0.000000000000000000, 1.000000000000000000 ) ) ;
#33424 = ADVANCED_FACE ( 'NONE', ( #92070 ), #73424, .T. ) ;
#33425 = AXIS2_PLACEMENT_3D ( 'NONE', #5565, #83685, #14165 ) ;
#33426 = PLANE ( 'NONE',  #4672 ) ;
#33427 = ORIENTED_EDGE ( 'NONE', *, *, #53351, .T. ) ;
#33428 = CARTESIAN_POINT ( 'NONE',  ( -29.49875734969026198, 5.965225279485572685, 0.1180228001186258285 ) ) ;
#33429 = AXIS2_PLACEMENT_3D ( 'NONE', #20568, #51540, #12952 ) ;
#33430 = EDGE_CURVE ( 'NONE', #49698, #38599, #16947, .T. ) ;
#33431 = CARTESIAN_POINT ( 'NONE',  ( -10.62949710387652758, 20.32685691788189075, 11.49999999999999645 ) ) ;
#33432 = CARTESIAN_POINT ( 'NONE',  ( 15.23092229589061830, -16.91372389758942418, -1.500000000000002220 ) ) ;
#33433 = CARTESIAN_POINT ( 'NONE',  ( 4.189750619059152470, -6.376774720514427841, 21.76591699724029283 ) ) ;
#33434 = LINE ( 'NONE', #25824, #78724 ) ;
#33435 = CARTESIAN_POINT ( 'NONE',  ( -90.55814957459756442, -23.85016227208580730, -0.8807180028928305315 ) ) ;
#33436 = CARTESIAN_POINT ( 'NONE',  ( -82.55620429048340725, -23.48783264082478084, -1.443836473390066377 ) ) ;
#33437 = CARTESIAN_POINT ( 'NONE',  ( -17.40403014803320758, -13.24600170205644289, -1.500000000000002220 ) ) ;
#33438 = DIRECTION ( 'NONE',  ( -1.000000000000000000, -3.773278334444167608E-23, -8.201307833595939069E-29 ) ) ;
#33439 = DIRECTION ( 'NONE',  ( -0.7071067811865452413, 8.659560562354961208E-17, -0.7071067811865497932 ) ) ;
#33440 = CARTESIAN_POINT ( 'NONE',  ( -122.5190359270850990, -24.51314013834316086, 0.6176544820404212821 ) ) ;
#33441 = CARTESIAN_POINT ( 'NONE',  ( -81.55620429048342146, -23.47593901973091235, -1.443836447539004642 ) ) ;
#33442 = VERTEX_POINT ( 'NONE', #63141 ) ;
#33443 = CARTESIAN_POINT ( 'NONE',  ( 8.094744887094867281, -18.73235182305680624, 11.49999999999998934 ) ) ;
#33444 = ORIENTED_EDGE ( 'NONE', *, *, #11053, .F. ) ;
#33445 = VERTEX_POINT ( 'NONE', #17444 ) ;
#33446 = CARTESIAN_POINT ( 'NONE',  ( -4.971178678486217528, -22.47594730032828281, -1.500000000000002220 ) ) ;
#33447 = DIRECTION ( 'NONE',  ( -0.000000000000000000, 1.000000000000000000, -0.000000000000000000 ) ) ;
#33448 = ORIENTED_EDGE ( 'NONE', *, *, #61494, .T. ) ;
#33449 = AXIS2_PLACEMENT_3D ( 'NONE', #70303, #44975, #783 ) ;
#33450 = LINE ( 'NONE', #64439, #41262 ) ;
#33451 = CARTESIAN_POINT ( 'NONE',  ( -42.52287095715005449, -23.47593901973090169, -1.443836447538997092 ) ) ;
#33452 = LINE ( 'NONE', #48193, #90062 ) ;
#33453 = CARTESIAN_POINT ( 'NONE',  ( -116.6623051836383667, -25.28353586862649038, 5.756525109479947666 ) ) ;
#33455 = ORIENTED_EDGE ( 'NONE', *, *, #68209, .T. ) ;
#33454 = CARTESIAN_POINT ( 'NONE',  ( 14.87313431965483801, 15.23822737908125902, 11.49999999999999645 ) ) ;
#33456 = EDGE_LOOP ( 'NONE', ( #43794, #15882, #59090, #54299 ) ) ;
#33457 = CARTESIAN_POINT ( 'NONE',  ( -15.91109736606077441, 15.52988587838853540, 11.49999999999998934 ) ) ;
#33458 = CARTESIAN_POINT ( 'NONE',  ( 20.52162115075873672, 2.272738508513782119, -1.500000000000002220 ) ) ;
#33459 = B_SPLINE_CURVE_WITH_KNOTS ( 'NONE', 3,
 ( #79145, #63962, #40094, #48216 ),
 .UNSPECIFIED., .F., .F.,
 ( 4, 4 ),
 ( 0.000000000000000000, 0.0002633127703855885223 ),
 .UNSPECIFIED. ) ;
#33460 = ORIENTED_EDGE ( 'NONE', *, *, #680, .T. ) ;
#33461 = EDGE_CURVE ( 'NONE', #11978, #82726, #91516, .T. ) ;
#33462 = CARTESIAN_POINT ( 'NONE',  ( -6.020540257910568904, -6.376774720514411854, 19.49847411603315095 ) ) ;
#33463 = CARTESIAN_POINT ( 'NONE',  ( -69.85793399335128129, -25.20650855361216713, 6.812664954086296909 ) ) ;
#33464 = VERTEX_POINT ( 'NONE', #87462 ) ;
#33465 = FACE_OUTER_BOUND ( 'NONE', #8749, .T. ) ;
#33466 = ORIENTED_EDGE ( 'NONE', *, *, #1568, .F. ) ;
#33467 = CARTESIAN_POINT ( 'NONE',  ( -58.50878158211892810, -23.96169478059713143, 10.65365249895718058 ) ) ;
#33468 = DIRECTION ( 'NONE',  ( 0.000000000000000000, 2.173523156925980399E-06, -0.9999999999976378895 ) ) ;
#33469 = CARTESIAN_POINT ( 'NONE',  ( -13.97254113366623152, 15.51630364309664856, -1.500000000000002220 ) ) ;
#33470 = CARTESIAN_POINT ( 'NONE',  ( -15.04333773895388937, -15.80532200100455498, 11.49999999999999645 ) ) ;
#33471 = DIRECTION ( 'NONE',  ( -0.000000000000000000, -0.000000000000000000, -1.000000000000000000 ) ) ;
#33472 = LINE ( 'NONE', #64463, #88837 ) ;
#33473 = CARTESIAN_POINT ( 'NONE',  ( 22.09666729679958053, 4.251135690456572469, 11.49999999999998934 ) ) ;
#33474 = AXIS2_PLACEMENT_3D ( 'NONE', #78186, #75816, #90552 ) ;
#33475 = CARTESIAN_POINT ( 'NONE',  ( -5.518977837361389582, -20.17201009624758257, -1.500000000000002220 ) ) ;
#33477 = FACE_OUTER_BOUND ( 'NONE', #82413, .T. ) ;
#33476 = B_SPLINE_CURVE_WITH_KNOTS ( 'NONE', 3,
 ( #84818, #15303, #8209, #16311 ),
 .UNSPECIFIED., .F., .F.,
 ( 4, 4 ),
 ( 0.000000000000000000, 9.999999999998897304E-05 ),
 .UNSPECIFIED. ) ;
#33478 = B_SPLINE_CURVE_WITH_KNOTS ( 'NONE', 3,
 ( #28394, #14670, #69961, #29898, #68963, #99887 ),
 .UNSPECIFIED., .F., .F.,
 ( 4, 2, 4 ),
 ( 1.570887131794333942E-05, 0.001396322306279758904, 0.002776935741241574537 ),
 .UNSPECIFIED. ) ;
#33479 = CARTESIAN_POINT ( 'NONE',  ( -52.55620429048339304, -24.66019654487199020, 8.947790411086135265 ) ) ;
#33480 = CARTESIAN_POINT ( 'NONE',  ( -68.58953762381672448, -23.47593901973091235, -1.443836447539006196 ) ) ;
#33481 = VERTEX_POINT ( 'NONE', #71747 ) ;
#33482 = ORIENTED_EDGE ( 'NONE', *, *, #42800, .T. ) ;
#33483 = ORIENTED_EDGE ( 'NONE', *, *, #31784, .F. ) ;
#33484 = CARTESIAN_POINT ( 'NONE',  ( -52.50176957019452573, -24.15543982623907482, -0.2315651400026529916 ) ) ;
#33485 = ORIENTED_EDGE ( 'NONE', *, *, #16879, .T. ) ;
#33486 = VECTOR ( 'NONE', #74095, 1000.000000000000000 ) ;
#33487 = ADVANCED_FACE ( 'NONE', ( #24051 ), #55527, .T. ) ;
#33488 = CARTESIAN_POINT ( 'NONE',  ( -1.242826169824672977, 21.35102975155811222, -1.500000000000002220 ) ) ;
#33489 = CARTESIAN_POINT ( 'NONE',  ( 21.44611857939883137, 6.294191480875499067, 11.49999999999999645 ) ) ;
#33490 = ORIENTED_EDGE ( 'NONE', *, *, #71999, .T. ) ;
#33491 = CARTESIAN_POINT ( 'NONE',  ( -59.52287095715007581, -23.96127896941631974, -0.6493128931038036900 ) ) ;
#33492 = VECTOR ( 'NONE', #63205, 1000.000000000000000 ) ;
#33493 = CARTESIAN_POINT ( 'NONE',  ( 9.758084087097168791, -18.66043984184860349, -1.500000000000002220 ) ) ;
#33494 = CARTESIAN_POINT ( 'NONE',  ( -30.64649332944061655, -23.48782090502276176, 11.44779287168131710 ) ) ;
#33495 = CARTESIAN_POINT ( 'NONE',  ( 1.402406813841059030, 19.88454085074057076, -1.500000000000002220 ) ) ;
#33496 = DIRECTION ( 'NONE',  ( -0.000000000000000000, -1.000000000000000000, -0.000000000000000000 ) ) ;
#33497 = TOROIDAL_SURFACE ( 'NONE', #78893, 25.90800000000000125, 3.060000000000000053 ) ;
#33498 = CARTESIAN_POINT ( 'NONE',  ( -113.5228709571500758, -23.48783264082477373, -1.443836473390082586 ) ) ;
#33499 = CARTESIAN_POINT ( 'NONE',  ( -6.199593828526920092, 21.14725108817225419, -1.500000000000002220 ) ) ;
#33500 = ORIENTED_EDGE ( 'NONE', *, *, #3628, .F. ) ;
#33501 = CARTESIAN_POINT ( 'NONE',  ( -65.48791648632810336, -24.83644354573578994, 8.397322867130098345 ) ) ;
#33502 = EDGE_CURVE ( 'NONE', #36274, #50583, #224, .T. ) ;
#33503 = CYLINDRICAL_SURFACE ( 'NONE', #10883, 0.09999999999999939493 ) ;
#33504 = CARTESIAN_POINT ( 'NONE',  ( -40.63161819696095733, -25.27956070701981162, 5.540357918835671747 ) ) ;
#33505 = ADVANCED_FACE ( 'NONE', ( #15937 ), #78827, .F. ) ;
#33506 = VECTOR ( 'NONE', #85709, 1000.000000000000114 ) ;
#33507 = EDGE_CURVE ( 'NONE', #87407, #34175, #83061, .T. ) ;
#33508 = CARTESIAN_POINT ( 'NONE',  ( -62.50437674283933376, -24.15620529776627734, 10.23563542870660825 ) ) ;
#33509 = CARTESIAN_POINT ( 'NONE',  ( 282.9764569301858046, 6.376774720514426953, 20.79159422840526616 ) ) ;
#33510 = EDGE_CURVE ( 'NONE', #78003, #76683, #98693, .T. ) ;
#33511 = CARTESIAN_POINT ( 'NONE',  ( -61.62287095715004881, -24.65952944569304606, 1.056160979905695907 ) ) ;
#33512 = CARTESIAN_POINT ( 'NONE',  ( -1.825377252022436281, -21.23478267787193730, 11.49999999999998934 ) ) ;
#33513 = CARTESIAN_POINT ( 'NONE',  ( -121.5895376238167103, -24.64965694238408034, 8.947790433994647685 ) ) ;
#33514 = CARTESIAN_POINT ( 'NONE',  ( -117.5228709571500758, -23.48786465467241769, 11.44779295918253759 ) ) ;
#33515 = CARTESIAN_POINT ( 'NONE',  ( 29.73860345376319003, -5.356774720514425603, -4.021180035027960287 ) ) ;
#33516 = DIRECTION ( 'NONE',  ( 0.000000000000000000, -1.000000000000000000, 0.000000000000000000 ) ) ;
#33517 = CARTESIAN_POINT ( 'NONE',  ( -12.77507031947300042, 18.62636059118606724, -1.500000000000002220 ) ) ;
#33518 = CARTESIAN_POINT ( 'NONE',  ( 19.72776355195876263, 0.3587747205144265483, 28.39950002376595606 ) ) ;
#33519 = ORIENTED_EDGE ( 'NONE', *, *, #6598, .F. ) ;
#33520 = CARTESIAN_POINT ( 'NONE',  ( 4.573489327750471567, -5.876774720514419847, 20.79634280254998657 ) ) ;
#33521 = CARTESIAN_POINT ( 'NONE',  ( -31.50372651583977657, -23.96169478059712432, 10.65365249895719124 ) ) ;
#33522 = CARTESIAN_POINT ( 'NONE',  ( -2.355416116969162754, -19.56741566493107598, 11.49999999999999645 ) ) ;
#33523 = CARTESIAN_POINT ( 'NONE',  ( -41.22287095715007155, -23.47593901973090169, -1.443836447538997980 ) ) ;
#33524 = B_SPLINE_CURVE_WITH_KNOTS ( 'NONE', 3,
 ( #10698, #34037, #41660, #65013 ),
 .UNSPECIFIED., .F., .F.,
 ( 4, 4 ),
 ( 0.6002145229766536749, 0.6092209542487688756 ),
 .UNSPECIFIED. ) ;
#33525 = DIRECTION ( 'NONE',  ( -3.773278334453079618E-23, 0.9999999999976377785, 2.173523156925979975E-06 ) ) ;
#33526 = EDGE_CURVE ( 'NONE', #51543, #36438, #18913, .T. ) ;
#33527 = ORIENTED_EDGE ( 'NONE', *, *, #4819, .F. ) ;
#33528 = DIRECTION ( 'NONE',  ( 0.000000000000000000, 0.000000000000000000, 1.000000000000000000 ) ) ;
#33529 = CARTESIAN_POINT ( 'NONE',  ( 32.16024265030974050, -0.3587747205144265483, 16.27760796525321751 ) ) ;
#33530 = CARTESIAN_POINT ( 'NONE',  ( -124.6256213753410691, -23.73791477778912551, 11.05961554403169878 ) ) ;
#33531 = AXIS2_PLACEMENT_3D ( 'NONE', #39954, #17111, #9001 ) ;
#33532 = CARTESIAN_POINT ( 'NONE',  ( 29.73860345376319358, 5.356774720496559894, 1.647607965253216511 ) ) ;
#33533 = DIRECTION ( 'NONE',  ( 0.000000000000000000, 1.020425574104004246E-16, -1.000000000000000000 ) ) ;
#33534 = LINE ( 'NONE', #2600, #64288 ) ;
#33535 = CARTESIAN_POINT ( 'NONE',  ( -19.30086548479123465, -4.275078920326023990, 11.49999999999998934 ) ) ;
#33536 = EDGE_LOOP ( 'NONE', ( #40142, #3776, #78587, #73491, #19090, #8014, #3946, #56191, #53906, #36524, #93062 ) ) ;
#33537 = AXIS2_PLACEMENT_3D ( 'NONE', #98129, #58108, #51978 ) ;
#33538 = CARTESIAN_POINT ( 'NONE',  ( -18.67835518149133378, -7.740158416121700746, 11.49999999999999645 ) ) ;
#33539 = CARTESIAN_POINT ( 'NONE',  ( 11.51813299235546673, 6.376774720514426953, -25.01561358505534471 ) ) ;
#33540 = EDGE_CURVE ( 'NONE', #55957, #8604, #89009, .T. ) ;
#33541 = EDGE_CURVE ( 'NONE', #56728, #23355, #37640, .T. ) ;
#33542 = ORIENTED_EDGE ( 'NONE', *, *, #64893, .F. ) ;
#33543 = CARTESIAN_POINT ( 'NONE',  ( 13.91401389203221406, 0.3587747205144265483, 158.0376437107427137 ) ) ;
#33544 = CARTESIAN_POINT ( 'NONE',  ( -81.26450725226473537, -25.30500210224441560, 5.136533544873633339 ) ) ;
#33545 = CARTESIAN_POINT ( 'NONE',  ( -77.52287095715006160, -24.64965694238575011, 8.947790433994198267 ) ) ;
#33546 = CARTESIAN_POINT ( 'NONE',  ( -112.6228709571500559, -24.64965695001469115, 8.947790433994176951 ) ) ;
#33547 = CARTESIAN_POINT ( 'NONE',  ( -39.62287095715005592, -24.65952944569304606, 1.056160979905692354 ) ) ;
#33548 = CARTESIAN_POINT ( 'NONE',  ( -0.02075734969026423599, 0.3587747205144213303, -0.08597719988137648983 ) ) ;
#33549 = CARTESIAN_POINT ( 'NONE',  ( -18.22994410263883225, 8.285605901428201747, 11.49999999999998934 ) ) ;
#33550 = EDGE_CURVE ( 'NONE', #63463, #7016, #76949, .T. ) ;
#33551 = CARTESIAN_POINT ( 'NONE',  ( -99.12594121859551421, -25.10935281042543821, 3.952133049703926648 ) ) ;
#33552 = ORIENTED_EDGE ( 'NONE', *, *, #73971, .T. ) ;
#33553 = VECTOR ( 'NONE', #19647, 1000.000000000000000 ) ;
#33554 = EDGE_CURVE ( 'NONE', #10013, #25854, #11341, .T. ) ;
#33555 = EDGE_CURVE ( 'NONE', #51332, #83129, #96567, .T. ) ;
#33556 = DIRECTION ( 'NONE',  ( 0.000000000000000000, -0.000000000000000000, -1.000000000000000000 ) ) ;
#33557 = CARTESIAN_POINT ( 'NONE',  ( 8.071512145086503054, -1.028487854913507693, -5.500000000000000000 ) ) ;
#33558 = CARTESIAN_POINT ( 'NONE',  ( -100.6228709571500559, -24.99156045073393173, 7.747789690856161648 ) ) ;
#33559 = B_SPLINE_CURVE_WITH_KNOTS ( 'NONE', 3,
 ( #81562, #4443, #82054, #12037, #28264, #34885 ),
 .UNSPECIFIED., .F., .F.,
 ( 4, 2, 4 ),
 ( 0.000000000000000000, 0.001380764517853248600, 0.002761529035706497201 ),
 .UNSPECIFIED. ) ;
#33560 = CARTESIAN_POINT ( 'NONE',  ( -84.52287095715006160, -29.50248528299804818, 1.056150453629038477 ) ) ;
#33561 = CARTESIAN_POINT ( 'NONE',  ( -101.5413594152072960, -25.20011968295217386, 3.398381376179529401 ) ) ;
#33562 = CIRCLE ( 'NONE', #4383, 2.249999999999998668 ) ;
#33563 = CARTESIAN_POINT ( 'NONE',  ( 14.74815398954886270, 3.719725396297121289, -28.39563063676393639 ) ) ;
#33564 = EDGE_CURVE ( 'NONE', #32852, #76880, #38879, .T. ) ;
#33566 = VECTOR ( 'NONE', #40356, 1000.000000000000114 ) ;
#33565 = CARTESIAN_POINT ( 'NONE',  ( -49.51564274782410280, -25.25375110409948576, 3.879908378599426833 ) ) ;
#33567 = ORIENTED_EDGE ( 'NONE', *, *, #79220, .T. ) ;
#33568 = AXIS2_PLACEMENT_3D ( 'NONE', #38491, #23751, #52720 ) ;
#33569 = CARTESIAN_POINT ( 'NONE',  ( 5.353267490507026771, -19.58905154090721368, 11.49999999999998934 ) ) ;
#33570 = EDGE_LOOP ( 'NONE', ( #69007, #6534, #88284, #93722 ) ) ;
#33571 = CARTESIAN_POINT ( 'NONE',  ( 31.60706529141451426, 4.540774720514427543, 26.12024523944107202 ) ) ;
#33572 = CARTESIAN_POINT ( 'NONE',  ( -127.5214690509877187, -24.15620529776629155, 10.23563542870658694 ) ) ;
#33573 = ORIENTED_EDGE ( 'NONE', *, *, #69772, .T. ) ;
#33574 = DIRECTION ( 'NONE',  ( -0.000000000000000000, 2.173523156925979552E-06, -0.9999999999976378895 ) ) ;
#33575 = CARTESIAN_POINT ( 'NONE',  ( -50.28030459868799795, -25.26264177999245319, 7.099251632680519286 ) ) ;
#33576 = CARTESIAN_POINT ( 'NONE',  ( -30.47287095715006089, -24.48470683598323916, 9.426283873570685756 ) ) ;
#33577 = CARTESIAN_POINT ( 'NONE',  ( 14.48694714638828884, 15.39972936300609341, 11.49999999999999645 ) ) ;
#33578 = CARTESIAN_POINT ( 'NONE',  ( 20.51613352552997327, 8.347415244503286758, -1.500000000000002220 ) ) ;
#33579 = CARTESIAN_POINT ( 'NONE',  ( 18.12345787009687115, -9.690629616749632191, -1.500000000000002220 ) ) ;
#33580 = ORIENTED_EDGE ( 'NONE', *, *, #92724, .F. ) ;
#33581 = CARTESIAN_POINT ( 'NONE',  ( -94.52287095715003318, -24.66019654487199730, 8.947790411086124607 ) ) ;
#33582 = EDGE_LOOP ( 'NONE', ( #12254, #92608, #83579, #74133 ) ) ;
#33583 = PLANE ( 'NONE',  #15528 ) ;
#33584 = CARTESIAN_POINT ( 'NONE',  ( -80.62287095715005592, -23.47593901973091235, -1.443836447539004642 ) ) ;
#33585 = VERTEX_POINT ( 'NONE', #89958 ) ;
#33586 = ORIENTED_EDGE ( 'NONE', *, *, #56612, .F. ) ;
#33587 = VERTEX_POINT ( 'NONE', #27069 ) ;
#33588 = DIRECTION ( 'NONE',  ( 0.000000000000000000, -2.173523156925979552E-06, 0.9999999999976378895 ) ) ;
#33589 = CARTESIAN_POINT ( 'NONE',  ( -127.6228709571500275, -23.73934037231758154, 11.05740245334327732 ) ) ;
#33590 = CARTESIAN_POINT ( 'NONE',  ( 6.156881756163101294, -5.876774720514413630, 19.74809127057764968 ) ) ;
#33591 = CARTESIAN_POINT ( 'NONE',  ( 18.27903665858761073, 9.701928907310005457, -1.500000000000002220 ) ) ;
#33592 = CARTESIAN_POINT ( 'NONE',  ( -14.64807036877012258, -15.96857234361563904, 11.49999999999999645 ) ) ;
#33593 = ORIENTED_EDGE ( 'NONE', *, *, #77273, .T. ) ;
#33594 = CARTESIAN_POINT ( 'NONE',  ( -98.98242597041321744, -25.29000073409625315, 5.621580901835582011 ) ) ;
#33595 = VECTOR ( 'NONE', #74666, 1000.000000000000000 ) ;
#33596 = CARTESIAN_POINT ( 'NONE',  ( -111.7342643247342551, -25.26010494679146490, 3.947561888149926368 ) ) ;
#33597 = CARTESIAN_POINT ( 'NONE',  ( 14.42577177192597482, -17.14957960503723911, -1.500000000000002220 ) ) ;
#33598 = LINE ( 'NONE', #50830, #20549 ) ;
#33599 = DIRECTION ( 'NONE',  ( 2.327730190238734579E-16, -1.000000000000000000, -8.064610422320895277E-16 ) ) ;
#33600 = ORIENTED_EDGE ( 'NONE', *, *, #83381, .T. ) ;
#33601 = CARTESIAN_POINT ( 'NONE',  ( 29.58519688192010832, 4.109013365083094449, 29.12059310601990703 ) ) ;
#33602 = CARTESIAN_POINT ( 'NONE',  ( 12.00135123753652877, -5.092666038735283784, -26.74699110798160007 ) ) ;
#33603 = B_SPLINE_SURFACE_WITH_KNOTS ( 'NONE', 3, 3, ( 
 ( #12375, #74286, #91995, #91492 ),
 ( #99099, #76752, #14366, #21971 ),
 ( #67687, #83383, #21473, #38708 ),
 ( #6264, #76264, #84882, #100083 ),
 ( #36723, #77259, #52953, #92493 ),
 ( #69163, #60575, #82883, #90999 ),
 ( #13369, #30597, #7253, #75765 ) ),
 .UNSPECIFIED., .F., .F., .F.,
 ( 4, 3, 4 ),
 ( 4, 4 ),
 ( 0.0004766839783842195507, 0.1029713700210906219, 0.2054660560637970312 ),
 ( 0.4396058254596823534, 0.4408213833358379796 ),
 .UNSPECIFIED. ) ;
#33604 = VERTEX_POINT ( 'NONE', #19939 ) ;
#33605 = VECTOR ( 'NONE', #27402, 1000.000000000000000 ) ;
#33606 = ORIENTED_EDGE ( 'NONE', *, *, #19791, .T. ) ;
#33607 = CARTESIAN_POINT ( 'NONE',  ( -46.58178904775838447, -24.51419770103157347, 9.386484678747180510 ) ) ;
#33608 = EDGE_LOOP ( 'NONE', ( #37357, #98834, #93567, #25214, #46038, #79751, #92713, #36311, #26314, #18730, #28930, #8133, #55950, #89272, #96636, #96254, #71561, #9112, #65603, #20506, #28392, #54276, #8890, #83146, #65808, #92721, #5811, #25134 ) ) ;
#33609 = CARTESIAN_POINT ( 'NONE',  ( 15.97264540888995299, 3.316774720514426456, -27.93485543958162154 ) ) ;
#33610 = EDGE_CURVE ( 'NONE', #82393, #30291, #45530, .T. ) ;
#33611 = CARTESIAN_POINT ( 'NONE',  ( 1.624102159173431259, 21.17561035156254334, -1.500000000000002220 ) ) ;
#33612 = EDGE_LOOP ( 'NONE', ( #95323, #91493, #69400, #15450 ) ) ;
#33613 = CARTESIAN_POINT ( 'NONE',  ( 22.81105451610979173, 2.682774720514426559, -18.46691820600746681 ) ) ;
#33614 = ADVANCED_FACE ( 'NONE', ( #74236 ), #65654, .T. ) ;
#33615 = CARTESIAN_POINT ( 'NONE',  ( -16.21501377034323710, -14.60173171477820198, 11.49999999999998934 ) ) ;
#33616 = CARTESIAN_POINT ( 'NONE',  ( -103.5871769483072313, -24.51419770103158058, 9.386484678747171628 ) ) ;
#33617 = CARTESIAN_POINT ( 'NONE',  ( 26.74698519091204574, -1.682774720514426114, -10.98683230472874506 ) ) ;
#33618 = CARTESIAN_POINT ( 'NONE',  ( 5.786755829966409692, -5.876774720514414518, 19.89762986309224857 ) ) ;
#33619 = CARTESIAN_POINT ( 'NONE',  ( -21.72861685410901700, 2.547970858986955189, -1.500000000000002220 ) ) ;
#33620 = CARTESIAN_POINT ( 'NONE',  ( 7.166666666666669627, -6.376774720514420736, 20.78665865384615330 ) ) ;
#33621 = ORIENTED_EDGE ( 'NONE', *, *, #71674, .F. ) ;
#33622 = CARTESIAN_POINT ( 'NONE',  ( 25.31657025823196605, 5.174471705609984262, -8.330429310402083232 ) ) ;
#33623 = CARTESIAN_POINT ( 'NONE',  ( -85.63410945799364526, -24.40133493613049964, 9.663955038902802386 ) ) ;
#33624 = EDGE_CURVE ( 'NONE', #12137, #80389, #41291, .T. ) ;
#33625 = ADVANCED_FACE ( 'NONE', ( #59025 ), #42316, .F. ) ;
#33626 = VECTOR ( 'NONE', #98514, 1000.000000000000114 ) ;
#33627 = EDGE_LOOP ( 'NONE', ( #66325, #28987, #38067, #87510 ) ) ;
#33628 = ADVANCED_FACE ( 'NONE', ( #34184 ), #58032, .T. ) ;
#33629 = CARTESIAN_POINT ( 'NONE',  ( -99.62287095715005592, -24.64965695001468404, 8.947790433994178727 ) ) ;
#33630 = ORIENTED_EDGE ( 'NONE', *, *, #34042, .T. ) ;
#33631 = CARTESIAN_POINT ( 'NONE',  ( 9.451856243913134392, 6.475225279485569807, -27.03492916892036746 ) ) ;
#33632 = EDGE_CURVE ( 'NONE', #99483, #71932, #66155, .T. ) ;
#33633 = CARTESIAN_POINT ( 'NONE',  ( -82.64545374615299522, -23.48783264082478084, -1.443836473390069264 ) ) ;
#33634 = CARTESIAN_POINT ( 'NONE',  ( 21.10678091372558640, -2.468637549841573797, -1.500000000000002220 ) ) ;
#33635 = CARTESIAN_POINT ( 'NONE',  ( -57.52287095715005449, -24.64965694238407323, 8.947790433994201820 ) ) ;
#33636 = CARTESIAN_POINT ( 'NONE',  ( -30.61275986115374437, -24.37728322581795481, 9.960208392924579712 ) ) ;
#33637 = DIRECTION ( 'NONE',  ( 3.773278334444167608E-23, -1.000000000000000000, 0.000000000000000000 ) ) ;
#33638 = AXIS2_PLACEMENT_3D ( 'NONE', #13102, #44068, #60806 ) ;
#33639 = CARTESIAN_POINT ( 'NONE',  ( -68.62364069832202063, -24.65952944569304606, 1.056160979905701236 ) ) ;
#33640 = CARTESIAN_POINT ( 'NONE',  ( -8.724563080612403709, -17.33930400145671413, -1.500000000000002220 ) ) ;
#33641 = LINE ( 'NONE', #56991, #24729 ) ;
#33642 = ORIENTED_EDGE ( 'NONE', *, *, #69992, .T. ) ;
#33643 = CARTESIAN_POINT ( 'NONE',  ( 14.32981562401322506, -13.22600733894156200, 11.49999999999999645 ) ) ;
#33644 = FACE_OUTER_BOUND ( 'NONE', #32486, .T. ) ;
#33645 = AXIS2_PLACEMENT_3D ( 'NONE', #68699, #13395, #6783 ) ;
#33646 = CARTESIAN_POINT ( 'NONE',  ( 6.499999999999992895, -1.874386984050377894E-16, 2.100000000000000977 ) ) ;
#33647 = EDGE_CURVE ( 'NONE', #59212, #50584, #95117, .T. ) ;
#33648 = EDGE_LOOP ( 'NONE', ( #76828, #42809, #59147, #53216 ) ) ;
#33649 = CARTESIAN_POINT ( 'NONE',  ( 4.967622410992271753, -6.376774720514415407, 20.05703257908297843 ) ) ;
#33650 = CARTESIAN_POINT ( 'NONE',  ( -89.62358325167234341, -24.65952944569304250, 1.056160979905701902 ) ) ;
#33651 = CARTESIAN_POINT ( 'NONE',  ( 0.000000000000000000, 0.000000000000000000, 6.099999999999999645 ) ) ;
#33652 = CARTESIAN_POINT ( 'NONE',  ( -81.86427935766467101, -25.24813745008903965, 6.429952853325594297 ) ) ;
#33654 = ADVANCED_FACE ( 'NONE', ( #19443 ), #50410, .T. ) ;
#33653 = CARTESIAN_POINT ( 'NONE',  ( 14.14096853472169535, -13.71769858867784464, 11.49999999999998934 ) ) ;
#33655 = ORIENTED_EDGE ( 'NONE', *, *, #57147, .T. ) ;
#33656 = CARTESIAN_POINT ( 'NONE',  ( -78.52287095715003318, -23.73907113216987952, -1.053371485793253015 ) ) ;
#33657 = CARTESIAN_POINT ( 'NONE',  ( -114.5228709571500616, -23.47596703998600631, 11.44779298504228038 ) ) ;
#33658 = EDGE_CURVE ( 'NONE', #61303, #72922, #58821, .T. ) ;
#33659 = DATE_AND_TIME ( #40765, #3573 ) ;
#33660 = DIRECTION ( 'NONE',  ( -3.773278334444166432E-23, 1.000000000000000000, 0.000000000000000000 ) ) ;
#33661 = DIRECTION ( 'NONE',  ( 0.09721092304694055330, 0.000000000000000000, -0.9952638024365006997 ) ) ;
#33662 = CARTESIAN_POINT ( 'NONE',  ( 6.600000000000001421, 0.000000000000000000, 0.000000000000000000 ) ) ;
#33663 = CARTESIAN_POINT ( 'NONE',  ( -17.64648606763744354, -0.3587747205144061202, -23.04404205923973237 ) ) ;
#33664 = CARTESIAN_POINT ( 'NONE',  ( -50.38191529551148307, -29.50248914370730091, 2.832395270851967073 ) ) ;
#33665 = CARTESIAN_POINT ( 'NONE',  ( -69.36083545395123906, -25.24515197910791997, 6.029876749600012964 ) ) ;
#33666 = CARTESIAN_POINT ( 'NONE',  ( -79.52287095715006160, -24.34917612406836795, 0.1852690917426539075 ) ) ;
#33667 = CARTESIAN_POINT ( 'NONE',  ( -13.68957358570155769, -14.46295258127404892, 11.49999999999998934 ) ) ;
#33668 = CARTESIAN_POINT ( 'NONE',  ( -75.63647615153271886, -24.40133493613049964, 9.663955038902805939 ) ) ;
#33669 = CARTESIAN_POINT ( 'NONE',  ( -19.55781625546462976, 3.520333346782119843, -1.500000000000002220 ) ) ;
#33670 = VERTEX_POINT ( 'NONE', #76703 ) ;
#33671 = VECTOR ( 'NONE', #22970, 1000.000000000000000 ) ;
#33672 = DIRECTION ( 'NONE',  ( 0.000000000000000000, -1.000000000000000000, 0.000000000000000000 ) ) ;
#33673 = ADVANCED_FACE ( 'NONE', ( #52902 ), #58035, .T. ) ;
#33674 = B_SPLINE_CURVE_WITH_KNOTS ( 'NONE', 3,
 ( #70864, #69859, #24664, #62763, #24170, #55644 ),
 .UNSPECIFIED., .F., .F.,
 ( 4, 2, 4 ),
 ( 1.570755371633934808E-05, 0.001396183895866086669, 0.002776660238015834278 ),
 .UNSPECIFIED. ) ;
#33675 = CARTESIAN_POINT ( 'NONE',  ( -104.6228709571500559, -23.47596703998600631, 11.44779298504227860 ) ) ;
#33676 = CARTESIAN_POINT ( 'NONE',  ( 30.53060340732036337, 2.682774720514426559, -8.442346167188908623 ) ) ;
#33677 = CARTESIAN_POINT ( 'NONE',  ( 10.24059822343757808, -5.876774720514426953, 0.000000000000000000 ) ) ;
#33678 = CARTESIAN_POINT ( 'NONE',  ( -15.22196369898608737, 14.14466773073655581, 11.49999999999999645 ) ) ;
#33679 = CARTESIAN_POINT ( 'NONE',  ( -7.024122139145243082, -6.376774720514408301, 19.17707164986947532 ) ) ;
#33680 = ADVANCED_FACE ( 'NONE', ( #82342 ), #40881, .T. ) ;
#33681 = CARTESIAN_POINT ( 'NONE',  ( -51.26161549125684758, -25.24476575314045945, 3.786882481863750094 ) ) ;
#33682 = CARTESIAN_POINT ( 'NONE',  ( 2.723195454624489642, 22.67993996152103620, 11.49999999999999645 ) ) ;
#33683 = VERTEX_POINT ( 'NONE', #15820 ) ;
#33684 = B_SPLINE_SURFACE_WITH_KNOTS ( 'NONE', 3, 3, ( 
 ( #74372, #51550, #34321, #90103 ),
 ( #19581, #81989, #28705, #51050 ),
 ( #81495, #28202, #27210, #35816 ),
 ( #96223, #4868, #27708, #96707 ),
 ( #73387, #66790, #98195, #43929 ),
 ( #19080, #12473, #20577, #58654 ),
 ( #82480, #89602, #97708, #3882 ) ),
 .UNSPECIFIED., .F., .F., .F.,
 ( 4, 3, 4 ),
 ( 4, 4 ),
 ( 0.7945040050992233649, 0.8970133687736495665, 0.9995227324480757680 ),
 ( 0.1695370789669584655, 0.1706280730879164986 ),
 .UNSPECIFIED. ) ;
#33685 = CARTESIAN_POINT ( 'NONE',  ( -54.62287095715005592, -23.47593901973091235, -1.443836447539009749 ) ) ;
#33686 = CARTESIAN_POINT ( 'NONE',  ( -127.5906365579869970, -23.48783264082477018, -1.443836473390083919 ) ) ;
#33687 = EDGE_LOOP ( 'NONE', ( #30755, #48886, #39166, #34112 ) ) ;
#33688 = CARTESIAN_POINT ( 'NONE',  ( -14.42758394406654610, -14.16023863206117994, 11.49999999999998934 ) ) ;
#33689 = CARTESIAN_POINT ( 'NONE',  ( -89.62287095715004170, -23.47596703998600631, 11.44779298504227860 ) ) ;
#33690 = DIRECTION ( 'NONE',  ( 0.000000000000000000, 0.000000000000000000, -1.000000000000000000 ) ) ;
#33691 = AXIS2_PLACEMENT_3D ( 'NONE', #78939, #32777, #9939 ) ;
#33692 = CARTESIAN_POINT ( 'NONE',  ( -100.6228709571500559, -23.48783264082478794, -1.443836473390061936 ) ) ;
#33693 = B_SPLINE_CURVE_WITH_KNOTS ( 'NONE', 3,
 ( #2114, #25933, #57905, #72124 ),
 .UNSPECIFIED., .F., .F.,
 ( 4, 4 ),
 ( 0.000000000000000000, 9.999999999998897304E-05 ),
 .UNSPECIFIED. ) ;
#33694 = ORIENTED_EDGE ( 'NONE', *, *, #25362, .F. ) ;
#33695 = CARTESIAN_POINT ( 'NONE',  ( -45.62287095715004881, -29.50248789122583659, 2.256150453626215580 ) ) ;
#33696 = CARTESIAN_POINT ( 'NONE',  ( -100.6228709571500843, -24.51163499207179441, 0.6490370598555492698 ) ) ;
#33697 = CARTESIAN_POINT ( 'NONE',  ( 8.874027960929927517, 17.90919871486395465, -1.500000000000002220 ) ) ;
#33698 = CARTESIAN_POINT ( 'NONE',  ( -11.48448384864204996, -17.54081393385053644, 11.49999999999999645 ) ) ;
#33699 = DIRECTION ( 'NONE',  ( 0.7071067811865474617, -0.000000000000000000, 0.7071067811865476838 ) ) ;
#33700 = DIRECTION ( 'NONE',  ( 0.000000000000000000, -1.000000000000000000, 0.000000000000000000 ) ) ;
#33701 = CARTESIAN_POINT ( 'NONE',  ( 19.60348439636399931, 10.09110264789753053, 11.49999999999998934 ) ) ;
#33702 = VECTOR ( 'NONE', #57571, 1000.000000000000000 ) ;
#33703 = CARTESIAN_POINT ( 'NONE',  ( -53.55620429048338593, -24.64965694238574656, 8.947790433994208925 ) ) ;
#33704 = ORIENTED_EDGE ( 'NONE', *, *, #30626, .T. ) ;
#33705 = CARTESIAN_POINT ( 'NONE',  ( -127.5228709571500616, -23.48786465467242479, 11.44779295918253581 ) ) ;
#33706 = CARTESIAN_POINT ( 'NONE',  ( -129.6228709571500417, -29.50248528299804818, 1.056150453629047137 ) ) ;
#33707 = CARTESIAN_POINT ( 'NONE',  ( -72.60175781541748563, -23.73766607897670156, -1.055555164236458454 ) ) ;
#33708 = ORIENTED_EDGE ( 'NONE', *, *, #42038, .F. ) ;
#33709 = CARTESIAN_POINT ( 'NONE',  ( 19.75748517575715368, -5.965225279485572685, 28.87153971905864580 ) ) ;
#33710 = ORIENTED_EDGE ( 'NONE', *, *, #79272, .F. ) ;
#33711 = AXIS2_PLACEMENT_3D ( 'NONE', #55869, #26899, #73087 ) ;
#33712 = ORIENTED_EDGE ( 'NONE', *, *, #47750, .T. ) ;
#33713 = DIRECTION ( 'NONE',  ( 0.1478094111296165691, -0.9890158633619158257, 0.000000000000000000 ) ) ;
#33714 = CARTESIAN_POINT ( 'NONE',  ( -28.32169924589829080, 5.965225279485592225, -8.244178532169447848 ) ) ;
#33715 = DIRECTION ( 'NONE',  ( -3.773278334453080206E-23, 0.9999999999976377785, 2.173523156925979975E-06 ) ) ;
#33716 = CARTESIAN_POINT ( 'NONE',  ( 15.43701773751798001, -13.56989305476470875, -1.500000000000002220 ) ) ;
#33717 = EDGE_LOOP ( 'NONE', ( #34759, #23483, #62576, #64956 ) ) ;
#33718 = CARTESIAN_POINT ( 'NONE',  ( -51.62287095715005592, -29.50248528299804818, 1.056150453629033370 ) ) ;
#33719 = PLANE ( 'NONE',  #90414 ) ;
#33720 = LINE ( 'NONE', #25603, #36675 ) ;
#33721 = CARTESIAN_POINT ( 'NONE',  ( -1.228339276683141579, -22.28195500894762660, 11.49999999999998934 ) ) ;
#33722 = CARTESIAN_POINT ( 'NONE',  ( 10.24059822343757986, -5.876774720514426953, 22.82308057603840368 ) ) ;
#33723 = CARTESIAN_POINT ( 'NONE',  ( -35.62287095715005592, -29.50248789122583659, 2.256150453626215580 ) ) ;
#33724 = ORIENTED_EDGE ( 'NONE', *, *, #57149, .T. ) ;
#33725 = CARTESIAN_POINT ( 'NONE',  ( 30.93860345374796594, 0.000000000000000000, 0.000000000000000000 ) ) ;
#33726 = LINE ( 'NONE', #1779, #3751 ) ;
#33727 = VECTOR ( 'NONE', #5700, 1000.000000000000114 ) ;
#33728 = CARTESIAN_POINT ( 'NONE',  ( 20.34438994040483806, -4.565235006643893811, 11.49999999999998934 ) ) ;
#33729 = ORIENTED_EDGE ( 'NONE', *, *, #72628, .T. ) ;
#33731 = EDGE_LOOP ( 'NONE', ( #22194, #19878, #97373, #73025 ) ) ;
#33730 = CARTESIAN_POINT ( 'NONE',  ( -61.62287095715004881, -23.47596703998600631, 11.44779298504227505 ) ) ;
#33732 = EDGE_LOOP ( 'NONE', ( #90771, #67911, #57129, #48988 ) ) ;
#33733 = CARTESIAN_POINT ( 'NONE',  ( -69.03624148920614800, -25.25935168378925866, 6.724186225230494252 ) ) ;
#33734 = CARTESIAN_POINT ( 'NONE',  ( 7.388015978253313243, 19.69965359013245632, -1.500000000000002220 ) ) ;
#33735 = ORIENTED_EDGE ( 'NONE', *, *, #66964, .T. ) ;
#33736 = CARTESIAN_POINT ( 'NONE',  ( -114.5228709571500616, -23.48783264083396105, -1.443836473375806895 ) ) ;
#33738 = ADVANCED_FACE ( 'NONE', ( #94454 ), #1619, .T. ) ;
#33737 = PLANE ( 'NONE',  #56368 ) ;
#33739 = FACE_OUTER_BOUND ( 'NONE', #40198, .T. ) ;
#33740 = B_SPLINE_CURVE_WITH_KNOTS ( 'NONE', 3,
 ( #73392, #65303, #11478, #58169 ),
 .UNSPECIFIED., .F., .F.,
 ( 4, 4 ),
 ( 6.276132038432468235E-06, 0.001058024727852768581 ),
 .UNSPECIFIED. ) ;
#33741 = CARTESIAN_POINT ( 'NONE',  ( -86.62607985270027200, -24.51419770103155926, 9.386484678747176957 ) ) ;
#33742 = CARTESIAN_POINT ( 'NONE',  ( -73.58953762381673869, -24.65952944569304606, 1.056160979905698794 ) ) ;
#33743 = CARTESIAN_POINT ( 'NONE',  ( 5.343276940429747768, -21.04383479052346217, -1.500000000000002220 ) ) ;
#33744 = CARTESIAN_POINT ( 'NONE',  ( -64.52287095715009002, -24.33927499327855770, 9.819080762295815390 ) ) ;
#33746 = ORIENTED_EDGE ( 'NONE', *, *, #13130, .T. ) ;
#33745 = CARTESIAN_POINT ( 'NONE',  ( -4.481184387785930312, -21.81124396384582909, 11.49999999999999645 ) ) ;
#33747 = CARTESIAN_POINT ( 'NONE',  ( -51.52443300084429723, -25.24728917589673216, 6.090565017594450126 ) ) ;
#33748 = CARTESIAN_POINT ( 'NONE',  ( 8.940588884021780203, 1.067603002178827815E-16, -3.692441190372577342 ) ) ;
#33749 = LINE ( 'NONE', #86525, #48937 ) ;
#33750 = ORIENTED_EDGE ( 'NONE', *, *, #62657, .F. ) ;
#33751 = EDGE_CURVE ( 'NONE', #27602, #90358, #92442, .T. ) ;
#33752 = EDGE_CURVE ( 'NONE', #30676, #100208, #16828, .T. ) ;
#33754 = VERTEX_POINT ( 'NONE', #77710 ) ;
#33753 = CARTESIAN_POINT ( 'NONE',  ( -110.6228709571500559, -29.50249982740957577, 7.747779886224967605 ) ) ;
#33755 = EDGE_LOOP ( 'NONE', ( #93356, #45490, #50401, #64120 ) ) ;
#33756 = EDGE_CURVE ( 'NONE', #74029, #21350, #85820, .T. ) ;
#33757 = DIRECTION ( 'NONE',  ( -3.773278334453079618E-23, 0.9999999999976377785, 2.173523156925979975E-06 ) ) ;
#33758 = CARTESIAN_POINT ( 'NONE',  ( -35.52287095715007581, -24.62226745350439217, 0.9660975649728085202 ) ) ;
#33759 = CARTESIAN_POINT ( 'NONE',  ( 8.349999999999972999, 27.69999999999999574, 0.000000000000000000 ) ) ;
#33760 = ORIENTED_EDGE ( 'NONE', *, *, #71363, .T. ) ;
#33761 = CARTESIAN_POINT ( 'NONE',  ( -130.5728709571500588, -25.39039004847436232, 5.722739179073901283 ) ) ;
#33762 = CARTESIAN_POINT ( 'NONE',  ( -22.26391555059773353, 2.265117081278330780, -1.500000000000002220 ) ) ;
#33763 = ORIENTED_EDGE ( 'NONE', *, *, #77430, .F. ) ;
#33764 = EDGE_LOOP ( 'NONE', ( #40688, #28441, #69164, #12954 ) ) ;
#33765 = CARTESIAN_POINT ( 'NONE',  ( -34.52287095715006160, -24.33927499327853994, 9.819080762295811837 ) ) ;
#33766 = LINE ( 'NONE', #79931, #55655 ) ;
#33767 = PLANE ( 'NONE',  #78207 ) ;
#33768 = DIRECTION ( 'NONE',  ( -1.012712320732673682E-13, 0.000000000000000000, 1.000000000000000000 ) ) ;
#33769 = VECTOR ( 'NONE', #91682, 1000.000000000000000 ) ;
#33770 = CARTESIAN_POINT ( 'NONE',  ( -130.5728709571500588, -24.82959736273287632, 8.370978854367631783 ) ) ;
#33771 = CARTESIAN_POINT ( 'NONE',  ( -15.85469643196389278, -11.46343829903102396, -1.500000000000002220 ) ) ;
#33772 = CARTESIAN_POINT ( 'NONE',  ( -49.50841769935765768, -25.27292115247390569, 3.984447733149576898 ) ) ;
#33773 = ORIENTED_EDGE ( 'NONE', *, *, #55304, .F. ) ;
#33774 = CARTESIAN_POINT ( 'NONE',  ( 2.436486579176012413, 21.40072447632485364, -1.500000000000002220 ) ) ;
#33775 = CARTESIAN_POINT ( 'NONE',  ( -64.52287095715006160, -29.50250786944525672, 11.44777988621623876 ) ) ;
#33776 = CARTESIAN_POINT ( 'NONE',  ( -119.5895376238167245, -23.47596703998600631, 11.44779298504227683 ) ) ;
#33777 = DIRECTION ( 'NONE',  ( -0.000000000000000000, 0.000000000000000000, 1.000000000000000000 ) ) ;
#33778 = CARTESIAN_POINT ( 'NONE',  ( 32.84232313084847732, 4.840274619473232676, -11.71291885348859196 ) ) ;
#33779 = CARTESIAN_POINT ( 'NONE',  ( 21.34038654641452482, 8.310931564070170197, -1.500000000000002220 ) ) ;
#33780 = APPROVAL_STATUS ( 'not_yet_approved' ) ;
#33781 = CARTESIAN_POINT ( 'NONE',  ( -39.62287095715005592, -29.50248528299804818, 1.056150453629031594 ) ) ;
#33782 = DIRECTION ( 'NONE',  ( -0.000000000000000000, -0.000000000000000000, -1.000000000000000000 ) ) ;
#33783 = CARTESIAN_POINT ( 'NONE',  ( -18.39468835979788608, -8.022455445098881199, 11.49999999999999645 ) ) ;
#33784 = LINE ( 'NONE', #64769, #13838 ) ;
#33785 = DIRECTION ( 'NONE',  ( -3.773278334453079618E-23, 0.9999999999976377785, 2.173523156925979975E-06 ) ) ;
#33786 = AXIS2_PLACEMENT_3D ( 'NONE', #53576, #61191, #62180 ) ;
#33787 = DIRECTION ( 'NONE',  ( 0.000000000000000000, 2.173523156925980399E-06, -0.9999999999976378895 ) ) ;
#33788 = CARTESIAN_POINT ( 'NONE',  ( 15.15958133180904355, 5.152774720514426754, -26.63299148310930420 ) ) ;
#33789 = CARTESIAN_POINT ( 'NONE',  ( -126.5228709571500616, -24.64965694238408034, 8.947790433994189385 ) ) ;
#33790 = CARTESIAN_POINT ( 'NONE',  ( 9.833179757865110560, 17.22857952739193266, 11.49999999999998934 ) ) ;
#33791 = FACE_OUTER_BOUND ( 'NONE', #8786, .T. ) ;
#33792 = CARTESIAN_POINT ( 'NONE',  ( 11.96684523812195700, 15.63349346248531546, -1.500000000000002220 ) ) ;
#33793 = CARTESIAN_POINT ( 'NONE',  ( -42.59367499821067327, -24.15543982623907127, -0.2315651400026575435 ) ) ;
#33794 = AXIS2_PLACEMENT_3D ( 'NONE', #50407, #58523, #88467 ) ;
#33795 = PLANE ( 'NONE',  #53207 ) ;
#33796 = CALENDAR_DATE ( 2026, 9, 10 ) ;
#33797 = CARTESIAN_POINT ( 'NONE',  ( 15.98199071239991120, 3.493868136757070975, -27.92664602931597884 ) ) ;
#33798 = CARTESIAN_POINT ( 'NONE',  ( 3.202571139211427553, -6.376774720514406525, 18.81074098386681470 ) ) ;
#33799 = CARTESIAN_POINT ( 'NONE',  ( 19.39950376024442846, -7.079068461131618584, 11.49999999999999645 ) ) ;
#33800 = CARTESIAN_POINT ( 'NONE',  ( 4.373554412633047228, -6.376774720514422512, 21.19197260575996822 ) ) ;
#33801 = ADVANCED_FACE ( 'NONE', ( #54902 ), #86836, .T. ) ;
#33802 = DIRECTION ( 'NONE',  ( -1.797640907747986603E-16, 1.000000000000000000, 0.000000000000000000 ) ) ;
#33803 = CARTESIAN_POINT ( 'NONE',  ( -19.18631400275845422, -11.98935526391121087, 11.49999999999999645 ) ) ;
#33804 = ORIENTED_EDGE ( 'NONE', *, *, #69988, .T. ) ;
#33805 = ADVANCED_FACE ( 'NONE', ( #8726 ), #85843, .F. ) ;
#33806 = CARTESIAN_POINT ( 'NONE',  ( -72.62287095715005592, -29.50248528299804818, 1.056150453629036701 ) ) ;
#33807 = CARTESIAN_POINT ( 'NONE',  ( -97.55776836362488780, -23.73766607897671221, -1.055555164236451793 ) ) ;
#33808 = CARTESIAN_POINT ( 'NONE',  ( -26.76727616692972234, -24.79064461044202616, 2.646210252706996169 ) ) ;
#33809 = CARTESIAN_POINT ( 'NONE',  ( -26.85174826923451974, -24.93063591732613204, 8.053059820581612627 ) ) ;
#33810 = CARTESIAN_POINT ( 'NONE',  ( 1.600000000000000755, 2.939152317953647894E-15, -24.00000000000000000 ) ) ;
#33811 = ORIENTED_EDGE ( 'NONE', *, *, #56400, .T. ) ;
#33812 = CARTESIAN_POINT ( 'NONE',  ( -79.57226238056755108, -25.31596297220300329, 5.312438930566553807 ) ) ;
#33813 = CARTESIAN_POINT ( 'NONE',  ( 9.452765381649220089, 20.79790602042944414, 11.49999999999998934 ) ) ;
#33814 = CARTESIAN_POINT ( 'NONE',  ( 2.499999999999995115, 19.99999999999999645, 0.000000000000000000 ) ) ;
#33815 = CARTESIAN_POINT ( 'NONE',  ( -91.52287095715006160, -23.47593901973090524, -1.443836447538996648 ) ) ;
#33816 = FACE_OUTER_BOUND ( 'NONE', #56436, .T. ) ;
#33817 = CARTESIAN_POINT ( 'NONE',  ( 14.28312119630281174, -17.39864199977734671, 11.49999999999999645 ) ) ;
#33818 = ORIENTED_EDGE ( 'NONE', *, *, #56665, .T. ) ;
#33819 = CARTESIAN_POINT ( 'NONE',  ( -43.54651782967658136, -24.15543982623906771, -0.2315651400026568496 ) ) ;
#33820 = CARTESIAN_POINT ( 'NONE',  ( -20.58003014649542095, 7.718188279156099618, -1.500000000000002220 ) ) ;
#33821 = DIRECTION ( 'NONE',  ( 0.1254312216594016538, 0.000000000000000000, 0.9921023176230513441 ) ) ;
#33822 = CARTESIAN_POINT ( 'NONE',  ( 22.81105451610979173, -500000.0000000000582, -18.46691820600746681 ) ) ;
#33823 = CARTESIAN_POINT ( 'NONE',  ( -29.24573430514233507, -24.79699791941041553, 5.187749665486013129 ) ) ;
#33824 = VERTEX_POINT ( 'NONE', #70619 ) ;
#33825 = CARTESIAN_POINT ( 'NONE',  ( -48.63354421635416003, -24.35071581493542681, 9.817618358456027039 ) ) ;
#33826 = CARTESIAN_POINT ( 'NONE',  ( -0.3544984435505275644, -6.376774720514408301, 19.15251819062245531 ) ) ;
#33827 = ORIENTED_EDGE ( 'NONE', *, *, #38960, .T. ) ;
#33828 = CARTESIAN_POINT ( 'NONE',  ( -54.59312836098206390, -24.15620529776628089, 10.23563542870661180 ) ) ;
#33829 = CARTESIAN_POINT ( 'NONE',  ( 14.40702264168333890, -14.58922348230443689, -1.500000000000002220 ) ) ;
#33830 = ORIENTED_EDGE ( 'NONE', *, *, #44876, .T. ) ;
#33831 = VECTOR ( 'NONE', #59728, 1000.000000000000000 ) ;
#33832 = ORIENTED_EDGE ( 'NONE', *, *, #52311, .F. ) ;
#33833 = ORIENTED_EDGE ( 'NONE', *, *, #10258, .F. ) ;
#33834 = CARTESIAN_POINT ( 'NONE',  ( -72.52287095715007581, -23.47593901973090169, -1.443836447538996870 ) ) ;
#33835 = CARTESIAN_POINT ( 'NONE',  ( 16.03631736716203449, -16.64276770305488284, 11.49999999999998934 ) ) ;
#33836 = CARTESIAN_POINT ( 'NONE',  ( -104.5511856791031562, -24.35071581493544102, 9.817618358456019934 ) ) ;
#33837 = CARTESIAN_POINT ( 'NONE',  ( -7.038884989605349141, -19.10714869031923513, -1.500000000000002220 ) ) ;
#33838 = ORIENTED_EDGE ( 'NONE', *, *, #87120, .T. ) ;
#33839 = DIRECTION ( 'NONE',  ( 0.000000000000000000, -3.740886741919572836E-15, -1.000000000000000000 ) ) ;
#33840 = VECTOR ( 'NONE', #37464, 1000.000000000000000 ) ;
#33841 = CARTESIAN_POINT ( 'NONE',  ( -51.69051972431498143, -25.25860399288287894, 3.823735972406262729 ) ) ;
#33842 = ADVANCED_FACE ( 'NONE', ( #17328 ), #75059, .T. ) ;
#33843 = CARTESIAN_POINT ( 'NONE',  ( -93.62287095715011276, -23.95044443724992789, 10.65354141964649592 ) ) ;
#33844 = CARTESIAN_POINT ( 'NONE',  ( 18.72495633783376334, 0.000000000000000000, -1.691563534834430227 ) ) ;
#33845 = EDGE_LOOP ( 'NONE', ( #55554, #96742, #70898, #78339 ) ) ;
#33846 = CARTESIAN_POINT ( 'NONE',  ( -27.75618988833547718, -24.76880854971131996, 2.278559976844410695 ) ) ;
#33847 = CARTESIAN_POINT ( 'NONE',  ( -9.278253834636469577, -5.876774720514426953, 21.48128695274316158 ) ) ;
#33848 = ORIENTED_EDGE ( 'NONE', *, *, #30963, .F. ) ;
#33849 = VECTOR ( 'NONE', #89715, 1000.000000000000000 ) ;
#33850 = B_SPLINE_CURVE_WITH_KNOTS ( 'NONE', 3,
 ( #37791, #67758, #99174, #7323 ),
 .UNSPECIFIED., .F., .F.,
 ( 4, 4 ),
 ( 0.000000000000000000, 1.000000000000000000 ),
 .UNSPECIFIED. ) ;
#33851 = CARTESIAN_POINT ( 'NONE',  ( 10.28901978357889035, -18.02705789925236957, 11.49999999999998934 ) ) ;
#33852 = ORIENTED_EDGE ( 'NONE', *, *, #35569, .T. ) ;
#33854 = VERTEX_POINT ( 'NONE', #8223 ) ;
#33853 = LINE ( 'NONE', #17120, #84751 ) ;
#33855 = CARTESIAN_POINT ( 'NONE',  ( 28.87399897812680649, -1.682774720514426114, -12.57761096169975801 ) ) ;
#33856 = DIRECTION ( 'NONE',  ( 0.000000000000000000, -0.9999999999976377785, -2.173523156925979975E-06 ) ) ;
#33857 = EDGE_LOOP ( 'NONE', ( #65966, #41345, #99673, #39600 ) ) ;
#33858 = ORIENTED_EDGE ( 'NONE', *, *, #84533, .F. ) ;
#33859 = CARTESIAN_POINT ( 'NONE',  ( -29.62287095715004881, -23.64899563800052817, -1.053577770480854436 ) ) ;
#33860 = EDGE_CURVE ( 'NONE', #50489, #41964, #92330, .T. ) ;
#33861 = VECTOR ( 'NONE', #54525, 1000.000000000000000 ) ;
#33862 = CARTESIAN_POINT ( 'NONE',  ( 7.160000000000000142, 7.891155995661684130, 5.788828319098143993 ) ) ;
#33863 = CARTESIAN_POINT ( 'NONE',  ( -28.59316516807098196, -24.74616672227249481, 1.851678086324305861 ) ) ;
#33865 = VERTEX_POINT ( 'NONE', #96455 ) ;
#33864 = CARTESIAN_POINT ( 'NONE',  ( 18.18892703665305177, -12.56521834855340281, 11.49999999999999645 ) ) ;
#33866 = CARTESIAN_POINT ( 'NONE',  ( -108.5964263034907873, -23.48783264082478794, -1.443836473390062825 ) ) ;
#33867 = EDGE_CURVE ( 'NONE', #90247, #80731, #30948, .T. ) ;
#33868 = CARTESIAN_POINT ( 'NONE',  ( -18.09186581907994196, -13.49991075323410250, -1.500000000000002220 ) ) ;
#33869 = EDGE_CURVE ( 'NONE', #70921, #76784, #14539, .T. ) ;
#33871 = EDGE_LOOP ( 'NONE', ( #95171, #26022, #74620, #7763 ) ) ;
#33870 = DIRECTION ( 'NONE',  ( -3.773278334453080206E-23, 0.9999999999976377785, 2.173523156925979975E-06 ) ) ;
#33872 = EDGE_CURVE ( 'NONE', #70264, #82528, #66038, .T. ) ;
#33873 = VERTEX_POINT ( 'NONE', #65538 ) ;
#33874 = ADVANCED_FACE ( 'NONE', ( #42689 ), #85687, .T. ) ;
#33875 = CARTESIAN_POINT ( 'NONE',  ( -127.5228709571500616, -23.47593901973090524, -1.443836447538996204 ) ) ;
#33876 = VECTOR ( 'NONE', #60251, 1000.000000000000000 ) ;
#33877 = DIRECTION ( 'NONE',  ( 0.000000000000000000, 0.000000000000000000, 1.000000000000000000 ) ) ;
#33878 = ORIENTED_EDGE ( 'NONE', *, *, #42606, .F. ) ;
#33879 = CARTESIAN_POINT ( 'NONE',  ( 4.708956132399880978, 20.65895737721473679, -1.500000000000002220 ) ) ;
#33880 = CARTESIAN_POINT ( 'NONE',  ( 29.70397367894831930, -3.853389802531868469, 28.15179473738050220 ) ) ;
#33881 = CARTESIAN_POINT ( 'NONE',  ( -32.62287095715006302, -23.47596703998600276, 11.44779298504227505 ) ) ;
#33882 = LINE ( 'NONE', #33373, #89180 ) ;
#33883 = CARTESIAN_POINT ( 'NONE',  ( -17.21897301287555848, -14.04741862099043104, -1.500000000000002220 ) ) ;
#33884 = CARTESIAN_POINT ( 'NONE',  ( -114.5584126538706045, -23.48783264082478794, -1.443836473390062380 ) ) ;
#33885 = EDGE_CURVE ( 'NONE', #42129, #34509, #62416, .T. ) ;
#33886 = EDGE_LOOP ( 'NONE', ( #3516, #47688, #3405, #85596, #50816 ) ) ;
#33887 = CARTESIAN_POINT ( 'NONE',  ( -29.62287095715004881, -29.50247984919044697, -1.443849411171584940 ) ) ;
#33888 = CARTESIAN_POINT ( 'NONE',  ( -50.55620429048339304, -23.47596703998600276, 11.44779298504227505 ) ) ;
#33889 = LINE ( 'NONE', #64873, #44734 ) ;
#33890 = CARTESIAN_POINT ( 'NONE',  ( -49.52287095715004739, -24.66019654487198665, 8.947790411086131712 ) ) ;
#33891 = CARTESIAN_POINT ( 'NONE',  ( -19.46337940159461866, -0.4807646128305608779, -1.500000000000002220 ) ) ;
#33892 = CARTESIAN_POINT ( 'NONE',  ( 21.36505145794347982, 1.902718533054148509, 11.49999999999998934 ) ) ;
#33893 = CARTESIAN_POINT ( 'NONE',  ( -85.52287095715004739, -24.99156044556120193, 7.747789690856173195 ) ) ;
#33894 = CARTESIAN_POINT ( 'NONE',  ( -0.5830141525297981575, -5.876774720514410077, 19.15054976246387497 ) ) ;
#33895 = FACE_OUTER_BOUND ( 'NONE', #54339, .T. ) ;
#33896 = DIRECTION ( 'NONE',  ( -0.9161084732596777025, 0.000000000000000000, 0.4009304992412306978 ) ) ;
#33897 = CARTESIAN_POINT ( 'NONE',  ( -22.42851769774927817, -3.676000928666301792, -1.500000000000002220 ) ) ;
#33898 = B_SPLINE_CURVE_WITH_KNOTS ( 'NONE', 3,
 ( #41029, #3470, #57756, #33907, #42535, #71982 ),
 .UNSPECIFIED., .F., .F.,
 ( 4, 2, 4 ),
 ( 0.000000000000000000, 0.001380901958385395700, 0.002761803916770791401 ),
 .UNSPECIFIED. ) ;
#33899 = DIRECTION ( 'NONE',  ( -1.909006365409800904E-24, 1.000000000000000000, -6.950561949739505919E-24 ) ) ;
#33900 = CARTESIAN_POINT ( 'NONE',  ( -102.5170246378254149, -23.96119346886881729, -0.6495511937831880411 ) ) ;
#33901 = LINE ( 'NONE', #19164, #37890 ) ;
#33902 = CARTESIAN_POINT ( 'NONE',  ( -1.646307629438301667, 19.86461321233117872, 11.49999999999999645 ) ) ;
#33903 = CARTESIAN_POINT ( 'NONE',  ( -104.6250152058018870, -24.51314013834316796, 0.6176544820404187286 ) ) ;
#33904 = VECTOR ( 'NONE', #83475, 1000.000000000000000 ) ;
#33905 = CIRCLE ( 'NONE', #3132, 80.18232118519038920 ) ;
#33906 = B_SPLINE_CURVE_WITH_KNOTS ( 'NONE', 3,
 ( #22610, #38854, #7397, #99733, #61219, #38356, #16010, #23614, #293, #92138, #14011, #85525, #8405, #39357, #70315, #53604, #75911, #53101, #69308, #6416 ),
 .UNSPECIFIED., .F., .F.,
 ( 4, 2, 2, 2, 2, 2, 2, 2, 2, 4 ),
 ( 0.000000000000000000, 0.0008691610528771086383, 0.001303741579315663337, 0.001738322105754218144, 0.002172902632192772517, 0.002390192895412054149, 0.002607483158631335781, 0.003042063685069898177, 0.003259353948289179376, 0.003476644211508461008 ),
 .UNSPECIFIED. ) ;
#33907 = CARTESIAN_POINT ( 'NONE',  ( -128.5228709571499621, -23.95044443724993144, 10.65354141964648704 ) ) ;
#33908 = CARTESIAN_POINT ( 'NONE',  ( -118.6228709571500559, -23.47593901973091235, -1.443836447538997536 ) ) ;
#33909 = ORIENTED_EDGE ( 'NONE', *, *, #70970, .F. ) ;
#33910 = DIRECTION ( 'NONE',  ( -1.000000000000000000, -3.773278334444167608E-23, -8.201307833595939069E-29 ) ) ;
#33911 = DIRECTION ( 'NONE',  ( 0.000000000000000000, 1.000000000000000000, 0.000000000000000000 ) ) ;
#33912 = CARTESIAN_POINT ( 'NONE',  ( -14.64807036877012258, -15.96857234361563904, 11.49999999999998934 ) ) ;
#33913 = CARTESIAN_POINT ( 'NONE',  ( -51.91883209273765232, -25.23905552336719182, 6.365853120814609412 ) ) ;
#33914 = VECTOR ( 'NONE', #19369, 1000.000000000000114 ) ;
#33915 = CARTESIAN_POINT ( 'NONE',  ( 9.662506626059768067, -16.94115208737379774, -1.500000000000002220 ) ) ;
#33916 = FACE_OUTER_BOUND ( 'NONE', #70637, .T. ) ;
#33917 = EDGE_CURVE ( 'NONE', #65922, #60254, #70962, .T. ) ;
#33918 = VERTEX_POINT ( 'NONE', #79056 ) ;
#33919 = VECTOR ( 'NONE', #82492, 1000.000000000000000 ) ;
#33920 = PERSON_AND_ORGANIZATION_ROLE ( 'classification_officer' ) ;
#33921 = CIRCLE ( 'NONE', #7975, 6.000000000000000888 ) ;
#33922 = CARTESIAN_POINT ( 'NONE',  ( -59.62287095715004881, -24.64965695001468404, 8.947790433994185832 ) ) ;
#33923 = CARTESIAN_POINT ( 'NONE',  ( 0.3735783541106268979, -20.45636175344465713, 11.49999999999999645 ) ) ;
#33924 = CARTESIAN_POINT ( 'NONE',  ( -29.49875734969026198, -5.965225279485572685, 0.1180228001186258285 ) ) ;
#33925 = EDGE_CURVE ( 'NONE', #82260, #9871, #84215, .T. ) ;
#33926 = CARTESIAN_POINT ( 'NONE',  ( -101.5468792378191978, -25.24282061761980955, 6.236250683194342059 ) ) ;
#33927 = ORIENTED_EDGE ( 'NONE', *, *, #17913, .T. ) ;
#33928 = CARTESIAN_POINT ( 'NONE',  ( -55.52287095715006870, -23.48786465467241058, 11.44779295918254824 ) ) ;
#33929 = CARTESIAN_POINT ( 'NONE',  ( 6.660000000000001030, 2.888964624466060727, -0.2527516539682188035 ) ) ;
#33930 = CARTESIAN_POINT ( 'NONE',  ( 30.57287095715021508, -5.759977553574911369, 25.41160796525321786 ) ) ;
#33931 = CARTESIAN_POINT ( 'NONE',  ( -49.29568538784691611, -25.31439443837986403, 5.964271667760576712 ) ) ;
#33932 = B_SPLINE_CURVE_WITH_KNOTS ( 'NONE', 3,
 ( #99798, #30305, #60780, #84095, #61283, #46542, #69376, #360 ),
 .UNSPECIFIED., .F., .F.,
 ( 4, 2, 2, 4 ),
 ( -0.001240355328176665156, -0.0002398155169398032398, 0.0007607242942970586768, 0.002761803916770783594 ),
 .UNSPECIFIED. ) ;
#33933 = CARTESIAN_POINT ( 'NONE',  ( -109.5552946845191826, -23.96119346886880663, -0.6495511937832053606 ) ) ;
#33934 = ORIENTED_EDGE ( 'NONE', *, *, #26422, .F. ) ;
#33935 = CARTESIAN_POINT ( 'NONE',  ( -66.52209599655327565, -23.48786465467241058, 11.44779295918254824 ) ) ;
#33936 = CARTESIAN_POINT ( 'NONE',  ( -8.204236019480731557, -21.45505762417899831, 11.49999999999999645 ) ) ;
#33937 = CARTESIAN_POINT ( 'NONE',  ( 16.48639501038195121, -15.69157857782056276, -1.500000000000002220 ) ) ;
#33938 = CARTESIAN_POINT ( 'NONE',  ( 4.585161930874343206, -6.376774720514427841, 21.47592444013076118 ) ) ;
#33939 = CARTESIAN_POINT ( 'NONE',  ( -28.84663072490566194, -0.3587747205144265483, 28.73989617533406715 ) ) ;
#33940 = CARTESIAN_POINT ( 'NONE',  ( -90.64148924035946209, -23.85016227208580730, -0.8807180028928307536 ) ) ;
#33941 = CARTESIAN_POINT ( 'NONE',  ( -74.52287095715010423, -23.96177878511308279, 10.65340807706329684 ) ) ;
#33942 = PLANE ( 'NONE',  #38407 ) ;
#33943 = CARTESIAN_POINT ( 'NONE',  ( -21.72861685410901700, 2.547970858986955189, -1.500000000000002220 ) ) ;
#33944 = CC_DESIGN_PERSON_AND_ORGANIZATION_ASSIGNMENT ( #1838, #18051, ( #50676 ) ) ;
#33945 = CARTESIAN_POINT ( 'NONE',  ( -69.62708888908201743, -24.51419770103157347, 9.386484678747178734 ) ) ;
#33946 = CIRCLE ( 'NONE', #69355, 27.94799999999999685 ) ;
#33947 = CARTESIAN_POINT ( 'NONE',  ( -48.87835844652435213, -25.27427334345122034, 6.006362479330361381 ) ) ;
#33948 = CARTESIAN_POINT ( 'NONE',  ( -120.6228709571500417, -24.51163499207180507, 0.6490370598555501580 ) ) ;
#33949 = CARTESIAN_POINT ( 'NONE',  ( -34.55620429048339304, -24.65952944569303895, 1.056160979905690356 ) ) ;
#33950 = ORIENTED_EDGE ( 'NONE', *, *, #28553, .T. ) ;
#33951 = CARTESIAN_POINT ( 'NONE',  ( -10.82153711268468932, 17.32902648900640230, 11.49999999999998934 ) ) ;
#33952 = ORIENTED_EDGE ( 'NONE', *, *, #52185, .F. ) ;
#33953 = EDGE_LOOP ( 'NONE', ( #1365, #36873, #20619, #24295 ) ) ;
#33954 = CARTESIAN_POINT ( 'NONE',  ( 22.97298546869389568, 1.202750762487129199, 11.49999999999998934 ) ) ;
#33955 = CARTESIAN_POINT ( 'NONE',  ( -105.5228709571501042, -23.48783264082477018, -1.443836473390085917 ) ) ;
#33956 = ORIENTED_EDGE ( 'NONE', *, *, #12416, .F. ) ;
#33957 = DIRECTION ( 'NONE',  ( 0.000000000000000000, -0.9999999999976377785, -2.173523156925979128E-06 ) ) ;
#33958 = CARTESIAN_POINT ( 'NONE',  ( -77.92287095715008149, -23.47596703998600631, 11.44779298504227683 ) ) ;
#33959 = CARTESIAN_POINT ( 'NONE',  ( -122.6228709571500417, -24.66019654487199730, 8.947790411086121054 ) ) ;
#33960 = CARTESIAN_POINT ( 'NONE',  ( 6.660000000000001030, -2.890508098367099432, -0.2344417481469836528 ) ) ;
#33962 = ORIENTED_EDGE ( 'NONE', *, *, #57419, .F. ) ;
#33961 = CARTESIAN_POINT ( 'NONE',  ( -1.966620079519992181, -21.27258529651320274, 11.49999999999999645 ) ) ;
#33963 = ORIENTED_EDGE ( 'NONE', *, *, #91391, .F. ) ;
#33964 = CARTESIAN_POINT ( 'NONE',  ( -17.21897301287555848, -14.04741862099043104, 11.49999999999998934 ) ) ;
#33965 = CARTESIAN_POINT ( 'NONE',  ( -18.22997975830956108, -9.740667652671243459, -1.500000000000002220 ) ) ;
#33966 = AXIS2_PLACEMENT_3D ( 'NONE', #89179, #65867, #34895 ) ;
#33967 = VERTEX_POINT ( 'NONE', #86673 ) ;
#33968 = FACE_OUTER_BOUND ( 'NONE', #69316, .T. ) ;
#33969 = CARTESIAN_POINT ( 'NONE',  ( 9.383883476483161346, 17.86611652351680846, 2.100000000000000089 ) ) ;
#33970 = ORIENTED_EDGE ( 'NONE', *, *, #8029, .T. ) ;
#33971 = CARTESIAN_POINT ( 'NONE',  ( -0.3059464777392844059, -8.530684776139525027, -9.000000000000000000 ) ) ;
#33972 = AXIS2_PLACEMENT_3D ( 'NONE', #21093, #52061, #13481 ) ;
#33973 = ORIENTED_EDGE ( 'NONE', *, *, #9904, .T. ) ;
#33974 = CARTESIAN_POINT ( 'NONE',  ( -111.5122638532038053, -25.28710546256126435, 4.332404433089555695 ) ) ;
#33975 = CARTESIAN_POINT ( 'NONE',  ( -5.628781154649386664, 20.11113626451368219, -1.500000000000002220 ) ) ;
#33976 = EDGE_CURVE ( 'NONE', #100229, #61899, #34559, .T. ) ;
#33977 = B_SPLINE_CURVE_WITH_KNOTS ( 'NONE', 3,
 ( #98387, #29887, #97887, #5548 ),
 .UNSPECIFIED., .F., .F.,
 ( 4, 4 ),
 ( 0.000000000000000000, 1.000000000000000000 ),
 .UNSPECIFIED. ) ;
#33978 = CARTESIAN_POINT ( 'NONE',  ( 11.09338859787202480, -18.89396691112096605, 11.49999999999999645 ) ) ;
#33979 = DIRECTION ( 'NONE',  ( -1.000000000000000000, -4.986391167143583514E-16, 0.000000000000000000 ) ) ;
#33980 = PLANE ( 'NONE',  #66175 ) ;
#33981 = CARTESIAN_POINT ( 'NONE',  ( 12.95044643391442030, 18.39415735498938176, 11.49999999999998934 ) ) ;
#33982 = VECTOR ( 'NONE', #87026, 1000.000000000000114 ) ;
#33983 = CARTESIAN_POINT ( 'NONE',  ( 20.88312143257166653, -1.666129412636018214, 11.49999999999998934 ) ) ;
#33984 = CARTESIAN_POINT ( 'NONE',  ( -38.62894216554127524, -24.51314013834316086, 0.6176544820404135105 ) ) ;
#33985 = CARTESIAN_POINT ( 'NONE',  ( -15.82668884360736961, 6.475225279485576024, 42.07822029717483758 ) ) ;
#33986 = DIRECTION ( 'NONE',  ( -0.000000000000000000, -1.000000000000000000, -0.000000000000000000 ) ) ;
#33987 = ORIENTED_EDGE ( 'NONE', *, *, #29372, .T. ) ;
#33988 = AXIS2_PLACEMENT_3D ( 'NONE', #22445, #7231, #38178 ) ;
#33989 = B_SPLINE_CURVE_WITH_KNOTS ( 'NONE', 3,
 ( #51762, #35543, #66513, #27917 ),
 .UNSPECIFIED., .F., .F.,
 ( 4, 4 ),
 ( 0.000000000000000000, 1.000000000000000000 ),
 .UNSPECIFIED. ) ;
#33990 = EDGE_CURVE ( 'NONE', #51194, #22708, #45340, .T. ) ;
#33991 = ORIENTED_EDGE ( 'NONE', *, *, #58990, .F. ) ;
#33992 = VECTOR ( 'NONE', #9348, 1000.000000000000114 ) ;
#33993 = ORIENTED_EDGE ( 'NONE', *, *, #17925, .T. ) ;
#33994 = EDGE_CURVE ( 'NONE', #1891, #46085, #25924, .T. ) ;
#33995 = CARTESIAN_POINT ( 'NONE',  ( -52.53663968116620708, -24.51314013834315375, 0.6176544820404114011 ) ) ;
#33996 = ORIENTED_EDGE ( 'NONE', *, *, #76326, .T. ) ;
#33997 = AXIS2_PLACEMENT_3D ( 'NONE', #80795, #11275, #12260 ) ;
#33998 = CARTESIAN_POINT ( 'NONE',  ( -11.90495014755217618, 17.82271480561356469, -1.500000000000002220 ) ) ;
#33999 = ORIENTED_EDGE ( 'NONE', *, *, #80310, .F. ) ;
#34000 = CARTESIAN_POINT ( 'NONE',  ( 30.53060340732036337, -5.329285123471891872, 3.289350009555732868 ) ) ;
#34001 = CARTESIAN_POINT ( 'NONE',  ( 17.50165659415881336, 11.77592616506222711, -1.500000000000002220 ) ) ;
#34002 = CARTESIAN_POINT ( 'NONE',  ( -30.51821473474449675, -25.31108805091020741, 6.147639284700202822 ) ) ;
#34003 = CARTESIAN_POINT ( 'NONE',  ( 3.113719597313231002, -6.376774720514426065, 21.58936759753562029 ) ) ;
#34004 = CARTESIAN_POINT ( 'NONE',  ( -50.50115682139630735, -24.15602025860895097, 10.28564288303536856 ) ) ;
#34005 = CARTESIAN_POINT ( 'NONE',  ( -101.5869946791053025, -24.51314013834316086, 0.6176544820404198388 ) ) ;
#34006 = DIRECTION ( 'NONE',  ( -3.773278334444166432E-23, 1.000000000000000000, 0.000000000000000000 ) ) ;
#34007 = CARTESIAN_POINT ( 'NONE',  ( -16.14483305390557888, 14.99321182834783528, -1.500000000000002220 ) ) ;
#34008 = ORIENTED_EDGE ( 'NONE', *, *, #88791, .T. ) ;
#34009 = CARTESIAN_POINT ( 'NONE',  ( -116.5555276665938180, -23.96119346886881729, -0.6495511937831834892 ) ) ;
#34010 = ADVANCED_FACE ( 'NONE', ( #77547 ), #24277, .T. ) ;
#34011 = DIRECTION ( 'NONE',  ( 1.000000000000000000, 2.710505431213760099E-16, 0.000000000000000000 ) ) ;
#34012 = CARTESIAN_POINT ( 'NONE',  ( -41.14436886340001820, -25.27956039219115425, 5.395510761495216023 ) ) ;
#34013 = CARTESIAN_POINT ( 'NONE',  ( -26.94908181867664965, -25.04135458203152353, 6.075536601959949934 ) ) ;
#34014 = DIRECTION ( 'NONE',  ( 0.000000000000000000, -2.173523156925980399E-06, 0.9999999999976378895 ) ) ;
#34015 = PLANE ( 'NONE',  #83785 ) ;
#34016 = CARTESIAN_POINT ( 'NONE',  ( 2.936642053869352953, -21.15864249054145674, -1.500000000000002220 ) ) ;
#34017 = CARTESIAN_POINT ( 'NONE',  ( 4.967948717948723392, -5.876774720514415407, 20.00140224358974095 ) ) ;
#34018 = DIRECTION ( 'NONE',  ( 3.491481338843133355E-15, -1.000000000000000000, 2.352173255807804438E-16 ) ) ;
#34019 = CARTESIAN_POINT ( 'NONE',  ( -64.53585642586003246, -24.66019654487199730, 8.947790411086113949 ) ) ;
#34020 = CARTESIAN_POINT ( 'NONE',  ( -79.52287095715006160, -29.50250243563736774, 8.947779886222141599 ) ) ;
#34021 = CARTESIAN_POINT ( 'NONE',  ( 22.10748686624256720, -4.471405416651531795, -1.500000000000002220 ) ) ;
#34022 = CARTESIAN_POINT ( 'NONE',  ( 0.000000000000000000, 2.682774720514426559, 0.000000000000000000 ) ) ;
#34023 = ORIENTED_EDGE ( 'NONE', *, *, #76444, .F. ) ;
#34025 = CARTESIAN_POINT ( 'NONE',  ( 10.81255391457704640, 3.316774720514425123, -28.05044903510771803 ) ) ;
#34024 = B_SPLINE_CURVE_WITH_KNOTS ( 'NONE', 3,
 ( #63552, #50195, #94472, #19231 ),
 .UNSPECIFIED., .F., .F.,
 ( 4, 4 ),
 ( 0.5108647960461032422, 0.5198712273182189980 ),
 .UNSPECIFIED. ) ;
#34026 = CARTESIAN_POINT ( 'NONE',  ( -120.6228709571500417, -23.47596703998600631, 11.44779298504227683 ) ) ;
#34027 = CARTESIAN_POINT ( 'NONE',  ( -16.18664964019209052, -11.25563402961023662, 11.49999999999999645 ) ) ;
#34028 = PLANE ( 'NONE',  #87726 ) ;
#34029 = CARTESIAN_POINT ( 'NONE',  ( -8.160000000000000142, -10.15233964170348457, -1.303165529866009420 ) ) ;
#34030 = EDGE_CURVE ( 'NONE', #36077, #81218, #94784, .T. ) ;
#34031 = VERTEX_POINT ( 'NONE', #48635 ) ;
#34032 = B_SPLINE_CURVE_WITH_KNOTS ( 'NONE', 3,
 ( #15067, #60269, #46035, #54155, #76956, #85078, #91192, #23671, #77454, #16059 ),
 .UNSPECIFIED., .F., .F.,
 ( 4, 2, 2, 2, 4 ),
 ( 0.000000000000000000, 0.0007250860325595927204, 0.001087629048839393146, 0.001268900556979295907, 0.001450172065119198668 ),
 .UNSPECIFIED. ) ;
#34033 = LINE ( 'NONE', #35537, #5290 ) ;
#34034 = CARTESIAN_POINT ( 'NONE',  ( -10.54059822343757880, -6.376774720514426953, 22.82308057603841078 ) ) ;
#34035 = CARTESIAN_POINT ( 'NONE',  ( -105.5228709571501184, -24.63345952396258198, 9.038047939301510070 ) ) ;
#34036 = CARTESIAN_POINT ( 'NONE',  ( -20.54952838774410750, 6.582847151591199264, 11.49999999999998934 ) ) ;
#34037 = CARTESIAN_POINT ( 'NONE',  ( -90.92287095715005307, -23.47593901973090169, -1.443836447538996870 ) ) ;
#34038 = CARTESIAN_POINT ( 'NONE',  ( -76.58953762381673869, -24.66019654487198665, 8.947790411086133489 ) ) ;
#34039 = CARTESIAN_POINT ( 'NONE',  ( -13.89275734969026388, -0.3587747205144262708, 31.02402280011862246 ) ) ;
#34040 = CARTESIAN_POINT ( 'NONE',  ( -97.62287095715008434, -23.47596703998600631, 11.44779298504227860 ) ) ;
#34041 = CARTESIAN_POINT ( 'NONE',  ( -16.30015253881794379, -11.17962500214296639, 11.49999999999998934 ) ) ;
#34042 = EDGE_CURVE ( 'NONE', #90256, #62112, #41939, .T. ) ;
#34043 = ORIENTED_EDGE ( 'NONE', *, *, #34135, .F. ) ;
#34044 = CARTESIAN_POINT ( 'NONE',  ( 6.837353022973060135, 19.10023500134885310, 11.49999999999999645 ) ) ;
#34045 = FACE_OUTER_BOUND ( 'NONE', #99950, .T. ) ;
#34046 = VECTOR ( 'NONE', #90489, 1000.000000000000114 ) ;
#34047 = ADVANCED_FACE ( 'NONE', ( #54742 ), #10050, .T. ) ;
#34048 = ORIENTED_EDGE ( 'NONE', *, *, #96968, .F. ) ;
#34049 = CARTESIAN_POINT ( 'NONE',  ( 26.73860345374794889, 5.333846218197647815, -4.449799762242919954 ) ) ;
#34050 = DIRECTION ( 'NONE',  ( -1.334402673828313093E-16, 0.000000000000000000, -1.000000000000000000 ) ) ;
#34051 = CARTESIAN_POINT ( 'NONE',  ( -48.62287095715004881, -29.50248528299804818, 1.056150453629033370 ) ) ;
#34052 = DIRECTION ( 'NONE',  ( 0.6599726524652410609, 0.000000000000000000, -0.7512896232465839930 ) ) ;
#34053 = VECTOR ( 'NONE', #81382, 1000.000000000000000 ) ;
#34054 = CYLINDRICAL_SURFACE ( 'NONE', #97542, 0.2499999999997798983 ) ;
#34055 = PLANE ( 'NONE',  #2547 ) ;
#34056 = CARTESIAN_POINT ( 'NONE',  ( 18.34943919012036773, 8.063251210807163005, 11.49999999999998934 ) ) ;
#34057 = DIRECTION ( 'NONE',  ( 1.000000000000000000, 0.000000000000000000, 0.000000000000000000 ) ) ;
#34058 = EDGE_LOOP ( 'NONE', ( #58689, #75922, #47194, #97498 ) ) ;
#34059 = VECTOR ( 'NONE', #97770, 1000.000000000000114 ) ;
#34060 = VECTOR ( 'NONE', #32862, 1000.000000000000114 ) ;
#34061 = DIRECTION ( 'NONE',  ( -1.000000000000000000, 0.000000000000000000, -0.000000000000000000 ) ) ;
#34062 = CARTESIAN_POINT ( 'NONE',  ( -35.62380676451632411, -25.00158670708910336, 2.256160236439224143 ) ) ;
#34063 = CARTESIAN_POINT ( 'NONE',  ( -80.08697634283775812, -25.30560378225014873, 5.004156656408841997 ) ) ;
#34064 = VECTOR ( 'NONE', #62924, 1000.000000000000000 ) ;
#34065 = FACE_OUTER_BOUND ( 'NONE', #81626, .T. ) ;
#34066 = CARTESIAN_POINT ( 'NONE',  ( -73.60155033630429955, -23.73766607897670511, -1.055555164236457344 ) ) ;
#34067 = EDGE_CURVE ( 'NONE', #234, #39724, #85398, .T. ) ;
#34068 = CIRCLE ( 'NONE', #3306, 1.325999999999990298 ) ;
#34069 = CARTESIAN_POINT ( 'NONE',  ( 15.99960863614694873, 3.577630190449803571, -27.91116951066526397 ) ) ;
#34070 = VECTOR ( 'NONE', #64888, 1000.000000000000114 ) ;
#34071 = CARTESIAN_POINT ( 'NONE',  ( -98.87540794031171743, -25.20650842489795807, 6.812665538484692362 ) ) ;
#34072 = VERTEX_POINT ( 'NONE', #23769 ) ;
#34073 = EDGE_CURVE ( 'NONE', #94109, #40447, #2449, .T. ) ;
#34074 = CARTESIAN_POINT ( 'NONE',  ( -0.6891947355827284794, 20.32259304938107292, -1.500000000000002220 ) ) ;
#34075 = ORIENTED_EDGE ( 'NONE', *, *, #18704, .F. ) ;
#34076 = CARTESIAN_POINT ( 'NONE',  ( -32.53790792079495020, -24.34968618360933590, 0.1864209137778856384 ) ) ;
#34077 = CARTESIAN_POINT ( 'NONE',  ( -118.5228709571500758, -23.47596703998600631, 11.44779298504227860 ) ) ;
#34079 = ORIENTED_EDGE ( 'NONE', *, *, #36890, .F. ) ;
#34078 = EDGE_CURVE ( 'NONE', #9871, #79973, #64784, .T. ) ;
#34080 = CARTESIAN_POINT ( 'NONE',  ( -59.61137031377487006, -23.48786465467240703, 11.44779295918255180 ) ) ;
#34081 = EDGE_CURVE ( 'NONE', #17533, #96649, #64371, .T. ) ;
#34082 = CARTESIAN_POINT ( 'NONE',  ( -49.39546678031889826, -25.26264066864941782, 6.587942125045247899 ) ) ;
#34083 = CARTESIAN_POINT ( 'NONE',  ( -30.47287095715008576, -24.67388046057699924, 1.121487310756236200 ) ) ;
#34084 = CARTESIAN_POINT ( 'NONE',  ( 12.26186175617451113, -17.30295086655154080, 11.49999999999999645 ) ) ;
#34085 = EDGE_CURVE ( 'NONE', #2532, #80762, #62868, .T. ) ;
#34086 = CARTESIAN_POINT ( 'NONE',  ( -0.9539927174334467130, 22.11892580961223587, -1.500000000000002220 ) ) ;
#34087 = CARTESIAN_POINT ( 'NONE',  ( 20.45670835789597319, 2.398913822417158226, 11.49999999999998934 ) ) ;
#34088 = VERTEX_POINT ( 'NONE', #47628 ) ;
#34089 = CARTESIAN_POINT ( 'NONE',  ( -91.55620429048339304, -23.47596703998600631, 11.44779298504227683 ) ) ;
#34090 = VERTEX_POINT ( 'NONE', #94281 ) ;
#34091 = CARTESIAN_POINT ( 'NONE',  ( 7.136624701378261548, -6.376774720514420736, 20.99078681144753844 ) ) ;
#34092 = FACE_OUTER_BOUND ( 'NONE', #9462, .T. ) ;
#34093 = EDGE_LOOP ( 'NONE', ( #90581, #45811, #97977, #22940 ) ) ;
#34094 = VERTEX_POINT ( 'NONE', #55748 ) ;
#34095 = EDGE_LOOP ( 'NONE', ( #13888, #70181, #6903, #4236 ) ) ;
#34096 = FACE_BOUND ( 'NONE', #5524, .T. ) ;
#34098 = CARTESIAN_POINT ( 'NONE',  ( 6.910430652544937935, -6.376774720514418959, 20.24472806504191169 ) ) ;
#34097 = B_SPLINE_CURVE_WITH_KNOTS ( 'NONE', 3,
 ( #27717, #65801, #58175, #59169, #28715, #59676 ),
 .UNSPECIFIED., .F., .F.,
 ( 4, 2, 4 ),
 ( 1.570887131795109485E-05, 0.001396322306279764325, 0.002776935741241577573 ),
 .UNSPECIFIED. ) ;
#34099 = PLANE ( 'NONE',  #38977 ) ;
#34100 = CARTESIAN_POINT ( 'NONE',  ( -11.67826063220891086, 17.12864047899337550, -1.500000000000002220 ) ) ;
#34101 = EDGE_CURVE ( 'NONE', #13389, #99974, #57253, .T. ) ;
#34102 = CARTESIAN_POINT ( 'NONE',  ( -17.53059066697263546, 12.75712217820542627, 11.49999999999999645 ) ) ;
#34103 = ORIENTED_EDGE ( 'NONE', *, *, #13552, .F. ) ;
#34104 = CARTESIAN_POINT ( 'NONE',  ( 7.749999999999998224, 23.99999999999999289, 2.100000000000000089 ) ) ;
#34105 = CARTESIAN_POINT ( 'NONE',  ( -109.5228709571500616, -23.48786465467242479, 11.44779295918253936 ) ) ;
#34106 = CARTESIAN_POINT ( 'NONE',  ( 15.34105849444754455, 16.31744944422920440, 11.49999999999998934 ) ) ;
#34107 = CARTESIAN_POINT ( 'NONE',  ( -22.05275734969026047, 5.965225279485572685, 31.02402280011862246 ) ) ;
#34108 = CARTESIAN_POINT ( 'NONE',  ( -65.65276470879786075, -23.85016227208580730, -0.8807180028928343063 ) ) ;
#34109 = EDGE_LOOP ( 'NONE', ( #18890, #44846, #72926, #24213 ) ) ;
#34110 = CARTESIAN_POINT ( 'NONE',  ( 29.57907552799942508, 3.316774720514426456, 29.21818156447043791 ) ) ;
#34111 = CARTESIAN_POINT ( 'NONE',  ( -129.5562042904834072, -24.64898659630529920, 1.056161002820838579 ) ) ;
#34112 = ORIENTED_EDGE ( 'NONE', *, *, #5215, .F. ) ;
#34113 = ORIENTED_EDGE ( 'NONE', *, *, #85418, .T. ) ;
#34114 = CIRCLE ( 'NONE', #14686, 6.000000000000000888 ) ;
#34116 = EDGE_CURVE ( 'NONE', #69928, #98963, #65369, .T. ) ;
#34115 = CARTESIAN_POINT ( 'NONE',  ( -87.62287095715004170, -24.33832256526968862, 0.1851278514119903129 ) ) ;
#34117 = ORIENTED_EDGE ( 'NONE', *, *, #61709, .F. ) ;
#34118 = CARTESIAN_POINT ( 'NONE',  ( 9.480266252741309074, -18.97159823121752709, -1.500000000000002220 ) ) ;
#34119 = EDGE_CURVE ( 'NONE', #88641, #75066, #37062, .T. ) ;
#34120 = VERTEX_POINT ( 'NONE', #49135 ) ;
#34121 = CARTESIAN_POINT ( 'NONE',  ( -88.62863264088480264, -24.34968618360934656, 0.1864209137778829184 ) ) ;
#34122 = CARTESIAN_POINT ( 'NONE',  ( 9.711643268838683341, -19.58466107313252635, 11.49999999999998934 ) ) ;
#34123 = CARTESIAN_POINT ( 'NONE',  ( -52.59912202816710902, -23.96169478059712787, 10.65365249895718591 ) ) ;
#34124 = CARTESIAN_POINT ( 'NONE',  ( -41.35158263814751933, -25.28892524829919708, 3.766620786843653867 ) ) ;
#34125 = CARTESIAN_POINT ( 'NONE',  ( -49.52287095715006870, -24.35013146730202749, 9.818937971375111928 ) ) ;
#34126 = CARTESIAN_POINT ( 'NONE',  ( 1.740910633133015972, 21.82039641801506846, -1.500000000000002220 ) ) ;
#34127 = CARTESIAN_POINT ( 'NONE',  ( -109.5228709571500616, -23.48786465467242479, 11.44779295918253936 ) ) ;
#34128 = VERTEX_POINT ( 'NONE', #89675 ) ;
#34129 = CARTESIAN_POINT ( 'NONE',  ( 25.10471210317054513, 4.943531924819384749, -10.06527829753310499 ) ) ;
#34130 = CARTESIAN_POINT ( 'NONE',  ( -49.18705952543585624, -25.26337497496688300, 7.035471253413802195 ) ) ;
#34131 = EDGE_CURVE ( 'NONE', #42735, #86336, #96292, .T. ) ;
#34132 = EDGE_CURVE ( 'NONE', #42079, #23355, #32371, .T. ) ;
#34133 = ORIENTED_EDGE ( 'NONE', *, *, #7869, .F. ) ;
#34134 = DIRECTION ( 'NONE',  ( 0.000000000000000000, 0.000000000000000000, -1.000000000000000000 ) ) ;
#34135 = EDGE_CURVE ( 'NONE', #78378, #51347, #58238, .T. ) ;
#34136 = VECTOR ( 'NONE', #68089, 1000.000000000000000 ) ;
#34137 = ORIENTED_EDGE ( 'NONE', *, *, #17143, .F. ) ;
#34138 = DIRECTION ( 'NONE',  ( 0.1254312216594016816, 0.000000000000000000, 0.9921023176230514551 ) ) ;
#34139 = VECTOR ( 'NONE', #30470, 1000.000000000000114 ) ;
#34140 = CARTESIAN_POINT ( 'NONE',  ( -31.24388727629348494, -25.27868065289452559, 3.907572214828554991 ) ) ;
#34141 = CARTESIAN_POINT ( 'NONE',  ( -10.85727797829764185, 18.24708236899833835, -1.500000000000002220 ) ) ;
#34142 = CARTESIAN_POINT ( 'NONE',  ( -29.49875734969025842, -0.3587747205144265483, 25.61802280011862720 ) ) ;
#34143 = CARTESIAN_POINT ( 'NONE',  ( -102.6228709571500559, -23.47593901973091235, -1.443836447539001089 ) ) ;
#34144 = B_SPLINE_CURVE_WITH_KNOTS ( 'NONE', 3,
 ( #94660, #18037, #71335, #57619, #1824, #95166 ),
 .UNSPECIFIED., .F., .F.,
 ( 4, 2, 4 ),
 ( 6.384118694778946581E-06, 0.001386860460836456194, 0.002767336802978133219 ),
 .UNSPECIFIED. ) ;
#34145 = CARTESIAN_POINT ( 'NONE',  ( 14.76093561896379214, -6.475225279485573360, -26.55548769130089681 ) ) ;
#34146 = CARTESIAN_POINT ( 'NONE',  ( -129.5228709571501042, -24.51283580621366553, 0.6167428607019809217 ) ) ;
#34147 = AXIS2_PLACEMENT_3D ( 'NONE', #25278, #47132, #62356 ) ;
#34148 = CARTESIAN_POINT ( 'NONE',  ( 6.036767712469883307, 18.47306877840545170, -1.500000000000002220 ) ) ;
#34149 = CARTESIAN_POINT ( 'NONE',  ( -45.52251770710876855, -25.00158670708910336, 2.256160236439225031 ) ) ;
#34150 = ORIENTED_EDGE ( 'NONE', *, *, #90901, .F. ) ;
#34151 = CARTESIAN_POINT ( 'NONE',  ( 17.47348308817029405, 8.859467055162037141, 11.49999999999999645 ) ) ;
#34152 = CARTESIAN_POINT ( 'NONE',  ( -5.568927889719891944, -6.376774720514417183, 20.14881673916291760 ) ) ;
#34153 = DIRECTION ( 'NONE',  ( 0.000000000000000000, -0.9999999999976377785, -2.173523156925979975E-06 ) ) ;
#34154 = VERTEX_POINT ( 'NONE', #18655 ) ;
#34155 = CARTESIAN_POINT ( 'NONE',  ( -97.62287095715008434, -23.94994826722515668, -0.6494450866351703100 ) ) ;
#34156 = CARTESIAN_POINT ( 'NONE',  ( -89.55152734856552854, -24.15543982623907837, -0.2315651400026483009 ) ) ;
#34157 = CARTESIAN_POINT ( 'NONE',  ( 16.15056352287345121, -3.622774720514426949, -27.77856273171767398 ) ) ;
#34158 = CARTESIAN_POINT ( 'NONE',  ( -80.64549629918748508, -25.03156060304832664, 7.560538530590703132 ) ) ;
#34159 = CARTESIAN_POINT ( 'NONE',  ( 19.63295818312489871, -1.572306604260808260, 11.49999999999998934 ) ) ;
#34160 = EDGE_LOOP ( 'NONE', ( #27545, #12464, #80556, #76669 ) ) ;
#34161 = CARTESIAN_POINT ( 'NONE',  ( -121.6228709571500417, -24.64898659630368627, 1.056161002820833028 ) ) ;
#34162 = PLANE ( 'NONE',  #80355 ) ;
#34163 = MECHANICAL_CONTEXT ( 'NONE', #4487, 'mechanical' ) ;
#34164 = ORIENTED_EDGE ( 'NONE', *, *, #3725, .T. ) ;
#34165 = CARTESIAN_POINT ( 'NONE',  ( -125.5228709571500048, -24.83620972994592435, 8.398175272781372769 ) ) ;
#34166 = CARTESIAN_POINT ( 'NONE',  ( -1.649669150391666506, -6.376774720514411854, 19.67464842890028365 ) ) ;
#34167 = CARTESIAN_POINT ( 'NONE',  ( -108.9623037622677941, -25.26366506051257588, 3.989953612098970481 ) ) ;
#34168 = CARTESIAN_POINT ( 'NONE',  ( -76.52287095715007581, -24.65952944569304606, 1.056160979905698794 ) ) ;
#34169 = CARTESIAN_POINT ( 'NONE',  ( -119.5228709571500758, -24.64898659630368627, 1.056161002820833028 ) ) ;
#34170 = CARTESIAN_POINT ( 'NONE',  ( -69.51029376924685721, -25.31201676907213027, 5.710789725594461075 ) ) ;
#34171 = PLANE ( 'NONE',  #91542 ) ;
#34172 = CARTESIAN_POINT ( 'NONE',  ( 18.23660095519748481, -8.086948576924280374, 11.49999999999998934 ) ) ;
#34173 = CARTESIAN_POINT ( 'NONE',  ( -100.6945227148491426, -25.19910511675319853, 3.322861593611079467 ) ) ;
#34174 = CARTESIAN_POINT ( 'NONE',  ( -19.77004505525285083, 2.005399880840008642, -1.500000000000002220 ) ) ;
#34175 = VERTEX_POINT ( 'NONE', #88683 ) ;
#34176 = CARTESIAN_POINT ( 'NONE',  ( -84.62287095715005592, -29.50250786944525672, 11.44777988621623521 ) ) ;
#34177 = B_SPLINE_CURVE_WITH_KNOTS ( 'NONE', 3,
 ( #62194, #68799, #30221, #70798 ),
 .UNSPECIFIED., .F., .F.,
 ( 4, 4 ),
 ( 0.1105789617298616606, 0.1195853930019770833 ),
 .UNSPECIFIED. ) ;
#34178 = CARTESIAN_POINT ( 'NONE',  ( -51.22247509701755774, -25.17612187086679043, 6.839882705316316702 ) ) ;
#34179 = CARTESIAN_POINT ( 'NONE',  ( -6.741682653110981249, -5.965225279485572685, 30.62569541381301619 ) ) ;
#34180 = CARTESIAN_POINT ( 'NONE',  ( -80.49409576116666187, -24.92592662359561118, 8.075495903017996469 ) ) ;
#34181 = CARTESIAN_POINT ( 'NONE',  ( 19.72710162658169608, 6.580912942549038469, 11.49999999999999645 ) ) ;
#34182 = FACE_OUTER_BOUND ( 'NONE', #23848, .T. ) ;
#34183 = AXIS2_PLACEMENT_3D ( 'NONE', #9382, #32216, #77880 ) ;
#34184 = FACE_OUTER_BOUND ( 'NONE', #23612, .T. ) ;
#34185 = CARTESIAN_POINT ( 'NONE',  ( 22.22072617242880455, -5.352622178732230118, 11.49999999999999645 ) ) ;
#34187 = EDGE_CURVE ( 'NONE', #18921, #52201, #71263, .T. ) ;
#34186 = EDGE_LOOP ( 'NONE', ( #90865, #32373, #54796, #3096 ) ) ;
#34188 = CARTESIAN_POINT ( 'NONE',  ( -74.62287095715005592, -29.50247984919015209, -1.443849546365055359 ) ) ;
#34189 = CARTESIAN_POINT ( 'NONE',  ( -50.40445135320379677, -29.50249842297920466, 7.101626040072651413 ) ) ;
#34190 = VERTEX_POINT ( 'NONE', #19650 ) ;
#34191 = CARTESIAN_POINT ( 'NONE',  ( 19.26017855675105750, 6.235128648364509196, -1.500000000000002220 ) ) ;
#34192 = CARTESIAN_POINT ( 'NONE',  ( -90.52287095715006160, -23.47596703998600631, 11.44779298504228393 ) ) ;
#34193 = CARTESIAN_POINT ( 'NONE',  ( -129.6228709571500701, -24.50216790748205398, 0.6166512839542656055 ) ) ;
#34194 = EDGE_CURVE ( 'NONE', #61919, #19444, #89089, .T. ) ;
#34195 = EDGE_CURVE ( 'NONE', #37098, #29344, #51116, .T. ) ;
#34196 = CARTESIAN_POINT ( 'NONE',  ( -84.52287095715006160, -24.64898659630528854, 1.056161002820826145 ) ) ;
#34197 = EDGE_CURVE ( 'NONE', #17879, #33339, #63694, .T. ) ;
#34198 = ORIENTED_EDGE ( 'NONE', *, *, #100288, .T. ) ;
#34199 = CARTESIAN_POINT ( 'NONE',  ( -24.90875734969025501, 5.965225279485572685, 26.43402280011862615 ) ) ;
#34200 = CARTESIAN_POINT ( 'NONE',  ( -77.52287095715010423, -23.47593901973090524, -1.443836447538997092 ) ) ;
#34201 = VECTOR ( 'NONE', #17548, 1000.000000000000000 ) ;
#34202 = CARTESIAN_POINT ( 'NONE',  ( 15.90762396150235958, 12.10710967819287198, -1.500000000000002220 ) ) ;
#34203 = CARTESIAN_POINT ( 'NONE',  ( 20.69369447470243628, -3.267675865747468489, 11.49999999999999645 ) ) ;
#34205 = EDGE_CURVE ( 'NONE', #87248, #15603, #40673, .T. ) ;
#34204 = APPROVAL_PERSON_ORGANIZATION ( #39388, #65024, #54622 ) ;
#34206 = CARTESIAN_POINT ( 'NONE',  ( -25.92875734969026524, -6.376774720514426953, -0.08597719988137648983 ) ) ;
#34207 = DIRECTION ( 'NONE',  ( 0.000000000000000000, -1.000000000000000000, 0.000000000000000000 ) ) ;
#34208 = CARTESIAN_POINT ( 'NONE',  ( 2.156995527713877259, 21.93451973775924557, 11.49999999999998934 ) ) ;
#34209 = CARTESIAN_POINT ( 'NONE',  ( -39.71177198204633640, -25.31589273396069473, 4.822383007266354049 ) ) ;
#34210 = VERTEX_POINT ( 'NONE', #27774 ) ;
#34211 = CARTESIAN_POINT ( 'NONE',  ( -60.52287095715007581, -24.91544648472619983, 1.928969306349231250 ) ) ;
#34212 = CARTESIAN_POINT ( 'NONE',  ( -117.5228709571500758, -23.47593901973090524, -1.443836447538996204 ) ) ;
#34213 = CARTESIAN_POINT ( 'NONE',  ( -72.59671298878585333, -23.96119346886880663, -0.6495511937832119109 ) ) ;
#34214 = DIRECTION ( 'NONE',  ( -3.773278334453079618E-23, 0.9999999999976377785, 2.173523156925979975E-06 ) ) ;
#34215 = ORIENTED_EDGE ( 'NONE', *, *, #83630, .F. ) ;
#34216 = ORIENTED_EDGE ( 'NONE', *, *, #32383, .F. ) ;
#34217 = DIRECTION ( 'NONE',  ( 0.000000000000000000, 0.000000000000000000, -1.000000000000000000 ) ) ;
#34218 = CARTESIAN_POINT ( 'NONE',  ( -36.52287095715006870, -29.50250243563736774, 8.947779886222148704 ) ) ;
#34219 = CARTESIAN_POINT ( 'NONE',  ( -129.5228709571500758, -23.48786465467242479, 11.44779295918253581 ) ) ;
#34220 = CARTESIAN_POINT ( 'NONE',  ( 10.70087849588422380, -17.49211976490306597, -1.500000000000002220 ) ) ;
#34221 = ADVANCED_FACE ( 'NONE', ( #49630 ), #12543, .F. ) ;
#34222 = ORIENTED_EDGE ( 'NONE', *, *, #72614, .T. ) ;
#34223 = CARTESIAN_POINT ( 'NONE',  ( -39.52287095715006870, -24.65952944569304606, 1.056160979905691910 ) ) ;
#34224 = FACE_BOUND ( 'NONE', #62336, .T. ) ;
#34225 = CARTESIAN_POINT ( 'NONE',  ( -41.52287095715009002, -24.33927499327854349, 9.819080762295811837 ) ) ;
#34226 = CARTESIAN_POINT ( 'NONE',  ( 21.15698459081360383, -7.064864530413820454, -1.500000000000002220 ) ) ;
#34227 = CARTESIAN_POINT ( 'NONE',  ( -0.1051616404667204685, -21.68859992388200908, -0.4716817114508830566 ) ) ;
#34228 = LINE ( 'NONE', #10378, #95132 ) ;
#34229 = EDGE_CURVE ( 'NONE', #56711, #11930, #73196, .T. ) ;
#34230 = ORIENTED_EDGE ( 'NONE', *, *, #36774, .F. ) ;
#34231 = CARTESIAN_POINT ( 'NONE',  ( -42.62287095715004170, -23.94994826722515313, -0.6494450866351717533 ) ) ;
#34232 = CARTESIAN_POINT ( 'NONE',  ( -51.68090471422387111, -25.27854796960392036, 4.190565742094029211 ) ) ;
#34233 = CARTESIAN_POINT ( 'NONE',  ( -19.30504728598367237, -7.930543132070424051, -1.500000000000002220 ) ) ;
#34234 = VERTEX_POINT ( 'NONE', #18165 ) ;
#34237 = ORIENTED_EDGE ( 'NONE', *, *, #15401, .T. ) ;
#34236 = EDGE_CURVE ( 'NONE', #87928, #82230, #51862, .T. ) ;
#34235 = CARTESIAN_POINT ( 'NONE',  ( -39.04646076302208257, -25.27410141243213459, 4.123264079031926599 ) ) ;
#34238 = VERTEX_POINT ( 'NONE', #2956 ) ;
#34239 = CARTESIAN_POINT ( 'NONE',  ( -33.58953762381672448, -23.47593901973091235, -1.443836447539013301 ) ) ;
#34240 = CARTESIAN_POINT ( 'NONE',  ( 18.71565868802652588, -9.641079743366450572, -1.500000000000002220 ) ) ;
#34241 = EDGE_LOOP ( 'NONE', ( #11415, #51178, #65584 ) ) ;
#34242 = CARTESIAN_POINT ( 'NONE',  ( -37.52287095715006870, -23.47596703998600631, 11.44779298504229281 ) ) ;
#34243 = LINE ( 'NONE', #24608, #93549 ) ;
#34244 = CARTESIAN_POINT ( 'NONE',  ( -105.5895376238167103, -25.00182538069145721, 7.747789668545099317 ) ) ;
#34245 = CARTESIAN_POINT ( 'NONE',  ( -101.5316874056614012, -25.25419461862107795, 7.138212572458112248 ) ) ;
#34246 = CARTESIAN_POINT ( 'NONE',  ( -84.52287095715006160, -23.47593901973090524, -1.443836447538996648 ) ) ;
#34247 = CARTESIAN_POINT ( 'NONE',  ( 16.47784684176308545, -14.13017478139203220, -1.500000000000002220 ) ) ;
#34248 = CARTESIAN_POINT ( 'NONE',  ( -81.29833273411215089, -25.12224311376198926, 6.730504961598555269 ) ) ;
#34250 = ORIENTED_EDGE ( 'NONE', *, *, #36952, .T. ) ;
#34249 = CARTESIAN_POINT ( 'NONE',  ( 14.63995501510512653, -16.76770752772931772, 11.49999999999999645 ) ) ;
#34251 = CARTESIAN_POINT ( 'NONE',  ( -51.52764846858840997, -25.24728938674537559, 6.187572788865870699 ) ) ;
#34252 = FACE_OUTER_BOUND ( 'NONE', #67816, .T. ) ;
#34253 = CARTESIAN_POINT ( 'NONE',  ( -69.58953762381672448, -23.48786465467241058, 11.44779295918254824 ) ) ;
#34255 = ORIENTED_EDGE ( 'NONE', *, *, #71475, .F. ) ;
#34254 = EDGE_CURVE ( 'NONE', #27148, #5489, #64874, .T. ) ;
#34256 = ADVANCED_FACE ( 'NONE', ( #72963 ), #3457, .F. ) ;
#34258 = ORIENTED_EDGE ( 'NONE', *, *, #75795, .F. ) ;
#34257 = CYLINDRICAL_SURFACE ( 'NONE', #13479, 2.000000000000000888 ) ;
#34259 = ORIENTED_EDGE ( 'NONE', *, *, #173, .F. ) ;
#34260 = B_SPLINE_CURVE_WITH_KNOTS ( 'NONE', 3,
 ( #58065, #89491, #88999, #20464 ),
 .UNSPECIFIED., .F., .F.,
 ( 4, 4 ),
 ( 0.000000000000000000, 9.999999999998897304E-05 ),
 .UNSPECIFIED. ) ;
#34261 = DIRECTION ( 'NONE',  ( 0.1827036106964188555, 0.000000000000000000, -0.9831680378442393398 ) ) ;
#34263 = EDGE_CURVE ( 'NONE', #3153, #78991, #15003, .T. ) ;
#34262 = AXIS2_PLACEMENT_3D ( 'NONE', #80319, #10308, #33142 ) ;
#34264 = PLANE ( 'NONE',  #66444 ) ;
#34265 = FACE_OUTER_BOUND ( 'NONE', #89920, .T. ) ;
#34266 = ORIENTED_EDGE ( 'NONE', *, *, #35767, .T. ) ;
#34267 = APPLICATION_CONTEXT ( 'configuration controlled 3d designs of mechanical parts and assemblies' ) ;
#34269 =( BOUNDED_SURFACE ( )  B_SPLINE_SURFACE ( 3, 1, ( 
 ( #86977, #77355 ),
 ( #2262, #63164 ),
 ( #31699, #9857 ),
 ( #69768, #16458 ) ),
 .UNSPECIFIED., .F., .F., .T. ) 
 B_SPLINE_SURFACE_WITH_KNOTS ( ( 4, 4 ),
 ( 2, 2 ),
 ( 0.000000000000000000, 1.000000000000000000 ),
 ( 0.000000000000000000, 1.000000000000000000 ),
 .UNSPECIFIED. ) 
 GEOMETRIC_REPRESENTATION_ITEM ( )  RATIONAL_B_SPLINE_SURFACE ( (
 ( 1.000000000000000000, 1.000000000000000000),
 ( 0.3333333333333321491, 0.3333333333333321491),
 ( 0.3333333333333321491, 0.3333333333333321491),
 ( 1.000000000000000000, 1.000000000000000000) ) ) 
 REPRESENTATION_ITEM ( '' )  SURFACE ( )  );
#34268 = CARTESIAN_POINT ( 'NONE',  ( -130.5728709571500588, -23.56000036390797092, -1.497999999999531040 ) ) ;
#34270 = CARTESIAN_POINT ( 'NONE',  ( 11.54466316424315231, -19.26756404802103972, -1.500000000000002220 ) ) ;
#34271 = ORIENTED_EDGE ( 'NONE', *, *, #29950, .T. ) ;
#34272 = CARTESIAN_POINT ( 'NONE',  ( -112.5188917146773093, -23.96169478059713498, 10.65365249895717170 ) ) ;
#34273 = CARTESIAN_POINT ( 'NONE',  ( -88.52287095715006160, -29.50250786944525672, 11.44777988621623344 ) ) ;
#34274 = CARTESIAN_POINT ( 'NONE',  ( 2.591645189881369493, -5.876774720514412742, 19.84288601127407148 ) ) ;
#34275 = CARTESIAN_POINT ( 'NONE',  ( -49.22287095715007865, -23.47593901973090169, -1.443836447538997980 ) ) ;
#34276 = CARTESIAN_POINT ( 'NONE',  ( -30.57310316700385400, -25.30558673197060671, 5.002395802403323266 ) ) ;
#34277 = VECTOR ( 'NONE', #50755, 1000.000000000000000 ) ;
#34278 = CARTESIAN_POINT ( 'NONE',  ( 12.01011565470214393, -15.49198969801113890, 11.49999999999998934 ) ) ;
#34279 = DIRECTION ( 'NONE',  ( 0.000000000000000000, 0.000000000000000000, 1.000000000000000000 ) ) ;
#34281 = ORIENTED_EDGE ( 'NONE', *, *, #68203, .T. ) ;
#34280 = LOCAL_TIME ( 0, 54, 15.00000000000000000, #70342 ) ;
#34282 = CARTESIAN_POINT ( 'NONE',  ( -14.35963886870962192, 16.04489112172382903, 11.49999999999998934 ) ) ;
#34283 = DIRECTION ( 'NONE',  ( 1.000000000000000000, 0.000000000000000000, 0.000000000000000000 ) ) ;
#34284 = CARTESIAN_POINT ( 'NONE',  ( -80.64958649024407578, -25.30394762175274437, 4.980655888648957585 ) ) ;
#34285 = LINE ( 'NONE', #2337, #23096 ) ;
#34286 = CARTESIAN_POINT ( 'NONE',  ( -72.62287095715005592, -23.48783264082478084, -1.443836473390067265 ) ) ;
#34287 = CARTESIAN_POINT ( 'NONE',  ( -21.13427563780003382, 8.902639844219676135, -1.500000000000002220 ) ) ;
#34288 = APPROVAL_ROLE ( '' ) ;
#34289 = CARTESIAN_POINT ( 'NONE',  ( -93.62287095715002749, -24.51283580621365132, 0.6167428607019797004 ) ) ;
#34290 = CARTESIAN_POINT ( 'NONE',  ( -49.50098155592819893, -24.15543982623906771, -0.2315651400026657036 ) ) ;
#34291 = CARTESIAN_POINT ( 'NONE',  ( -7.287290609967129740, 18.71191762695291771, 11.49999999999999645 ) ) ;
#34292 = FACE_OUTER_BOUND ( 'NONE', #89425, .T. ) ;
#34293 = DIRECTION ( 'NONE',  ( -0.000000000000000000, 1.000000000000000000, -0.000000000000000000 ) ) ;
#34294 = CARTESIAN_POINT ( 'NONE',  ( -89.62287095715004170, -29.50250786944525672, 11.44777988621623344 ) ) ;
#34295 = CARTESIAN_POINT ( 'NONE',  ( -24.90875734969025501, 5.965225279485572685, 30.51402280011862089 ) ) ;
#34296 = CARTESIAN_POINT ( 'NONE',  ( -10.34999999999999254, 3.499999999999996003, 0.000000000000000000 ) ) ;
#34297 = CARTESIAN_POINT ( 'NONE',  ( -7.754168067426306266, 18.25094163199162622, 11.49999999999998934 ) ) ;
#34298 = DIRECTION ( 'NONE',  ( 0.000000000000000000, 1.000000000000000000, -0.000000000000000000 ) ) ;
#34299 = CARTESIAN_POINT ( 'NONE',  ( -2.355416116969162754, -19.56741566493107598, -1.500000000000002220 ) ) ;
#34300 = DIRECTION ( 'NONE',  ( 2.417950247244706201E-16, 0.000000000000000000, -1.000000000000000000 ) ) ;
#34301 = APPROVAL_DATE_TIME ( #3368, #61786 ) ;
#34302 = PLANE ( 'NONE',  #80777 ) ;
#34303 = CARTESIAN_POINT ( 'NONE',  ( 2.968164339864655332, -6.376774720514408301, 19.33154224050496595 ) ) ;
#34304 = CARTESIAN_POINT ( 'NONE',  ( 9.149160795417088821, -18.46424698110740437, 11.49999999999999645 ) ) ;
#34305 = DIRECTION ( 'NONE',  ( 0.000000000000000000, 0.000000000000000000, 1.000000000000000000 ) ) ;
#34306 = CARTESIAN_POINT ( 'NONE',  ( -22.58250372949163420, -2.080990182559540269, 11.49999999999999645 ) ) ;
#34307 = VECTOR ( 'NONE', #76282, 1000.000000000000000 ) ;
#34308 = ORIENTED_EDGE ( 'NONE', *, *, #60434, .F. ) ;
#34309 = CARTESIAN_POINT ( 'NONE',  ( -69.50411869601543913, -25.25639515137636337, 6.704350647680200836 ) ) ;
#34311 = EDGE_CURVE ( 'NONE', #88227, #3088, #94930, .T. ) ;
#34310 = CARTESIAN_POINT ( 'NONE',  ( -50.90364520198352238, -25.30916279181417394, 4.601666023064476363 ) ) ;
#34312 = EDGE_CURVE ( 'NONE', #34878, #64230, #53456, .T. ) ;
#34313 = CARTESIAN_POINT ( 'NONE',  ( -26.72222193076970953, -24.61460054499585226, 7.978875576793555524 ) ) ;
#34314 = ADVANCED_FACE ( 'NONE', ( #65238 ), #42393, .T. ) ;
#34315 = CARTESIAN_POINT ( 'NONE',  ( -2.283364382221138467, -6.376774720514411854, 19.46427715384223944 ) ) ;
#34316 = EDGE_CURVE ( 'NONE', #3681, #77123, #61160, .T. ) ;
#34317 = ORIENTED_EDGE ( 'NONE', *, *, #93177, .T. ) ;
#34318 = CARTESIAN_POINT ( 'NONE',  ( -99.56054792670708764, -25.17640016615229470, 6.770854614618325051 ) ) ;
#34319 = CARTESIAN_POINT ( 'NONE',  ( 13.94817355369617751, 18.09530419158152625, 11.49999999999998934 ) ) ;
#34320 = CARTESIAN_POINT ( 'NONE',  ( -98.62287095715005592, -24.64965695001469115, 8.947790433994178727 ) ) ;
#34321 = CARTESIAN_POINT ( 'NONE',  ( -113.5508033655503510, -24.66019654487200086, 8.947790411086106843 ) ) ;
#34322 = CARTESIAN_POINT ( 'NONE',  ( -82.50021946911930115, -24.66019654487199730, 8.947790411086122830 ) ) ;
#34323 = CARTESIAN_POINT ( 'NONE',  ( -22.33494257564923302, 2.542849975942539587, 11.49999999999999645 ) ) ;
#34324 = ORIENTED_EDGE ( 'NONE', *, *, #6477, .F. ) ;
#34325 = FACE_OUTER_BOUND ( 'NONE', #81410, .T. ) ;
#34326 = VECTOR ( 'NONE', #48527, 1000.000000000000114 ) ;
#34327 = CARTESIAN_POINT ( 'NONE',  ( 16.22650188657148362, -14.79325693486936188, 11.49999999999998934 ) ) ;
#34328 = CARTESIAN_POINT ( 'NONE',  ( -125.2170317540820861, -25.33540041250694230, 3.690481496468096090 ) ) ;
#34329 = B_SPLINE_CURVE_WITH_KNOTS ( 'NONE', 3,
 ( #50700, #4532, #13118, #58812, #42103, #51200 ),
 .UNSPECIFIED., .F., .F.,
 ( 4, 2, 4 ),
 ( 6.384118695309162101E-06, 0.001386860460836723992, 0.002767336802978138856 ),
 .UNSPECIFIED. ) ;
#34330 = CARTESIAN_POINT ( 'NONE',  ( -44.55312310627501660, -23.96169478059713143, 10.65365249895718414 ) ) ;
#34331 = CARTESIAN_POINT ( 'NONE',  ( -118.6228709571500701, -23.48783264082478794, -1.443836473390058384 ) ) ;
#34332 = VERTEX_POINT ( 'NONE', #19519 ) ;
#34333 = EDGE_CURVE ( 'NONE', #65938, #45794, #46600, .T. ) ;
#34334 = DIRECTION ( 'NONE',  ( 0.000000000000000000, 0.000000000000000000, -1.000000000000000000 ) ) ;
#34335 = DIRECTION ( 'NONE',  ( -3.773278334444167608E-23, 1.000000000000000000, 0.000000000000000000 ) ) ;
#34336 = VERTEX_POINT ( 'NONE', #28146 ) ;
#34337 = CARTESIAN_POINT ( 'NONE',  ( -88.52287095715006160, -23.94994826722564696, -0.6494450866342719175 ) ) ;
#34338 = CARTESIAN_POINT ( 'NONE',  ( 6.429960413904108663, -19.47341730443774921, 11.49999999999998934 ) ) ;
#34339 = EDGE_LOOP ( 'NONE', ( #97898, #91225, #93829, #51063, #44953, #67946, #80666, #90547, #40071, #45959, #80166, #10242 ) ) ;
#34340 = ORIENTED_EDGE ( 'NONE', *, *, #75672, .T. ) ;
#34341 = ORIENTED_EDGE ( 'NONE', *, *, #51669, .T. ) ;
#34342 = CARTESIAN_POINT ( 'NONE',  ( -0.02075734969026423599, -6.376774720514426953, -0.08597719988137648983 ) ) ;
#34343 = CARTESIAN_POINT ( 'NONE',  ( 21.75596283627254479, -7.788036635067100200, -1.500000000000002220 ) ) ;
#34344 = DIRECTION ( 'NONE',  ( -3.773278334453079030E-23, 0.9999999999976377785, 2.173523156925979128E-06 ) ) ;
#34345 = CARTESIAN_POINT ( 'NONE',  ( 20.27773211485958527, -1.686570798567030183, -1.500000000000002220 ) ) ;
#34346 = ORIENTED_EDGE ( 'NONE', *, *, #76721, .T. ) ;
#34347 = CARTESIAN_POINT ( 'NONE',  ( -1.675486951385420475, 10.82748519320431591, 3.549999999999999822 ) ) ;
#34348 = CARTESIAN_POINT ( 'NONE',  ( -29.61081068843649433, -23.65861429716871100, 11.05961561336856569 ) ) ;
#34350 = CARTESIAN_POINT ( 'NONE',  ( -105.5468799023555562, -24.92564183028979130, 1.928384488918251316 ) ) ;
#34349 = VECTOR ( 'NONE', #79590, 1000.000000000000000 ) ;
#34351 = FACE_OUTER_BOUND ( 'NONE', #86123, .T. ) ;
#34352 = EDGE_LOOP ( 'NONE', ( #53683, #21337, #6370, #91622 ) ) ;
#34353 = LINE ( 'NONE', #79517, #63034 ) ;
#34354 = FACE_OUTER_BOUND ( 'NONE', #43050, .T. ) ;
#34355 = APPROVAL_PERSON_ORGANIZATION ( #72727, #53771, #94047 ) ;
#34356 = ORIENTED_EDGE ( 'NONE', *, *, #82673, .T. ) ;
#34357 = CARTESIAN_POINT ( 'NONE',  ( 0.4431998670617953717, 20.78131286043265646, -1.500000000000002220 ) ) ;
#34358 = ORIENTED_EDGE ( 'NONE', *, *, #93985, .F. ) ;
#34360 = ORIENTED_EDGE ( 'NONE', *, *, #72627, .T. ) ;
#34359 = CARTESIAN_POINT ( 'NONE',  ( -39.44891728460616775, -25.28243733276015348, 4.250048832811843091 ) ) ;
#34361 = DIRECTION ( 'NONE',  ( -0.000000000000000000, 1.000000000000000000, -0.000000000000000000 ) ) ;
#34362 = DIRECTION ( 'NONE',  ( -3.773278334453079030E-23, 0.9999999999976377785, 2.173523156925978705E-06 ) ) ;
#34363 = ORIENTED_EDGE ( 'NONE', *, *, #58309, .T. ) ;
#34364 = ORIENTED_EDGE ( 'NONE', *, *, #53937, .F. ) ;
#34365 = CARTESIAN_POINT ( 'NONE',  ( -29.62287095715004881, -24.57333416927490433, 1.056161302446588124 ) ) ;
#34366 = SPHERICAL_SURFACE ( 'NONE', #9215, 1.000000000000000000 ) ;
#34367 = CARTESIAN_POINT ( 'NONE',  ( -70.97512524164069703, -25.24515085444608431, 5.512439509005878868 ) ) ;
#34369 = ORIENTED_EDGE ( 'NONE', *, *, #58997, .T. ) ;
#34368 = CARTESIAN_POINT ( 'NONE',  ( -19.90388773112789167, 9.559999800501117306, 11.49999999999999645 ) ) ;
#34370 = CARTESIAN_POINT ( 'NONE',  ( -47.62287095715004881, -23.48786465467240703, 11.44779295918255180 ) ) ;
#34371 = CARTESIAN_POINT ( 'NONE',  ( 15.43685675143394498, -16.52047792065556564, 11.49999999999998934 ) ) ;
#34372 = B_SPLINE_CURVE_WITH_KNOTS ( 'NONE', 3,
 ( #54498, #47389, #79323, #9817, #40767, #85433, #8822, #71728 ),
 .UNSPECIFIED., .F., .F.,
 ( 4, 2, 2, 4 ),
 ( -0.001240355328176878311, -0.0002398155169399626176, 0.0007607242942969530755, 0.002761803916770787931 ),
 .UNSPECIFIED. ) ;
#34373 = ADVANCED_FACE ( 'NONE', ( #89048 ), #88049, .F. ) ;
#34375 = ORIENTED_EDGE ( 'NONE', *, *, #65518, .F. ) ;
#34374 = DIRECTION ( 'NONE',  ( 0.000000000000000000, -1.000000000000000000, 0.000000000000000000 ) ) ;
#34376 = ORIENTED_EDGE ( 'NONE', *, *, #77896, .F. ) ;
#34377 = DIRECTION ( 'NONE',  ( 0.8788171126619707119, -0.4771587602595986910, 0.000000000000000000 ) ) ;
#34378 = EDGE_CURVE ( 'NONE', #294, #88628, #40486, .T. ) ;
#34379 = VECTOR ( 'NONE', #3445, 1000.000000000000000 ) ;
#34380 = CARTESIAN_POINT ( 'NONE',  ( 22.81105451610979173, -2.682774720514426559, -18.46691820600746681 ) ) ;
#34381 = ORIENTED_EDGE ( 'NONE', *, *, #44735, .T. ) ;
#34382 = CARTESIAN_POINT ( 'NONE',  ( -19.98373207111551508, 7.008865001458166155, -1.500000000000002220 ) ) ;
#34383 = CARTESIAN_POINT ( 'NONE',  ( 23.60872659128563811, -0.9000000000000000222, 2.097483029078132777 ) ) ;
#34384 = CARTESIAN_POINT ( 'NONE',  ( -125.6228709571500559, -23.47593901973091235, -1.443836447538995760 ) ) ;
#34385 = LINE ( 'NONE', #64866, #79462 ) ;
#34386 = CARTESIAN_POINT ( 'NONE',  ( 7.688942331755139747, 20.87172568467934752, -1.500000000000002220 ) ) ;
#34387 = CARTESIAN_POINT ( 'NONE',  ( -114.5158209565278469, -24.51314013834316086, 0.6176544820404251679 ) ) ;
#34388 = VERTEX_POINT ( 'NONE', #88547 ) ;
#34389 = CARTESIAN_POINT ( 'NONE',  ( -5.568927889719891944, -6.376774720514417183, 20.14881673916291760 ) ) ;
#34390 = CARTESIAN_POINT ( 'NONE',  ( 30.61643171304413613, 3.316774720514426456, 27.37433008668288181 ) ) ;
#34391 = CARTESIAN_POINT ( 'NONE',  ( -36.51285728403535558, -23.73791477778911130, 11.05961554403171121 ) ) ;
#34392 = CARTESIAN_POINT ( 'NONE',  ( 25.61870917940689196, -5.965225279485572685, 29.49402280011862487 ) ) ;
#34393 = CARTESIAN_POINT ( 'NONE',  ( -10.28394983263804185, -16.58134856480417341, 11.49999999999998934 ) ) ;
#34394 = CIRCLE ( 'NONE', #40907, 1.325999999999969647 ) ;
#34395 = CARTESIAN_POINT ( 'NONE',  ( 6.977786103627443559, 20.27319509581574408, -1.500000000000002220 ) ) ;
#34396 = CARTESIAN_POINT ( 'NONE',  ( -26.47871760004291630, -24.92774763277149574, 2.074684386906315847 ) ) ;
#34397 = AXIS2_PLACEMENT_3D ( 'NONE', #98538, #28535, #51389 ) ;
#34398 = LINE ( 'NONE', #2963, #35735 ) ;
#34399 = CARTESIAN_POINT ( 'NONE',  ( -77.54621141149542041, -24.34968618360934300, 0.1864209137778811143 ) ) ;
#34400 = CARTESIAN_POINT ( 'NONE',  ( -13.73562189146022661, -18.16285900770654393, -1.500000000000002220 ) ) ;
#34401 = B_SPLINE_CURVE_WITH_KNOTS ( 'NONE', 3,
 ( #84645, #46097, #77024, #98865 ),
 .UNSPECIFIED., .F., .F.,
 ( 4, 4 ),
 ( 1.387778780781445676E-17, 0.0001000000000000028508 ),
 .UNSPECIFIED. ) ;
#34402 =( LENGTH_UNIT ( ) NAMED_UNIT ( * ) SI_UNIT ( .MILLI., .METRE. ) );
#34403 = CARTESIAN_POINT ( 'NONE',  ( -102.5909830230292386, -24.15543982623908192, -0.2315651400026459694 ) ) ;
#34404 = CARTESIAN_POINT ( 'NONE',  ( 32.16024265030974050, 0.3587747205144265483, 16.27760796525321751 ) ) ;
#34405 = CARTESIAN_POINT ( 'NONE',  ( -10.29545327866581950, 17.06371652956568852, 11.49999999999999645 ) ) ;
#34406 = PLANE ( 'NONE',  #77787 ) ;
#34407 = B_SPLINE_CURVE_WITH_KNOTS ( 'NONE', 3,
 ( #36507, #5063, #75061, #5561 ),
 .UNSPECIFIED., .F., .F.,
 ( 4, 4 ),
 ( 0.7903502942768684258, 0.7993567255489840706 ),
 .UNSPECIFIED. ) ;
#34408 = CARTESIAN_POINT ( 'NONE',  ( -39.62372017418730508, -24.66019654487198665, 8.947790411086131712 ) ) ;
#34409 = CARTESIAN_POINT ( 'NONE',  ( -48.54706234259929687, -24.15543982623907482, -0.2315651400026527418 ) ) ;
#34410 = VERTEX_POINT ( 'NONE', #97155 ) ;
#34411 = CARTESIAN_POINT ( 'NONE',  ( 29.73849889714944084, 4.772794184420478203, -4.021328304942501930 ) ) ;
#34412 = CARTESIAN_POINT ( 'NONE',  ( -32.40343208386849483, -25.31558585043574183, 4.997857581739419075 ) ) ;
#34413 = CARTESIAN_POINT ( 'NONE',  ( -1.268225406894735396, -21.67698866206750097, 11.49999999999998934 ) ) ;
#34414 = CARTESIAN_POINT ( 'NONE',  ( -51.84991333203042529, -25.20452363795868678, 6.645056544736056559 ) ) ;
#34415 = CARTESIAN_POINT ( 'NONE',  ( -9.112395119859147741, -17.30902560603237106, -1.500000000000002220 ) ) ;
#34416 = DIRECTION ( 'NONE',  ( -0.6392559695863496705, -0.000000000000000000, -0.7689940216596069522 ) ) ;
#34417 = AXIS2_PLACEMENT_3D ( 'NONE', #83329, #75707, #99042 ) ;
#34418 = ORIENTED_EDGE ( 'NONE', *, *, #60888, .T. ) ;
#34419 = DATE_TIME_ROLE ( 'creation_date' ) ;
#34420 = SECURITY_CLASSIFICATION ( '', '', #76313 ) ;
#34421 = FACE_OUTER_BOUND ( 'NONE', #34186, .T. ) ;
#34422 = CARTESIAN_POINT ( 'NONE',  ( -2.750569593922542300, -20.27526743851804625, 11.49999999999999645 ) ) ;
#34423 = LINE ( 'NONE', #65403, #27815 ) ;
#34424 = CARTESIAN_POINT ( 'NONE',  ( -89.52287095715006160, -23.47593901973090169, -1.443836447538996426 ) ) ;
#34425 = ORIENTED_EDGE ( 'NONE', *, *, #57170, .F. ) ;
#34426 = FACE_OUTER_BOUND ( 'NONE', #80225, .T. ) ;
#34427 = CARTESIAN_POINT ( 'NONE',  ( 5.802984775641024662, -6.376774720514402972, 18.35026041666666430 ) ) ;
#34428 = EDGE_CURVE ( 'NONE', #73685, #18831, #12901, .T. ) ;
#34429 = DIRECTION ( 'NONE',  ( -1.000000000000000000, -3.773278334444167608E-23, -8.201307833595939069E-29 ) ) ;
#34430 = AXIS2_PLACEMENT_3D ( 'NONE', #82534, #89656, #12025 ) ;
#34431 = CARTESIAN_POINT ( 'NONE',  ( -109.5183339203764348, -23.96119346886880663, -0.6495511937832053606 ) ) ;
#34433 = ORIENTED_EDGE ( 'NONE', *, *, #93067, .T. ) ;
#34432 = EDGE_CURVE ( 'NONE', #86774, #71695, #55032, .T. ) ;
#34434 = LINE ( 'NONE', #65414, #75499 ) ;
#34435 = ADVANCED_FACE ( 'NONE', ( #89541 ), #34264, .F. ) ;
#34436 = CARTESIAN_POINT ( 'NONE',  ( 22.25235761598246143, -5.642936543268669780, 11.49999999999999645 ) ) ;
#34437 = CARTESIAN_POINT ( 'NONE',  ( 7.803535043518188274, -21.38454823780343617, -1.500000000000002220 ) ) ;
#34438 = CARTESIAN_POINT ( 'NONE',  ( 4.527536911777373163, -6.376774720514422512, 21.53954785142818196 ) ) ;
#34439 = B_SPLINE_SURFACE_WITH_KNOTS ( 'NONE', 3, 3, ( 
 ( #16560, #47534, #76957, #78458 ),
 ( #63778, #70363, #1856, #39907 ),
 ( #92685, #31293, #17068, #85578 ),
 ( #56154, #16060, #47033, #848 ),
 ( #7451, #31803, #46527, #38910 ),
 ( #62773, #70873, #94186, #32297 ),
 ( #69865, #1363, #346, #24673 ),
 ( #48034, #9460, #94695, #38408 ),
 ( #40418, #25178, #100280, #30800 ),
 ( #61765, #18073, #58639, #88595 ) ),
 .UNSPECIFIED., .F., .F., .F.,
 ( 4, 3, 3, 4 ),
 ( 4, 4 ),
 ( 0.0004766839783823869237, 0.1491231665100173909, 0.2234464077758348821, 0.2977696490416523734 ),
 ( 0.09950601477590118038, 0.1005780351604402129 ),
 .UNSPECIFIED. ) ;
#34440 = EDGE_CURVE ( 'NONE', #96725, #7991, #97449, .T. ) ;
#34441 = CARTESIAN_POINT ( 'NONE',  ( -7.749999999999996447, 25.69999999999999574, 2.100000000000000089 ) ) ;
#34442 = CARTESIAN_POINT ( 'NONE',  ( -81.52287095715006160, -24.50321055353805377, 9.387540953477525818 ) ) ;
#34443 = CARTESIAN_POINT ( 'NONE',  ( -78.58953762381671027, -23.48786465467241413, 11.44779295918254469 ) ) ;
#34444 = ADVANCED_FACE ( 'NONE', ( #21014 ), #22499, .T. ) ;
#34445 = CARTESIAN_POINT ( 'NONE',  ( -54.58953762381672448, -23.48786465467240347, 11.44779295918255180 ) ) ;
#34446 = CARTESIAN_POINT ( 'NONE',  ( 8.256513476402210117, 20.27555108428041208, 11.49999999999998934 ) ) ;
#34447 = CARTESIAN_POINT ( 'NONE',  ( -69.50159385232926468, -24.35071581493542681, 9.817618358456032368 ) ) ;
#34448 = CIRCLE ( 'NONE', #81461, 1.000000000000000000 ) ;
#34449 = CARTESIAN_POINT ( 'NONE',  ( -49.74369414166533687, -25.31543073408252909, 4.940877929217667663 ) ) ;
#34450 = CARTESIAN_POINT ( 'NONE',  ( -71.70422574834498164, -25.25838781600607419, 6.074309804579013594 ) ) ;
#34451 = PLANE ( 'NONE',  #6394 ) ;
#34452 = ORIENTED_EDGE ( 'NONE', *, *, #22255, .T. ) ;
#34453 = CARTESIAN_POINT ( 'NONE',  ( 5.143668500415711442, -19.74887971880038151, -1.500000000000002220 ) ) ;
#34454 = EDGE_LOOP ( 'NONE', ( #17219, #66090, #34341, #41835 ) ) ;
#34455 = ORIENTED_EDGE ( 'NONE', *, *, #94827, .F. ) ;
#34456 = ORIENTED_EDGE ( 'NONE', *, *, #71690, .F. ) ;
#34457 = ADVANCED_FACE ( 'NONE', ( #98134 ), #70297, .T. ) ;
#34458 = CARTESIAN_POINT ( 'NONE',  ( -14.43837761634077310, -17.93274050997184332, -1.500000000000002220 ) ) ;
#34459 = CARTESIAN_POINT ( 'NONE',  ( 33.12653832968937451, 6.376774720514426953, -7.315055336576590683 ) ) ;
#34460 = CARTESIAN_POINT ( 'NONE',  ( -3.510519812331947875, -19.85243952969433323, -1.500000000000002220 ) ) ;
#34461 = ORIENTED_EDGE ( 'NONE', *, *, #80585, .F. ) ;
#34462 = DIRECTION ( 'NONE',  ( -0.000000000000000000, 1.000000000000000000, -0.000000000000000000 ) ) ;
#34463 = DIRECTION ( 'NONE',  ( 1.000000000000000000, -0.000000000000000000, -0.000000000000000000 ) ) ;
#34464 = CARTESIAN_POINT ( 'NONE',  ( -95.54445644477492294, -24.83618233451450408, 1.606449574219538157 ) ) ;
#34465 = CARTESIAN_POINT ( 'NONE',  ( 3.509873074917118085, 5.965225279485572685, 29.15869884040363758 ) ) ;
#34467 = ORIENTED_EDGE ( 'NONE', *, *, #6823, .F. ) ;
#34466 = CARTESIAN_POINT ( 'NONE',  ( 18.61059577090848549, -10.47110149595715711, 11.49999999999999645 ) ) ;
#34468 = CARTESIAN_POINT ( 'NONE',  ( -55.52287095715010423, -24.14321612903117398, -0.2833117244521657918 ) ) ;
#34469 = AXIS2_PLACEMENT_3D ( 'NONE', #42300, #88947, #56512 ) ;
#34470 = ORIENTED_EDGE ( 'NONE', *, *, #23087, .T. ) ;
#34471 = CARTESIAN_POINT ( 'NONE',  ( 18.30470771955606679, 12.64531542519679697, 11.49999999999998934 ) ) ;
#34472 = CARTESIAN_POINT ( 'NONE',  ( -19.97286373971314433, -5.326668811655218327, -1.500000000000002220 ) ) ;
#34473 = ORIENTED_EDGE ( 'NONE', *, *, #64830, .F. ) ;
#34474 = PLANE ( 'NONE',  #74543 ) ;
#34475 = ORIENTED_EDGE ( 'NONE', *, *, #93866, .T. ) ;
#34476 = CARTESIAN_POINT ( 'NONE',  ( 2.750000000000001332, 26.59999999999999432, 2.100000000000000089 ) ) ;
#34477 = VERTEX_POINT ( 'NONE', #5382 ) ;
#34478 = DIRECTION ( 'NONE',  ( 0.000000000000000000, 0.000000000000000000, 1.000000000000000000 ) ) ;
#34479 = CARTESIAN_POINT ( 'NONE',  ( -2.499008156623981236, -20.81284420272260860, -1.500000000000002220 ) ) ;
#34481 = EDGE_CURVE ( 'NONE', #58570, #58197, #97728, .T. ) ;
#34480 = CARTESIAN_POINT ( 'NONE',  ( -3.281320334969873631, 21.64054093270537393, 11.49999999999999645 ) ) ;
#34482 = DIRECTION ( 'NONE',  ( 0.000000000000000000, 0.000000000000000000, 1.000000000000000000 ) ) ;
#34483 = CARTESIAN_POINT ( 'NONE',  ( 21.70358988458699301, 5.938112137899119070, 11.49999999999998934 ) ) ;
#34484 = CARTESIAN_POINT ( 'NONE',  ( 15.12549221760053086, 14.48511125727034177, 11.49999999999998934 ) ) ;
#34485 = CARTESIAN_POINT ( 'NONE',  ( -3.108974358974359475, -6.376774720514417183, 20.36458333333334281 ) ) ;
#34486 = EDGE_CURVE ( 'NONE', #12639, #5619, #67293, .T. ) ;
#34487 = CARTESIAN_POINT ( 'NONE',  ( -57.62287095715003460, -24.50216790748097395, 0.6166512839513648148 ) ) ;
#34488 = VECTOR ( 'NONE', #49002, 1000.000000000000000 ) ;
#34489 = CARTESIAN_POINT ( 'NONE',  ( -70.55620429048339304, -23.47596703998600276, 11.44779298504227505 ) ) ;
#34490 = ORIENTED_EDGE ( 'NONE', *, *, #57147, .F. ) ;
#34491 = LOCAL_TIME ( 0, 54, 15.00000000000000000, #65631 ) ;
#34492 = ORIENTED_EDGE ( 'NONE', *, *, #64854, .T. ) ;
#34493 = ORIENTED_EDGE ( 'NONE', *, *, #4531, .T. ) ;
#34494 = CARTESIAN_POINT ( 'NONE',  ( -99.29687923781919778, -25.12215468360345128, 6.149712483925878104 ) ) ;
#34495 = VERTEX_POINT ( 'NONE', #98719 ) ;
#34496 = CARTESIAN_POINT ( 'NONE',  ( 7.480126432006339421, -20.11416664461015458, -1.500000000000002220 ) ) ;
#34497 = AXIS2_PLACEMENT_3D ( 'NONE', #30142, #200, #77308 ) ;
#34498 = EDGE_CURVE ( 'NONE', #54462, #51886, #17817, .T. ) ;
#34499 = ORIENTED_EDGE ( 'NONE', *, *, #63095, .T. ) ;
#34500 = CARTESIAN_POINT ( 'NONE',  ( 0.2196812790064107401, -5.876774720514408301, 19.42522865122897002 ) ) ;
#34501 = CARTESIAN_POINT ( 'NONE',  ( -19.97109070424261645, 6.737033823242594366, -1.500000000000002220 ) ) ;
#34502 = DIRECTION ( 'NONE',  ( -0.06975647374412549673, -0.9975640502598241977, 0.000000000000000000 ) ) ;
#34503 = DIRECTION ( 'NONE',  ( 0.000000000000000000, 1.000000000000000000, 0.000000000000000000 ) ) ;
#34504 = DIRECTION ( 'NONE',  ( 0.000000000000000000, -1.000000000000000000, 0.000000000000000000 ) ) ;
#34505 = CARTESIAN_POINT ( 'NONE',  ( -80.61306835763387824, -25.29534349779240188, 4.525992644586477098 ) ) ;
#34506 = CARTESIAN_POINT ( 'NONE',  ( -109.3584176993576591, -25.28950181196791647, 4.206202504803813191 ) ) ;
#34507 = CARTESIAN_POINT ( 'NONE',  ( -5.561696574893697509, -21.35426480686918538, -1.500000000000002220 ) ) ;
#34508 = AXIS2_PLACEMENT_3D ( 'NONE', #99350, #60316, #93241 ) ;
#34509 = VERTEX_POINT ( 'NONE', #51067 ) ;
#34510 = CARTESIAN_POINT ( 'NONE',  ( -116.5534077701025240, -24.34968618360935366, 0.1864209137779019587 ) ) ;
#34511 = ADVANCED_FACE ( 'NONE', ( #36837 ), #36335, .F. ) ;
#34512 = CARTESIAN_POINT ( 'NONE',  ( -111.6228709571500417, -24.51387760970724727, 9.387446482453414731 ) ) ;
#34513 = CARTESIAN_POINT ( 'NONE',  ( -60.48077622483229021, -25.00158670708910336, 2.256160236439220590 ) ) ;
#34514 = CARTESIAN_POINT ( 'NONE',  ( -62.63182337673452338, -24.35071581493542325, 9.817618358456032368 ) ) ;
#34515 = DIRECTION ( 'NONE',  ( 0.000000000000000000, 0.000000000000000000, -1.000000000000000000 ) ) ;
#34516 = CARTESIAN_POINT ( 'NONE',  ( -127.5228709571499763, -23.48783264082477373, -1.443836473390082586 ) ) ;
#34517 = CARTESIAN_POINT ( 'NONE',  ( -1.966620079519992181, -21.27258529651320274, 11.49999999999998934 ) ) ;
#34518 = CARTESIAN_POINT ( 'NONE',  ( -70.66315859205543859, -25.31500238285650184, 4.882613580410660070 ) ) ;
#34519 = CARTESIAN_POINT ( 'NONE',  ( -52.52287095715009713, -23.48783264083416356, -1.443836473375487151 ) ) ;
#34520 = DIRECTION ( 'NONE',  ( 0.7689940216596065081, 7.885106708985488048E-16, -0.6392559695863502256 ) ) ;
#34521 = CARTESIAN_POINT ( 'NONE',  ( -47.62287095715004881, -29.50247984919015209, -1.443849546365058689 ) ) ;
#34522 = PRODUCT_DEFINITION ( 'UNKNOWN', '', #78135, #13440 ) ;
#34523 = CARTESIAN_POINT ( 'NONE',  ( 18.14931799402153345, 13.46472642042223633, -1.500000000000002220 ) ) ;
#34524 = B_SPLINE_SURFACE_WITH_KNOTS ( 'NONE', 3, 3, ( 
 ( #66463, #54093, #23606, #14507 ),
 ( #54580, #62201, #85515, #38347 ),
 ( #37365, #44979, #75904, #68806 ),
 ( #283, #84020, #93124, #68308 ),
 ( #30737, #77394, #51209, #7894 ),
 ( #85014, #92627, #46969, #45482 ),
 ( #82151, #14004, #46464, #53596 ) ),
 .UNSPECIFIED., .F., .F., .F.,
 ( 4, 3, 4 ),
 ( 4, 4 ),
 ( 0.7945040050992241421, 0.8970133687736501216, 0.9995227324480759901 ),
 ( 0.3795904564402555748, 0.3807784251392243857 ),
 .UNSPECIFIED. ) ;
#34525 = CARTESIAN_POINT ( 'NONE',  ( 10.24059822343757808, -5.876774720514426953, 0.000000000000000000 ) ) ;
#34526 = EDGE_LOOP ( 'NONE', ( #52747, #62696, #41095, #22719 ) ) ;
#34527 = DIRECTION ( 'NONE',  ( 0.000000000000000000, 2.173523156925980399E-06, -0.9999999999976378895 ) ) ;
#34528 = CARTESIAN_POINT ( 'NONE',  ( -113.6228709571500559, -29.50250786944525672, 11.44777988621622988 ) ) ;
#34529 = CARTESIAN_POINT ( 'NONE',  ( -13.31955177964949755, -14.60123061082138385, 11.49999999999999645 ) ) ;
#34530 = CARTESIAN_POINT ( 'NONE',  ( 4.444543648262985869, 12.92677669529668627, 2.100000000000000089 ) ) ;
#34531 = CARTESIAN_POINT ( 'NONE',  ( -67.63121645805480853, -24.34968618360933235, 0.1864209137778811143 ) ) ;
#34532 = VERTEX_POINT ( 'NONE', #28723 ) ;
#34533 = DIRECTION ( 'NONE',  ( 0.000000000000000000, 0.000000000000000000, -1.000000000000000000 ) ) ;
#34534 = CARTESIAN_POINT ( 'NONE',  ( -110.5562042904834072, -23.47593901973091235, -1.443836447538999312 ) ) ;
#34535 = AXIS2_PLACEMENT_3D ( 'NONE', #38830, #23591, #85501 ) ;
#34536 = CARTESIAN_POINT ( 'NONE',  ( -67.52287095715006160, -29.50247984919015209, -1.443849546365055359 ) ) ;
#34537 = CARTESIAN_POINT ( 'NONE',  ( -21.34238180412542718, 3.497892552127677135, -1.500000000000002220 ) ) ;
#34538 = CARTESIAN_POINT ( 'NONE',  ( -76.62287095715007013, -29.50250786944525672, 11.44777988621623521 ) ) ;
#34539 = CARTESIAN_POINT ( 'NONE',  ( -59.62287095715004881, -23.47593901973091235, -1.443836447539007972 ) ) ;
#34540 = DIRECTION ( 'NONE',  ( -3.773278334453079618E-23, 0.9999999999976377785, 2.173523156925979975E-06 ) ) ;
#34541 = CARTESIAN_POINT ( 'NONE',  ( -81.88534077628074215, -25.24685308744633616, 6.293942982122114671 ) ) ;
#34542 = CARTESIAN_POINT ( 'NONE',  ( 1.028332004353105233, 19.75660188889424518, -1.500000000000002220 ) ) ;
#34543 = ORIENTED_EDGE ( 'NONE', *, *, #50284, .T. ) ;
#34544 = VECTOR ( 'NONE', #2357, 1000.000000000000114 ) ;
#34545 = CARTESIAN_POINT ( 'NONE',  ( 3.949161919925879172, -19.86910077469890723, 11.49999999999999645 ) ) ;
#34546 = CARTESIAN_POINT ( 'NONE',  ( -7.640838998533831194, -5.876774720514417183, 20.32624910079993086 ) ) ;
#34547 = B_SPLINE_CURVE_WITH_KNOTS ( 'NONE', 3,
 ( #10140, #88273, #49226, #86759, #16743, #17248, #55330 ),
 .UNSPECIFIED., .F., .F.,
 ( 4, 3, 4 ),
 ( 0.000000000000000000, 1.195459452644217715E-05, 2.107775188753445374E-05 ),
 .UNSPECIFIED. ) ;
#34548 = ORIENTED_EDGE ( 'NONE', *, *, #61193, .F. ) ;
#34549 = CARTESIAN_POINT ( 'NONE',  ( 28.87399897812680649, 1.477225279485574028, -12.57761096169975445 ) ) ;
#34550 = CARTESIAN_POINT ( 'NONE',  ( 7.160000000000000142, 0.1579206558577706254, 7.788828319098143105 ) ) ;
#34551 = CARTESIAN_POINT ( 'NONE',  ( 33.08751910920749140, 4.671536413567966228, -11.65282283138775377 ) ) ;
#34552 = LINE ( 'NONE', #57903, #22394 ) ;
#34553 = DIRECTION ( 'NONE',  ( 1.000000000000000000, 3.773278334444167608E-23, 8.201307833595939069E-29 ) ) ;
#34554 = CARTESIAN_POINT ( 'NONE',  ( -81.58953762381673869, -24.65952944569305316, 1.056160979905705011 ) ) ;
#34556 = EDGE_CURVE ( 'NONE', #88644, #10751, #13482, .T. ) ;
#34555 = CARTESIAN_POINT ( 'NONE',  ( 0.1258803491696451060, 20.03332480481931199, -1.500000000000002220 ) ) ;
#34557 = CARTESIAN_POINT ( 'NONE',  ( -82.62287095715004170, -23.47596703998600631, 11.44779298504227860 ) ) ;
#34558 = ORIENTED_EDGE ( 'NONE', *, *, #70736, .T. ) ;
#34559 = B_SPLINE_CURVE_WITH_KNOTS ( 'NONE', 3,
 ( #69948, #17664, #46628, #86173 ),
 .UNSPECIFIED., .F., .F.,
 ( 4, 4 ),
 ( 0.000000000000000000, 9.999999999998206125E-05 ),
 .UNSPECIFIED. ) ;
#34560 = B_SPLINE_CURVE_WITH_KNOTS ( 'NONE', 3,
 ( #78808, #93042, #70222, #23521 ),
 .UNSPECIFIED., .F., .F.,
 ( 4, 4 ),
 ( 0.000000000000000000, 1.000000000000000000 ),
 .UNSPECIFIED. ) ;
#34561 = CONICAL_SURFACE ( 'NONE', #91260, 2.999999999999999112, 0.7853981633974412846 ) ;
#34562 = ORIENTED_EDGE ( 'NONE', *, *, #75193, .T. ) ;
#34563 = CARTESIAN_POINT ( 'NONE',  ( -32.62287095715004881, -24.35013146730203815, 9.818937971375115481 ) ) ;
#34564 = EDGE_CURVE ( 'NONE', #90802, #1762, #65810, .T. ) ;
#34565 = DIRECTION ( 'NONE',  ( 1.000000000000000000, 3.773278334444167608E-23, 8.201307833595939069E-29 ) ) ;
#34566 = CARTESIAN_POINT ( 'NONE',  ( -84.62287095715005592, -29.50248528299804818, 1.056150453629038477 ) ) ;
#34567 = EDGE_CURVE ( 'NONE', #20207, #55313, #96200, .T. ) ;
#34568 = CARTESIAN_POINT ( 'NONE',  ( -113.5228709571500332, -23.94994826722565406, -0.6494450866342719175 ) ) ;
#34569 = CARTESIAN_POINT ( 'NONE',  ( -73.59228414436695687, -24.15543982623907127, -0.2315651400026654816 ) ) ;
#34570 = CARTESIAN_POINT ( 'NONE',  ( 14.70028154896511552, 3.418387289166273657, -28.41026772490838681 ) ) ;
#34571 = VECTOR ( 'NONE', #50901, 1000.000000000000000 ) ;
#34572 = CARTESIAN_POINT ( 'NONE',  ( 282.9764569301858046, -0.6647747205144264315, 20.79159422840526616 ) ) ;
#34573 = ORIENTED_EDGE ( 'NONE', *, *, #70853, .F. ) ;
#34574 = CARTESIAN_POINT ( 'NONE',  ( -16.58479117878708209, 11.75282063728064053, -1.500000000000002220 ) ) ;
#34575 = CIRCLE ( 'NONE', #11894, 2.040000000000000036 ) ;
#34576 = ORIENTED_EDGE ( 'NONE', *, *, #84467, .T. ) ;
#34577 = EDGE_CURVE ( 'NONE', #57603, #29911, #21094, .T. ) ;
#34578 = CARTESIAN_POINT ( 'NONE',  ( -0.4961427919413599064, 22.93664481792237453, -1.500000000000002220 ) ) ;
#34579 = CARTESIAN_POINT ( 'NONE',  ( 31.65328924465906368, 5.892800044774432422, 28.08003312682333785 ) ) ;
#34580 = ORIENTED_EDGE ( 'NONE', *, *, #16895, .T. ) ;
#34581 = CARTESIAN_POINT ( 'NONE',  ( -109.5228709571500616, -24.65952944569305316, 1.056160979905704123 ) ) ;
#34582 = CARTESIAN_POINT ( 'NONE',  ( -50.16062266432883376, -25.12215416095027720, 7.085347845352387708 ) ) ;
#34583 = DIRECTION ( 'NONE',  ( -0.7071067811865513475, -0.7071067811865435759, 0.000000000000000000 ) ) ;
#34584 = CARTESIAN_POINT ( 'NONE',  ( -13.58512445790048417, 16.25115196636789250, 11.49999999999999645 ) ) ;
#34585 = CARTESIAN_POINT ( 'NONE',  ( 2.574831182292884435, -22.01391258260016315, -1.500000000000002220 ) ) ;
#34586 = CARTESIAN_POINT ( 'NONE',  ( 6.226698476505521995, -19.64469265145860177, -1.500000000000002220 ) ) ;
#34587 = ORIENTED_EDGE ( 'NONE', *, *, #40380, .T. ) ;
#34588 = CARTESIAN_POINT ( 'NONE',  ( -43.52287095715007581, -23.47593901973090169, -1.443836447538997092 ) ) ;
#34589 = ORIENTED_EDGE ( 'NONE', *, *, #69180, .T. ) ;
#34590 = CARTESIAN_POINT ( 'NONE',  ( -54.49170867734796531, -24.51314013834315020, 0.6176544820404069602 ) ) ;
#34591 = CARTESIAN_POINT ( 'NONE',  ( -126.6228709571500559, -23.96177878511310055, 10.65340807706329151 ) ) ;
#34592 = ORIENTED_EDGE ( 'NONE', *, *, #32754, .F. ) ;
#34593 = EDGE_LOOP ( 'NONE', ( #90096, #16408, #18094, #24799 ) ) ;
#34594 = B_SPLINE_CURVE_WITH_KNOTS ( 'NONE', 3,
 ( #29907, #75573, #67989, #22278, #52756, #83694 ),
 .UNSPECIFIED., .F., .F.,
 ( 4, 2, 4 ),
 ( 1.570755371633856203E-05, 0.001396183895866086886, 0.002776660238015835145 ),
 .UNSPECIFIED. ) ;
#34595 = ORIENTED_EDGE ( 'NONE', *, *, #24452, .T. ) ;
#34596 = LINE ( 'NONE', #26974, #47013 ) ;
#34597 = DIRECTION ( 'NONE',  ( 0.000000000000000000, 2.173523156925980399E-06, -0.9999999999976378895 ) ) ;
#34598 = DIRECTION ( 'NONE',  ( -3.773278334453079618E-23, 0.9999999999976377785, 2.173523156925979975E-06 ) ) ;
#34599 = CARTESIAN_POINT ( 'NONE',  ( 4.358738815032396907, -20.29635662749097236, -1.500000000000002220 ) ) ;
#34600 = CARTESIAN_POINT ( 'NONE',  ( -11.39883337241029793, 18.50525654427185884, 11.49999999999999645 ) ) ;
#34601 = EDGE_LOOP ( 'NONE', ( #91959, #65470, #66562, #8743 ) ) ;
#34602 = AXIS2_PLACEMENT_3D ( 'NONE', #20742, #15136, #5031 ) ;
#34603 = CARTESIAN_POINT ( 'NONE',  ( -62.52287095715006160, -24.65952944569304606, 1.056160979905695463 ) ) ;
#34604 = CARTESIAN_POINT ( 'NONE',  ( -96.62287095715004170, -24.65952944569304606, 1.056160979905703456 ) ) ;
#34605 = CARTESIAN_POINT ( 'NONE',  ( 6.497064355747536268, 21.42967291005575348, 11.49999999999998934 ) ) ;
#34606 = CARTESIAN_POINT ( 'NONE',  ( 11.56983764158150407, -0.3587747205144265483, 28.29037853177889517 ) ) ;
#34607 = CARTESIAN_POINT ( 'NONE',  ( -57.62287095715004881, -23.47596703998600276, 11.44779298504227683 ) ) ;
#34609 = ADVANCED_FACE ( 'NONE', ( #44955 ), #89127, .F. ) ;
#34608 = VERTEX_POINT ( 'NONE', #58673 ) ;
#34610 = CARTESIAN_POINT ( 'NONE',  ( 10.86264265031000775, -1.324225279485583551, -28.05717073599341660 ) ) ;
#34611 = DIRECTION ( 'NONE',  ( -3.773278334453079618E-23, 0.9999999999976377785, 2.173523156925979975E-06 ) ) ;
#34612 = VECTOR ( 'NONE', #23410, 1000.000000000000114 ) ;
#34613 = ORIENTED_EDGE ( 'NONE', *, *, #49674, .F. ) ;
#34614 = EDGE_LOOP ( 'NONE', ( #70942, #76959, #49994, #81814 ) ) ;
#34615 = CARTESIAN_POINT ( 'NONE',  ( -69.62287095715004170, -24.51387760970723662, 9.387446482453421837 ) ) ;
#34616 = EDGE_CURVE ( 'NONE', #40829, #50455, #37299, .T. ) ;
#34617 = ORIENTED_EDGE ( 'NONE', *, *, #86984, .F. ) ;
#34618 = EDGE_CURVE ( 'NONE', #84065, #9013, #89622, .T. ) ;
#34619 = CARTESIAN_POINT ( 'NONE',  ( 18.67678363807796416, 10.12720680154768971, -1.500000000000002220 ) ) ;
#34620 = EDGE_LOOP ( 'NONE', ( #72141, #72657, #1800, #97232 ) ) ;
#34621 = DIRECTION ( 'NONE',  ( 0.000000000000000000, 0.000000000000000000, -1.000000000000000000 ) ) ;
#34622 = CARTESIAN_POINT ( 'NONE',  ( 21.83686239284238084, -0.8075297431944471471, 11.49999999999998934 ) ) ;
#34623 = CARTESIAN_POINT ( 'NONE',  ( -103.5492830802958082, -24.51419770103155926, 9.386484678747176957 ) ) ;
#34624 = CARTESIAN_POINT ( 'NONE',  ( -22.63693132222386950, 1.387278323242118416, -1.500000000000002220 ) ) ;
#34625 = DIRECTION ( 'NONE',  ( -0.000000000000000000, 2.173523156925979552E-06, -0.9999999999976378895 ) ) ;
#34626 = DIRECTION ( 'NONE',  ( 1.000000000000000000, 3.773278334444166432E-23, 8.201307841325785021E-29 ) ) ;
#34627 = CARTESIAN_POINT ( 'NONE',  ( -17.40403014803320758, -13.24600170205644289, -1.500000000000002220 ) ) ;
#34628 = CARTESIAN_POINT ( 'NONE',  ( 7.164812103570541879, -5.876774720514421624, 20.85668272347560404 ) ) ;
#34629 = EDGE_LOOP ( 'NONE', ( #51476, #1238, #23582, #1644 ) ) ;
#34630 = CARTESIAN_POINT ( 'NONE',  ( -65.62287095715007013, -24.83602698348160942, 1.605859176311267511 ) ) ;
#34631 = CARTESIAN_POINT ( 'NONE',  ( -126.5895376238167529, -24.65952944569305316, 1.056160979905704123 ) ) ;
#34632 = ORIENTED_EDGE ( 'NONE', *, *, #35892, .F. ) ;
#34633 = CARTESIAN_POINT ( 'NONE',  ( -24.90875734969025501, -5.965225279485572685, 26.43402280011862615 ) ) ;
#34634 = ORIENTED_EDGE ( 'NONE', *, *, #44352, .F. ) ;
#34635 = LINE ( 'NONE', #74191, #49203 ) ;
#34636 = FACE_BOUND ( 'NONE', #56210, .T. ) ;
#34637 = CARTESIAN_POINT ( 'NONE',  ( 19.98919582620916913, -7.218065965386815996, -1.500000000000002220 ) ) ;
#34638 = DIRECTION ( 'NONE',  ( -1.000000000000000000, -0.000000000000000000, -0.000000000000000000 ) ) ;
#34639 = CARTESIAN_POINT ( 'NONE',  ( -53.01255352321339842, -5.356774720514425603, 35.59556822165056644 ) ) ;
#34640 = EDGE_CURVE ( 'NONE', #24018, #75990, #21586, .T. ) ;
#34641 = CARTESIAN_POINT ( 'NONE',  ( -85.58737842399442286, -24.63355581998386157, 0.9682620441943895484 ) ) ;
#34642 = CARTESIAN_POINT ( 'NONE',  ( -68.63577655697397972, -24.15543982623907127, -0.2315651400026649820 ) ) ;
#34643 = VECTOR ( 'NONE', #42654, 1000.000000000000114 ) ;
#34644 = CARTESIAN_POINT ( 'NONE',  ( -117.6260431914922862, -24.15620529776629510, 10.23563542870659582 ) ) ;
#34645 = ORIENTED_EDGE ( 'NONE', *, *, #62086, .F. ) ;
#34646 = CARTESIAN_POINT ( 'NONE',  ( 9.052818235119415746, 17.31195010612007223, 11.49999999999999645 ) ) ;
#34647 = CYLINDRICAL_SURFACE ( 'NONE', #90833, 0.2499999999997798983 ) ;
#34648 = CIRCLE ( 'NONE', #47619, 251.4258649670780699 ) ;
#34649 = CARTESIAN_POINT ( 'NONE',  ( -29.81066147699621283, -25.24716167724356097, 5.128593285976438487 ) ) ;
#34650 = ORIENTED_EDGE ( 'NONE', *, *, #75336, .T. ) ;
#34651 = DIRECTION ( 'NONE',  ( -0.000000000000000000, -1.000000000000000000, -0.000000000000000000 ) ) ;
#34652 = ADVANCED_FACE ( 'NONE', ( #43458 ), #91110, .T. ) ;
#34653 = CARTESIAN_POINT ( 'NONE',  ( -99.45104055277701605, -25.25095879578016422, 5.670438387523640600 ) ) ;
#34654 = CARTESIAN_POINT ( 'NONE',  ( -80.52287095715006160, -23.47596703998600631, 11.44779298504228571 ) ) ;
#34655 = CARTESIAN_POINT ( 'NONE',  ( 31.79364159983995464, 5.965225279485572685, -11.59305536555894278 ) ) ;
#34656 = CARTESIAN_POINT ( 'NONE',  ( 11.88433821776028942, -15.71472908967258242, -1.500000000000002220 ) ) ;
#34657 = EDGE_CURVE ( 'NONE', #11314, #13213, #35834, .T. ) ;
#34658 = VERTEX_POINT ( 'NONE', #20598 ) ;
#34659 = CARTESIAN_POINT ( 'NONE',  ( 31.88667425545052581, -1.682774720514426114, -9.651215965565016930 ) ) ;
#34660 = CARTESIAN_POINT ( 'NONE',  ( 2.976770017179964700, -5.876774720514419847, 20.68690469677381927 ) ) ;
#34661 = CALENDAR_DATE ( 2026, 9, 10 ) ;
#34662 = ORIENTED_EDGE ( 'NONE', *, *, #54713, .F. ) ;
#34663 = FACE_OUTER_BOUND ( 'NONE', #50092, .T. ) ;
#34664 = CARTESIAN_POINT ( 'NONE',  ( -123.6228709571500559, -29.50250243563736774, 8.947779886222134493 ) ) ;
#34665 = CARTESIAN_POINT ( 'NONE',  ( -47.51396546215941186, -23.73766607897670866, -1.055555164236438692 ) ) ;
#34666 = LINE ( 'NONE', #33663, #37983 ) ;
#34667 = CARTESIAN_POINT ( 'NONE',  ( -79.91667645764968597, -25.33009845126374415, 4.495758016894969344 ) ) ;
#34668 = CARTESIAN_POINT ( 'NONE',  ( 0.000000000000000000, -2.682774720514426559, 0.000000000000000000 ) ) ;
#34669 = CARTESIAN_POINT ( 'NONE',  ( -97.62287095715004170, -24.65952944569304606, 1.056160979905701236 ) ) ;
#34671 = EDGE_CURVE ( 'NONE', #54808, #40322, #35344, .T. ) ;
#34670 = CARTESIAN_POINT ( 'NONE',  ( 12.75013301566243129, -15.34773647900153115, -1.500000000000002220 ) ) ;
#34672 = AXIS2_PLACEMENT_3D ( 'NONE', #75481, #73508, #50672 ) ;
#34673 = CARTESIAN_POINT ( 'NONE',  ( -0.08316136044590859144, -21.97341083746030321, 10.06556358067885348 ) ) ;
#34674 = CARTESIAN_POINT ( 'NONE',  ( 4.300141163375406528, 19.41444791797076874, -1.500000000000002220 ) ) ;
#34675 = ORIENTED_EDGE ( 'NONE', *, *, #56232, .F. ) ;
#34676 = CARTESIAN_POINT ( 'NONE',  ( -25.92875734969026169, 5.356774720514426491, 23.50402280011861933 ) ) ;
#34677 = DIRECTION ( 'NONE',  ( 0.000000000000000000, 0.000000000000000000, -1.000000000000000000 ) ) ;
#34678 = CARTESIAN_POINT ( 'NONE',  ( 14.02639803017889086, -6.376774720514426065, -25.20535965011783119 ) ) ;
#34679 = CARTESIAN_POINT ( 'NONE',  ( 5.792680761630559338, -19.98616098212858105, 11.49999999999999645 ) ) ;
#34680 = CARTESIAN_POINT ( 'NONE',  ( -7.338700834008208496, -5.876774720514410077, 19.35116211686183263 ) ) ;
#34681 = EDGE_CURVE ( 'NONE', #70270, #63070, #33284, .T. ) ;
#34682 = CARTESIAN_POINT ( 'NONE',  ( 30.09341516180546350, -1.684774720514424562, -11.39311774897855933 ) ) ;
#34683 = CARTESIAN_POINT ( 'NONE',  ( 22.79674358141071977, 1.614764915196592598, 11.49999999999999645 ) ) ;
#34684 = VERTEX_POINT ( 'NONE', #51567 ) ;
#34685 = PLANE ( 'NONE',  #34919 ) ;
#34686 = EDGE_CURVE ( 'NONE', #58859, #99983, #54549, .T. ) ;
#34687 = DIRECTION ( 'NONE',  ( -1.000000000000000000, -3.773278334444166432E-23, -8.201307841325785021E-29 ) ) ;
#34688 = VERTEX_POINT ( 'NONE', #69779 ) ;
#34689 = CARTESIAN_POINT ( 'NONE',  ( 6.697674113365701842, 19.09646837838083400, -1.500000000000002220 ) ) ;
#34690 = CARTESIAN_POINT ( 'NONE',  ( 6.830155907162054341, -5.876774720514427841, 21.76451523534627341 ) ) ;
#34691 = EDGE_CURVE ( 'NONE', #86012, #49051, #87562, .T. ) ;
#34692 = FACE_OUTER_BOUND ( 'NONE', #79928, .T. ) ;
#34693 = EDGE_CURVE ( 'NONE', #44666, #3225, #1663, .T. ) ;
#34694 = FACE_OUTER_BOUND ( 'NONE', #27834, .T. ) ;
#34695 = VERTEX_POINT ( 'NONE', #30709 ) ;
#34696 = DIRECTION ( 'NONE',  ( 7.960204194457801640E-17, 1.000000000000000000, -1.571307496355802709E-16 ) ) ;
#34697 = CARTESIAN_POINT ( 'NONE',  ( -10.26098930579144763, 5.972795536074636757, 28.98685178976001353 ) ) ;
#34698 = CARTESIAN_POINT ( 'NONE',  ( 11.63622169266987783, 16.31392799894670631, -1.500000000000002220 ) ) ;
#34699 = CARTESIAN_POINT ( 'NONE',  ( 16.43158684610488862, 13.14696595092960152, 11.49999999999999645 ) ) ;
#34700 = DIRECTION ( 'NONE',  ( -0.06975647374412546897, -0.9975640502598241977, 0.000000000000000000 ) ) ;
#34701 = CARTESIAN_POINT ( 'NONE',  ( -124.6228709571500133, -24.33927499327854704, 9.819080762295811837 ) ) ;
#34702 = CARTESIAN_POINT ( 'NONE',  ( 11.67614657018352453, 18.69773523334854914, 11.49999999999998934 ) ) ;
#34703 = CARTESIAN_POINT ( 'NONE',  ( 20.52151214508650057, 3.625915217019311583E-15, -2.299999999999999822 ) ) ;
#34704 = FACE_OUTER_BOUND ( 'NONE', #78751, .T. ) ;
#34705 = CARTESIAN_POINT ( 'NONE',  ( -64.52287095715006160, -23.47596703998600631, 11.44779298504228926 ) ) ;
#34706 = DIRECTION ( 'NONE',  ( 1.000000000000000000, 3.773278334444166432E-23, 8.201307841325785021E-29 ) ) ;
#34707 = CARTESIAN_POINT ( 'NONE',  ( -86.52287095715006160, -24.65952944569304606, 1.056160979905700570 ) ) ;
#34708 = ORIENTED_EDGE ( 'NONE', *, *, #66892, .T. ) ;
#34709 = ORIENTED_EDGE ( 'NONE', *, *, #68908, .T. ) ;
#34710 = CARTESIAN_POINT ( 'NONE',  ( -117.6228709571500559, -23.48783264082479505, -1.443836473390058384 ) ) ;
#34711 = DIRECTION ( 'NONE',  ( 1.988296846060374587E-13, 1.000000000000000000, -1.446139281080278507E-13 ) ) ;
#34712 = CARTESIAN_POINT ( 'NONE',  ( -51.52287095715006160, -23.94994826722565406, -0.6494450866342730277 ) ) ;
#34713 = CARTESIAN_POINT ( 'NONE',  ( 20.52540449432101610, 0.9483640940595650104, -1.500000000000002220 ) ) ;
#34714 = EDGE_LOOP ( 'NONE', ( #15643, #85638, #90523, #69100 ) ) ;
#34715 = DIRECTION ( 'NONE',  ( -3.773278334453079618E-23, 0.9999999999976377785, 2.173523156925979975E-06 ) ) ;
#34716 = CARTESIAN_POINT ( 'NONE',  ( 7.052174998393318184, -5.876774720514418071, 20.39928653130861136 ) ) ;
#34717 = CARTESIAN_POINT ( 'NONE',  ( -88.88918693012686845, -25.23397913219354649, 6.409327625488847602 ) ) ;
#34718 = CARTESIAN_POINT ( 'NONE',  ( -2.938769918389303459, -22.12206158279486345, -1.500000000000002220 ) ) ;
#34719 = CARTESIAN_POINT ( 'NONE',  ( 29.72843915439144524, -4.948038888671026037, 27.41656699113896067 ) ) ;
#34721 = EDGE_CURVE ( 'NONE', #40304, #4416, #92572, .T. ) ;
#34720 = PLANE ( 'NONE',  #40011 ) ;
#34722 = ORIENTED_EDGE ( 'NONE', *, *, #42551, .F. ) ;
#34723 = CARTESIAN_POINT ( 'NONE',  ( -42.62287095715002749, -24.50216790748098461, 0.6166512839513551558 ) ) ;
#34724 = CARTESIAN_POINT ( 'NONE',  ( -119.6228709571500417, -24.65952944569304961, 1.056160979905704789 ) ) ;
#34725 = B_SPLINE_CURVE_WITH_KNOTS ( 'NONE', 3,
 ( #92216, #92707, #67904, #6490, #90726, #15095 ),
 .UNSPECIFIED., .F., .F.,
 ( 4, 2, 4 ),
 ( 6.391158118952235087E-06, 0.001387004593080770967, 0.002767618028042589419 ),
 .UNSPECIFIED. ) ;
#34726 = CARTESIAN_POINT ( 'NONE',  ( -20.82246440549779720, 1.468558417816581807, -1.500000000000002220 ) ) ;
#34727 = ORIENTED_EDGE ( 'NONE', *, *, #98529, .F. ) ;
#34728 = VECTOR ( 'NONE', #97923, 1000.000000000000227 ) ;
#34730 = ORIENTED_EDGE ( 'NONE', *, *, #65771, .F. ) ;
#34729 = CARTESIAN_POINT ( 'NONE',  ( -40.25462936170517025, -25.11181042176191980, 2.840493060246056523 ) ) ;
#34731 = B_SPLINE_CURVE_WITH_KNOTS ( 'NONE', 3,
 ( #98840, #68899, #91728, #53691, #30332, #36450 ),
 .UNSPECIFIED., .F., .F.,
 ( 4, 2, 4 ),
 ( 1.570887131795413739E-05, 0.001396322306279765843, 0.002776935741241577573 ),
 .UNSPECIFIED. ) ;
#34732 = ORIENTED_EDGE ( 'NONE', *, *, #97527, .T. ) ;
#34733 = EDGE_CURVE ( 'NONE', #75066, #92960, #32025, .T. ) ;
#34734 = CARTESIAN_POINT ( 'NONE',  ( -33.62287095715005592, -23.47593901973091235, -1.443836447539013301 ) ) ;
#34735 = CARTESIAN_POINT ( 'NONE',  ( -12.45680796028966597, 17.00782699154285638, -1.500000000000002220 ) ) ;
#34736 = ORIENTED_EDGE ( 'NONE', *, *, #57032, .T. ) ;
#34737 = DIRECTION ( 'NONE',  ( -0.000000000000000000, 1.000000000000000000, -0.000000000000000000 ) ) ;
#34738 = DIRECTION ( 'NONE',  ( -0.000000000000000000, 0.000000000000000000, 1.000000000000000000 ) ) ;
#34739 = DIRECTION ( 'NONE',  ( -7.960204194457801640E-17, -1.000000000000000000, 0.000000000000000000 ) ) ;
#34740 = CARTESIAN_POINT ( 'NONE',  ( 29.73860345376319358, 5.356774720514425603, -4.021109907510727943 ) ) ;
#34741 = CARTESIAN_POINT ( 'NONE',  ( 7.344278919687202922, -6.376774720514417183, 20.19896341048075783 ) ) ;
#34742 = CARTESIAN_POINT ( 'NONE',  ( 10.00111611332133421, -19.26892646806700071, -1.500000000000002220 ) ) ;
#34743 = CARTESIAN_POINT ( 'NONE',  ( -108.5228709571500616, -23.47596703998600631, 11.44779298504228038 ) ) ;
#34745 = ORIENTED_EDGE ( 'NONE', *, *, #75818, .T. ) ;
#34744 = CARTESIAN_POINT ( 'NONE',  ( -17.00426676922356606, 14.40147940013276973, 11.49999999999999645 ) ) ;
#34746 = CARTESIAN_POINT ( 'NONE',  ( -51.39979512284951824, -25.31441837832753095, 5.729491880671105264 ) ) ;
#34747 = PLANE ( 'NONE',  #20033 ) ;
#34748 = CARTESIAN_POINT ( 'NONE',  ( -36.52287095715006870, -23.48786465467240347, 11.44779295918255180 ) ) ;
#34749 = ORIENTED_EDGE ( 'NONE', *, *, #22393, .T. ) ;
#34750 = AXIS2_PLACEMENT_3D ( 'NONE', #82994, #13487, #75383 ) ;
#34752 = ORIENTED_EDGE ( 'NONE', *, *, #10891, .T. ) ;
#34751 = LINE ( 'NONE', #12397, #52315 ) ;
#34753 = EDGE_LOOP ( 'NONE', ( #41379, #76753, #86601, #86256, #100240, #15289, #56457, #98055 ) ) ;
#34754 = DIRECTION ( 'NONE',  ( -1.734723475976806848E-16, 1.000000000000000000, 0.000000000000000000 ) ) ;
#34755 = CARTESIAN_POINT ( 'NONE',  ( -121.5213660948649164, -23.73766607897670866, -1.055555164236450905 ) ) ;
#34756 = ADVANCED_FACE ( 'NONE', ( #7867 ), #70276, .F. ) ;
#34757 = CARTESIAN_POINT ( 'NONE',  ( -35.52287095715007581, -23.84047902841601640, -0.8780736468305702092 ) ) ;
#34758 = CARTESIAN_POINT ( 'NONE',  ( -32.62287095715004881, -23.73907113216990439, -1.053371485793237250 ) ) ;
#34759 = ORIENTED_EDGE ( 'NONE', *, *, #45266, .T. ) ;
#34760 = CARTESIAN_POINT ( 'NONE',  ( -42.62287095715006302, -24.51387760970723662, 9.387446482453421837 ) ) ;
#34761 = CARTESIAN_POINT ( 'NONE',  ( -3.561414601982806349, 22.15502443119318343, -1.500000000000002220 ) ) ;
#34762 = VERTEX_POINT ( 'NONE', #83995 ) ;
#34763 = DIRECTION ( 'NONE',  ( -0.000000000000000000, 1.000000000000000000, -0.000000000000000000 ) ) ;
#34764 = CARTESIAN_POINT ( 'NONE',  ( -0.02075734969026423599, 5.965225279485572685, -0.08597719988137648983 ) ) ;
#34765 = CARTESIAN_POINT ( 'NONE',  ( 8.720390671794367776, 5.356774720513354460, -27.07197491334870065 ) ) ;
#34766 = EDGE_CURVE ( 'NONE', #11431, #14117, #45455, .T. ) ;
#34767 = EDGE_CURVE ( 'NONE', #36722, #66916, #756, .T. ) ;
#34768 = CARTESIAN_POINT ( 'NONE',  ( -125.5228709571500900, -24.15431212366837244, -0.2830839119329186526 ) ) ;
#34769 = EDGE_CURVE ( 'NONE', #2264, #81363, #6872, .T. ) ;
#34770 = B_SPLINE_CURVE_WITH_KNOTS ( 'NONE', 3,
 ( #59386, #51777, #44661, #5591, #74599, #43172 ),
 .UNSPECIFIED., .F., .F.,
 ( 4, 2, 4 ),
 ( 0.000000000000000000, 0.001380901958385382473, 0.002761803916770764946 ),
 .UNSPECIFIED. ) ;
#34771 = CARTESIAN_POINT ( 'NONE',  ( -97.25161593912366698, -24.37907397113049868, 9.703205396196697308 ) ) ;
#34772 = CARTESIAN_POINT ( 'NONE',  ( 10.47639735327893362, 16.54961352017854637, -1.500000000000002220 ) ) ;
#34773 = DIRECTION ( 'NONE',  ( 1.000000000000000000, 3.491481338843133355E-15, 2.352173255807796056E-16 ) ) ;
#34775 = EDGE_CURVE ( 'NONE', #55675, #17192, #12614, .T. ) ;
#34774 = ORIENTED_EDGE ( 'NONE', *, *, #48148, .F. ) ;
#34776 = AXIS2_PLACEMENT_3D ( 'NONE', #35901, #88203, #89199 ) ;
#34777 = CARTESIAN_POINT ( 'NONE',  ( 13.04721882220160012, 17.14300067834640373, 11.49999999999998934 ) ) ;
#34778 = CARTESIAN_POINT ( 'NONE',  ( -128.5553793226067398, -24.65952944569305316, 1.056160979905708341 ) ) ;
#34779 = CARTESIAN_POINT ( 'NONE',  ( -71.30457154551153565, -25.12218950775439197, 6.209207676158021272 ) ) ;
#34780 = DIRECTION ( 'NONE',  ( 0.000000000000000000, 0.000000000000000000, -1.000000000000000000 ) ) ;
#34781 = DIRECTION ( 'NONE',  ( 1.000000000000000000, 0.000000000000000000, 0.000000000000000000 ) ) ;
#34782 = CARTESIAN_POINT ( 'NONE',  ( -22.77861398648627400, -3.026084143414268013, -1.500000000000002220 ) ) ;
#34783 = PERSON_AND_ORGANIZATION_ROLE ( 'design_supplier' ) ;
#34784 = DIRECTION ( 'NONE',  ( 1.611864046919725738E-15, -7.253388211138766116E-15, 1.000000000000000000 ) ) ;
#34785 = CARTESIAN_POINT ( 'NONE',  ( -49.65271201290308767, -23.73766607897670156, -1.055555164236457344 ) ) ;
#34786 = CARTESIAN_POINT ( 'NONE',  ( -0.3114230556345199963, -20.10660241673355486, 11.49999999999999645 ) ) ;
#34787 = CARTESIAN_POINT ( 'NONE',  ( -68.62287095715005592, -23.47596703998600631, 11.44779298504227505 ) ) ;
#34788 = CARTESIAN_POINT ( 'NONE',  ( -32.58669467011947773, -24.35071581493542681, 9.817618358456035921 ) ) ;
#34789 = B_SPLINE_CURVE_WITH_KNOTS ( 'NONE', 3,
 ( #24225, #72420, #33843, #48079, #86127, #79005 ),
 .UNSPECIFIED., .F., .F.,
 ( 4, 2, 4 ),
 ( 0.000000000000000000, 0.001380901958385387894, 0.002761803916770775788 ),
 .UNSPECIFIED. ) ;
#34790 = DIRECTION ( 'NONE',  ( -0.000000000000000000, 2.173523156925979552E-06, -0.9999999999976378895 ) ) ;
#34791 = FACE_OUTER_BOUND ( 'NONE', #62137, .T. ) ;
#34792 = FACE_OUTER_BOUND ( 'NONE', #14825, .T. ) ;
#34793 = ADVANCED_FACE ( 'NONE', ( #68779 ), #25487, .T. ) ;
#34795 = ADVANCED_FACE ( 'NONE', ( #17481 ), #1271, .T. ) ;
#34794 = CARTESIAN_POINT ( 'NONE',  ( -19.08307359429613825, -5.530936995296134917, 11.49999999999998934 ) ) ;
#34796 = LINE ( 'NONE', #96681, #28543 ) ;
#34797 = CARTESIAN_POINT ( 'NONE',  ( -17.00503767097633556, -9.977476526402845991, -1.500000000000002220 ) ) ;
#34798 = DIRECTION ( 'NONE',  ( 0.000000000000000000, 0.000000000000000000, -1.000000000000000000 ) ) ;
#34799 = DATE_TIME_ROLE ( 'classification_date' ) ;
#34800 = UNCERTAINTY_MEASURE_WITH_UNIT (LENGTH_MEASURE( 1.000000000000000082E-05 ), #79474, 'distance_accuracy_value', 'NONE');
#34801 = CARTESIAN_POINT ( 'NONE',  ( -115.6228709571500559, -24.82558206586148586, 1.605769216559630230 ) ) ;
#34802 = CARTESIAN_POINT ( 'NONE',  ( -79.52287095715007581, -23.72773821059536914, 11.05748984161097503 ) ) ;
#34803 = CARTESIAN_POINT ( 'NONE',  ( -19.87711886888390822, 5.503898473480427711, 11.49999999999999645 ) ) ;
#34804 = EDGE_CURVE ( 'NONE', #2526, #29468, #25918, .T. ) ;
#34805 = DIRECTION ( 'NONE',  ( 1.000000000000000000, 1.734723475976806848E-16, 0.000000000000000000 ) ) ;
#34806 = CARTESIAN_POINT ( 'NONE',  ( -4.753580043990282888, 22.13494492317406070, 11.49999999999999645 ) ) ;
#34807 = ORIENTED_EDGE ( 'NONE', *, *, #8741, .T. ) ;
#34808 = CARTESIAN_POINT ( 'NONE',  ( 17.91726403014145319, 0.000000000000000000, -1.691563534834430227 ) ) ;
#34809 = CARTESIAN_POINT ( 'NONE',  ( -51.29687923781919068, -25.27367468601215350, 3.993462154588707680 ) ) ;
#34810 = CARTESIAN_POINT ( 'NONE',  ( -127.5228709571500616, -24.33927499327856125, 9.819080762295806508 ) ) ;
#34811 = ADVANCED_FACE ( 'NONE', ( #24585 ), #87497, .F. ) ;
#34812 = VECTOR ( 'NONE', #67429, 1000.000000000000000 ) ;
#34813 = DIRECTION ( 'NONE',  ( 0.000000000000000000, -2.173523156925979552E-06, 0.9999999999976378895 ) ) ;
#34814 = ORIENTED_EDGE ( 'NONE', *, *, #21239, .F. ) ;
#34815 = EDGE_CURVE ( 'NONE', #81032, #78995, #2276, .T. ) ;
#34816 = ORIENTED_EDGE ( 'NONE', *, *, #11884, .T. ) ;
#34817 = CARTESIAN_POINT ( 'NONE',  ( 0.3791100739519297491, -6.376774720514418959, 20.35309744218306349 ) ) ;
#34818 = CARTESIAN_POINT ( 'NONE',  ( 13.72848742581335912, -18.28091200367991576, -1.500000000000002220 ) ) ;
#34820 = EDGE_CURVE ( 'NONE', #86130, #55078, #33205, .T. ) ;
#34819 = DIRECTION ( 'NONE',  ( -0.000000000000000000, 1.000000000000000000, -0.000000000000000000 ) ) ;
#34821 = PLANE ( 'NONE',  #28551 ) ;
#34822 = CARTESIAN_POINT ( 'NONE',  ( -76.55620429048342146, -23.48786465467241058, 11.44779295918254469 ) ) ;
#34823 = CARTESIAN_POINT ( 'NONE',  ( -18.84819291449097278, 12.34854029719970825, 11.49999999999999645 ) ) ;
#34824 = ORIENTED_EDGE ( 'NONE', *, *, #15429, .T. ) ;
#34825 = CARTESIAN_POINT ( 'NONE',  ( -43.58152581000473447, -24.51314013834316086, 0.6176544820404145097 ) ) ;
#34826 = B_SPLINE_CURVE_WITH_KNOTS ( 'NONE', 3,
 ( #74942, #92174, #30782, #21652, #30273, #69346 ),
 .UNSPECIFIED., .F., .F.,
 ( 4, 2, 4 ),
 ( 0.000000000000000000, 0.001380764517853253371, 0.002761529035706506742 ),
 .UNSPECIFIED. ) ;
#34827 = CARTESIAN_POINT ( 'NONE',  ( -8.471812324360341151, -20.26817064352238162, 11.49999999999998934 ) ) ;
#34828 = CARTESIAN_POINT ( 'NONE',  ( -92.62287095715005592, -29.50250243563736774, 8.947779886222139822 ) ) ;
#34829 = CARTESIAN_POINT ( 'NONE',  ( -29.21998272650427708, -25.21724568626827079, 5.646413213696420463 ) ) ;
#34830 = ORIENTED_EDGE ( 'NONE', *, *, #65447, .T. ) ;
#34831 = EDGE_CURVE ( 'NONE', #40253, #45491, #48946, .T. ) ;
#34832 = CARTESIAN_POINT ( 'NONE',  ( -63.62287095715006302, -24.50321055353805377, 9.387540953477527594 ) ) ;
#34833 = FACE_OUTER_BOUND ( 'NONE', #64451, .T. ) ;
#34834 = ORIENTED_EDGE ( 'NONE', *, *, #39150, .T. ) ;
#34835 = CARTESIAN_POINT ( 'NONE',  ( -49.55620429048339304, -23.48786465467241058, 11.44779295918254647 ) ) ;
#34836 = CARTESIAN_POINT ( 'NONE',  ( -11.60840874443078263, -16.91462557209307960, -1.500000000000002220 ) ) ;
#34837 = ORIENTED_EDGE ( 'NONE', *, *, #81448, .F. ) ;
#34838 = VERTEX_POINT ( 'NONE', #10368 ) ;
#34839 = ORIENTED_EDGE ( 'NONE', *, *, #39671, .T. ) ;
#34840 = DIRECTION ( 'NONE',  ( -0.000000000000000000, -1.000000000000000000, -0.000000000000000000 ) ) ;
#34841 = CARTESIAN_POINT ( 'NONE',  ( 11.75533340255842596, 19.88161105567325038, 11.49999999999998934 ) ) ;
#34842 = CARTESIAN_POINT ( 'NONE',  ( -41.52287095715008292, -24.51387760970724372, 9.387446482453407626 ) ) ;
#34843 = CARTESIAN_POINT ( 'NONE',  ( 8.194921280291850962, -18.63391395107102610, -1.500000000000002220 ) ) ;
#34844 = ORIENTED_EDGE ( 'NONE', *, *, #86852, .F. ) ;
#34845 = CARTESIAN_POINT ( 'NONE',  ( -20.27875734969026311, 7.743225279485574042, 24.00402280011862288 ) ) ;
#34846 = CARTESIAN_POINT ( 'NONE',  ( -29.53070056818989286, -24.43102165026504835, 9.386484716961749797 ) ) ;
#34847 = CARTESIAN_POINT ( 'NONE',  ( -105.6293832185014026, -24.40034930558991277, 0.3402023900116059041 ) ) ;
#34848 = CARTESIAN_POINT ( 'NONE',  ( -71.18291627536595456, -25.03149790695943366, 7.291244984715597788 ) ) ;
#34849 = ORIENTED_EDGE ( 'NONE', *, *, #1196, .F. ) ;
#34850 = CARTESIAN_POINT ( 'NONE',  ( 282.9764569301858046, 6.475225279485573360, 20.79159422840526616 ) ) ;
#34851 = DIRECTION ( 'NONE',  ( -1.000000000000000000, -3.773278334444166432E-23, -8.201307841325785021E-29 ) ) ;
#34852 = AXIS2_PLACEMENT_3D ( 'NONE', #48901, #58513, #26559 ) ;
#34853 = VERTEX_POINT ( 'NONE', #80385 ) ;
#34854 = CARTESIAN_POINT ( 'NONE',  ( -9.565632364391108311, -18.43008791299702764, 11.49999999999998934 ) ) ;
#34855 = VERTEX_POINT ( 'NONE', #16976 ) ;
#34857 = ORIENTED_EDGE ( 'NONE', *, *, #1144, .F. ) ;
#34856 = CARTESIAN_POINT ( 'NONE',  ( -39.93825361760627857, -25.30561201263888194, 4.984140935953358387 ) ) ;
#34858 = DIRECTION ( 'NONE',  ( 0.000000000000000000, 0.000000000000000000, -1.000000000000000000 ) ) ;
#34859 = CARTESIAN_POINT ( 'NONE',  ( -51.92991590564532345, -25.25550010977676507, 6.106957726396983865 ) ) ;
#34860 = ORIENTED_EDGE ( 'NONE', *, *, #91804, .F. ) ;
#34861 = VERTEX_POINT ( 'NONE', #47942 ) ;
#34862 = CARTESIAN_POINT ( 'NONE',  ( -88.62287095715004170, -24.65952944569304606, 1.056160979905700570 ) ) ;
#34863 =( BOUNDED_SURFACE ( )  B_SPLINE_SURFACE ( 3, 2, ( 
 ( #73362, #96685, #72366 ),
 ( #80466, #40904, #19558 ),
 ( #17566, #27187, #25676 ),
 ( #4354, #95692, #2862 ) ),
 .UNSPECIFIED., .F., .F., .T. ) 
 B_SPLINE_SURFACE_WITH_KNOTS ( ( 4, 4 ),
 ( 3, 3 ),
 ( 0.0009756167707891351057, 0.001181474220861217402 ),
 ( 0.000000000000000000, 1.000000000000000000 ),
 .UNSPECIFIED. ) 
 GEOMETRIC_REPRESENTATION_ITEM ( )  RATIONAL_B_SPLINE_SURFACE ( (
 ( 1.000000000000000000, 0.8117984224361689538, 1.000000000000000000),
 ( 1.000000000000000000, 0.7811245729408042848, 1.000000000000000000),
 ( 1.000000000000000000, 0.7458076110977214235, 1.000000000000000000),
 ( 1.000000000000000000, 0.7071067811865522357, 1.000000000000000000) ) ) 
 REPRESENTATION_ITEM ( '' )  SURFACE ( )  );
#34864 = CARTESIAN_POINT ( 'NONE',  ( 8.667033081675079131, 3.316774720514425567, -27.07192531862967400 ) ) ;
#34865 = PLANE ( 'NONE',  #46961 ) ;
#34866 = CARTESIAN_POINT ( 'NONE',  ( -43.53991149891938761, -24.35071581493542681, 9.817618358456032368 ) ) ;
#34868 = ORIENTED_EDGE ( 'NONE', *, *, #53572, .F. ) ;
#34867 = CARTESIAN_POINT ( 'NONE',  ( 15.76968270297436625, 15.47746201419723100, 11.49999999999999645 ) ) ;
#34869 = CARTESIAN_POINT ( 'NONE',  ( -103.5550949855981031, -23.96119346886881019, -0.6495511937832079141 ) ) ;
#34870 = CARTESIAN_POINT ( 'NONE',  ( 15.43685675143394498, -16.52047792065556564, -1.500000000000002220 ) ) ;
#34872 = ORIENTED_EDGE ( 'NONE', *, *, #52923, .T. ) ;
#34871 = CARTESIAN_POINT ( 'NONE',  ( -115.5877643602478884, -24.83644354573579349, 8.397322867130093016 ) ) ;
#34873 = ORIENTED_EDGE ( 'NONE', *, *, #88092, .T. ) ;
#34874 = CARTESIAN_POINT ( 'NONE',  ( -75.62287095715005592, -25.00158670708909625, 2.256160236439166855 ) ) ;
#34875 = AXIS2_PLACEMENT_3D ( 'NONE', #62243, #69848, #1342 ) ;
#34876 = ADVANCED_FACE ( 'NONE', ( #10875 ), #78863, .F. ) ;
#34877 = FACE_OUTER_BOUND ( 'NONE', #1980, .T. ) ;
#34878 = VERTEX_POINT ( 'NONE', #9868 ) ;
#34879 = CARTESIAN_POINT ( 'NONE',  ( -21.01389645921736360, -2.595061309317715281, 11.49999999999998934 ) ) ;
#34880 = EDGE_CURVE ( 'NONE', #63208, #76713, #25085, .T. ) ;
#34881 = CARTESIAN_POINT ( 'NONE',  ( -7.131053040288445999, -5.876774720514413630, 19.60308799987318196 ) ) ;
#34882 = LINE ( 'NONE', #88175, #21073 ) ;
#34883 = CARTESIAN_POINT ( 'NONE',  ( -0.5504121640580519337, 22.28327991085032878, -1.500000000000002220 ) ) ;
#34884 = EDGE_CURVE ( 'NONE', #23558, #88974, #63240, .T. ) ;
#34885 = CARTESIAN_POINT ( 'NONE',  ( -46.62287095715004881, -24.64898659630528499, 1.056161002820821038 ) ) ;
#34886 = VECTOR ( 'NONE', #73430, 1000.000000000000114 ) ;
#34887 = EDGE_CURVE ( 'NONE', #21668, #5151, #86989, .T. ) ;
#34888 = ORIENTED_EDGE ( 'NONE', *, *, #74682, .F. ) ;
#34889 = CARTESIAN_POINT ( 'NONE',  ( -52.52287095715006870, -29.50247984919015209, -1.443849546365058689 ) ) ;
#34890 = DIRECTION ( 'NONE',  ( 0.000000000000000000, 0.000000000000000000, 1.000000000000000000 ) ) ;
#34891 = EDGE_CURVE ( 'NONE', #16731, #20987, #82873, .T. ) ;
#34892 = AXIS2_PLACEMENT_3D ( 'NONE', #66800, #97721, #28212 ) ;
#34893 = EDGE_CURVE ( 'NONE', #16636, #2918, #95677, .T. ) ;
#34894 = CARTESIAN_POINT ( 'NONE',  ( -71.58953762381672448, -23.48783264082478084, -1.443836473390067487 ) ) ;
#34895 = DIRECTION ( 'NONE',  ( -0.8246584009594635223, 0.5656310827093757876, 1.065814103640150279E-14 ) ) ;
#34896 = CARTESIAN_POINT ( 'NONE',  ( -16.58133674543539371, -10.29093563426468450, -1.500000000000002220 ) ) ;
#34897 = CARTESIAN_POINT ( 'NONE',  ( 14.45597713831175035, -15.85640774750547344, -1.500000000000002220 ) ) ;
#34898 = CARTESIAN_POINT ( 'NONE',  ( -27.55569643375672584, -24.92774666922491278, 1.631373448212198429 ) ) ;
#34899 = CARTESIAN_POINT ( 'NONE',  ( -51.57779606109421877, -24.65952944569304250, 1.056160979905695463 ) ) ;
#34900 = CARTESIAN_POINT ( 'NONE',  ( 0.000000000000000000, -1.473225279485573802, 3.500000000000000000 ) ) ;
#34901 = CARTESIAN_POINT ( 'NONE',  ( 22.20583189720066741, -5.198064566299082756, -1.500000000000002220 ) ) ;
#34902 = CARTESIAN_POINT ( 'NONE',  ( 0.000000000000000000, -12.95045055897114494, 1.734723475976807094E-15 ) ) ;
#34903 = CARTESIAN_POINT ( 'NONE',  ( -102.5529430821646173, -24.15543982623908192, -0.2315651400026460249 ) ) ;
#34904 = CARTESIAN_POINT ( 'NONE',  ( -128.5228709571501042, -23.72747288104470442, -1.053458166803224572 ) ) ;
#34905 = CARTESIAN_POINT ( 'NONE',  ( 17.47191945374660094, 9.613082372698542599, 11.49999999999999645 ) ) ;
#34906 = FACE_OUTER_BOUND ( 'NONE', #78903, .T. ) ;
#34907 = CARTESIAN_POINT ( 'NONE',  ( -39.65634080071149015, -23.73791477778911485, 11.05961554403170943 ) ) ;
#34908 = CARTESIAN_POINT ( 'NONE',  ( 0.1553305729023591875, -1.423459158329792640, 2.407412430484044816E-32 ) ) ;
#34909 = ORIENTED_EDGE ( 'NONE', *, *, #46246, .F. ) ;
#34910 = DIRECTION ( 'NONE',  ( 1.000000000000000000, 0.000000000000000000, 0.000000000000000000 ) ) ;
#34911 = EDGE_CURVE ( 'NONE', #94949, #26877, #63504, .T. ) ;
#34912 = LINE ( 'NONE', #50143, #60497 ) ;
#34913 = CARTESIAN_POINT ( 'NONE',  ( 14.13103794885040898, -16.47871000921984219, 11.49999999999998934 ) ) ;
#34914 = CARTESIAN_POINT ( 'NONE',  ( -93.58953762381673869, -24.65952944569305316, 1.056160979905705011 ) ) ;
#34915 = CARTESIAN_POINT ( 'NONE',  ( -18.05301863641116000, -7.546005365994440162, -1.500000000000002220 ) ) ;
#34916 = CARTESIAN_POINT ( 'NONE',  ( -8.160000000000000142, 8.793627758918228565, -2.994553991265763049 ) ) ;
#34917 = EDGE_CURVE ( 'NONE', #14136, #58437, #6684, .T. ) ;
#34918 = DATE_AND_TIME ( #26804, #58753 ) ;
#34919 = AXIS2_PLACEMENT_3D ( 'NONE', #17956, #35682, #48917 ) ;
#34920 = DIRECTION ( 'NONE',  ( 0.000000000000000000, 0.000000000000000000, -1.000000000000000000 ) ) ;
#34921 = CARTESIAN_POINT ( 'NONE',  ( -20.42006937447004233, 0.3101567295262241952, 11.49999999999999645 ) ) ;
#34922 = CARTESIAN_POINT ( 'NONE',  ( -27.61845239340658154, 0.3587747205144057872, -10.37513603161905706 ) ) ;
#34923 = CARTESIAN_POINT ( 'NONE',  ( -61.59189125704995860, -25.07259839747099051, 7.371166918563575976 ) ) ;
#34924 = EDGE_LOOP ( 'NONE', ( #25119, #49102, #71784, #64224 ) ) ;
#34925 = CARTESIAN_POINT ( 'NONE',  ( -127.5228709571500616, -29.50248528299804818, 1.056150453629047137 ) ) ;
#34926 = CARTESIAN_POINT ( 'NONE',  ( -34.62287095715005592, -24.65952944569303895, 1.056160979905691688 ) ) ;
#34927 = CARTESIAN_POINT ( 'NONE',  ( -116.5158230194428342, -24.66019654487199730, 8.947790411086115725 ) ) ;
#34928 = CARTESIAN_POINT ( 'NONE',  ( -31.52166505407126706, -24.87479601683088148, 8.247789944647562876 ) ) ;
#34929 = ORIENTED_EDGE ( 'NONE', *, *, #84709, .T. ) ;
#34930 = CARTESIAN_POINT ( 'NONE',  ( 6.431189903846153300, -6.376774720514415407, 20.08974358974358765 ) ) ;
#34931 = EDGE_CURVE ( 'NONE', #27382, #12529, #19973, .T. ) ;
#34932 = CARTESIAN_POINT ( 'NONE',  ( 3.792298468851710069, -22.70151372599487871, 11.49999999999999645 ) ) ;
#34933 = CARTESIAN_POINT ( 'NONE',  ( -6.081610112697643622, 21.96313418072945822, 11.49999999999998934 ) ) ;
#34934 = CARTESIAN_POINT ( 'NONE',  ( -110.6248242805079656, -24.83644354573579349, 8.397322867130096569 ) ) ;
#34935 = CARTESIAN_POINT ( 'NONE',  ( 30.45304879119406039, 1.477225279485574028, -10.07140455160086390 ) ) ;
#34936 = CARTESIAN_POINT ( 'NONE',  ( -25.92875734969025814, -3.316774720514426456, 24.50402280011861933 ) ) ;
#34937 = CARTESIAN_POINT ( 'NONE',  ( -52.92287095715007439, -23.47593901973090169, -1.443836447538997980 ) ) ;
#34938 = CARTESIAN_POINT ( 'NONE',  ( -110.6352815603598572, -23.48783264082476663, -1.443836473390091690 ) ) ;
#34939 = EDGE_CURVE ( 'NONE', #40450, #5350, #4760, .T. ) ;
#34940 = CARTESIAN_POINT ( 'NONE',  ( -8.129759772327192380, 20.32010563749377141, 11.49999999999998934 ) ) ;
#34941 = CYLINDRICAL_SURFACE ( 'NONE', #25154, 1.000000000000000000 ) ;
#34942 = CIRCLE ( 'NONE', #52764, 1.050000000000000488 ) ;
#34943 = CARTESIAN_POINT ( 'NONE',  ( 8.978253834636468866, -5.876774720514426953, 18.51871304725684553 ) ) ;
#34944 = DIRECTION ( 'NONE',  ( -0.000000000000000000, 1.000000000000000000, -0.000000000000000000 ) ) ;
#34945 = CARTESIAN_POINT ( 'NONE',  ( -96.52287095715010423, -23.95044443724993144, 10.65354141964648882 ) ) ;
#34946 = ORIENTED_EDGE ( 'NONE', *, *, #2880, .T. ) ;
#34947 = CARTESIAN_POINT ( 'NONE',  ( -19.05221060042639536, -7.346018566486852031, -1.500000000000002220 ) ) ;
#34948 = ORIENTED_EDGE ( 'NONE', *, *, #44720, .F. ) ;
#34949 = CIRCLE ( 'NONE', #30074, 2.040000000000000036 ) ;
#34950 = ORIENTED_EDGE ( 'NONE', *, *, #92034, .T. ) ;
#34951 = ORIENTED_EDGE ( 'NONE', *, *, #53735, .T. ) ;
#34952 = VERTEX_POINT ( 'NONE', #36703 ) ;
#34953 = CARTESIAN_POINT ( 'NONE',  ( 20.85440106035463970, 9.703512019146668166, -1.500000000000002220 ) ) ;
#34954 = LINE ( 'NONE', #20211, #55147 ) ;
#34955 = CARTESIAN_POINT ( 'NONE',  ( 2.654622155064554789, -19.98241913370796041, -1.500000000000002220 ) ) ;
#34956 = AXIS2_PLACEMENT_3D ( 'NONE', #63105, #78793, #2209 ) ;
#34957 = ORIENTED_EDGE ( 'NONE', *, *, #60394, .F. ) ;
#34958 = DIRECTION ( 'NONE',  ( 0.000000000000000000, -2.173523156925979552E-06, 0.9999999999976378895 ) ) ;
#34959 = CARTESIAN_POINT ( 'NONE',  ( -9.940598223437573822, -5.876774720514426953, 18.21871304725684837 ) ) ;
#34960 = AXIS2_PLACEMENT_3D ( 'NONE', #84711, #31936, #68994 ) ;
#34961 = B_SPLINE_CURVE_WITH_KNOTS ( 'NONE', 3,
 ( #88582, #41405, #89077, #51020, #12440, #79957 ),
 .UNSPECIFIED., .F., .F.,
 ( 4, 2, 4 ),
 ( 0.000000000000000000, 0.001380901958385387894, 0.002761803916770775788 ),
 .UNSPECIFIED. ) ;
#34962 = CARTESIAN_POINT ( 'NONE',  ( -95.63008670059350891, -24.52300882791530512, 0.6510814631126408125 ) ) ;
#34963 = DIRECTION ( 'NONE',  ( 0.000000000000000000, 1.000000000000000000, 0.000000000000000000 ) ) ;
#34965 = ORIENTED_EDGE ( 'NONE', *, *, #5093, .T. ) ;
#34964 = CARTESIAN_POINT ( 'NONE',  ( -14.55006661338671847, 15.66751491618662406, 11.49999999999999645 ) ) ;
#34966 = LINE ( 'NONE', #5010, #80848 ) ;
#34967 = ORIENTED_EDGE ( 'NONE', *, *, #50409, .T. ) ;
#34968 = CARTESIAN_POINT ( 'NONE',  ( 21.95989154999629278, -3.605859658025859282, 11.49999999999998934 ) ) ;
#34969 = CARTESIAN_POINT ( 'NONE',  ( 18.27903665858761073, 9.701928907310005457, -1.500000000000002220 ) ) ;
#34970 = ORIENTED_EDGE ( 'NONE', *, *, #69635, .F. ) ;
#34971 = B_SPLINE_CURVE_WITH_KNOTS ( 'NONE', 3,
 ( #7081, #14182, #82705, #61385 ),
 .UNSPECIFIED., .F., .F.,
 ( 4, 4 ),
 ( 0.000000000000000000, 9.999999999998897304E-05 ),
 .UNSPECIFIED. ) ;
#34972 = CARTESIAN_POINT ( 'NONE',  ( -71.72619204561506479, -25.20650855361216713, 6.812664954086296021 ) ) ;
#34973 = VERTEX_POINT ( 'NONE', #20465 ) ;
#34974 = CARTESIAN_POINT ( 'NONE',  ( -13.89275734969026388, -5.965225279485572685, 31.02402280011862246 ) ) ;
#34975 = ORIENTED_EDGE ( 'NONE', *, *, #56534, .F. ) ;
#34976 = CARTESIAN_POINT ( 'NONE',  ( 5.851028665930490646, 6.475225279485576024, -27.43979700150094558 ) ) ;
#34977 = CARTESIAN_POINT ( 'NONE',  ( -20.86263692406621928, 1.606387762444034362, -1.500000000000002220 ) ) ;
#34978 = CARTESIAN_POINT ( 'NONE',  ( 4.863445656156933694, -21.36585520573490626, 11.49999999999999645 ) ) ;
#34979 = CARTESIAN_POINT ( 'NONE',  ( -26.50032570333037185, -24.89279848742383194, 6.891654722310369685 ) ) ;
#34980 = CARTESIAN_POINT ( 'NONE',  ( -15.68175098440391402, -16.16561365185589594, 11.49999999999998934 ) ) ;
#34981 = CARTESIAN_POINT ( 'NONE',  ( -2.368302597431856782, 20.80102113048726409, -1.500000000000002220 ) ) ;
#34982 = DIRECTION ( 'NONE',  ( 1.000000000000000000, 3.773278334444166432E-23, 8.201307841325785021E-29 ) ) ;
#34983 = FACE_OUTER_BOUND ( 'NONE', #7906, .T. ) ;
#34984 = CARTESIAN_POINT ( 'NONE',  ( -72.62287095715005592, -23.47593901973091235, -1.443836447539006196 ) ) ;
#34985 = CARTESIAN_POINT ( 'NONE',  ( -126.5895376238167529, -24.66019654487199375, 8.947790411086124607 ) ) ;
#34986 = ORIENTED_EDGE ( 'NONE', *, *, #47750, .F. ) ;
#34987 = ORIENTED_EDGE ( 'NONE', *, *, #54019, .T. ) ;
#34988 = VERTEX_POINT ( 'NONE', #28588 ) ;
#34989 = CARTESIAN_POINT ( 'NONE',  ( -52.64484739509910582, -23.96119346886881019, -0.6495511937831939253 ) ) ;
#34990 = ORIENTED_EDGE ( 'NONE', *, *, #79863, .T. ) ;
#34991 = CARTESIAN_POINT ( 'NONE',  ( 19.99082695160776169, -7.785253749782737209, -1.500000000000002220 ) ) ;
#34992 = EDGE_CURVE ( 'NONE', #64204, #32607, #72947, .T. ) ;
#34993 = FACE_OUTER_BOUND ( 'NONE', #56854, .T. ) ;
#34994 = VERTEX_POINT ( 'NONE', #12853 ) ;
#34995 = CARTESIAN_POINT ( 'NONE',  ( 17.90021246794804810, -11.17811638239879279, 11.49999999999998934 ) ) ;
#34996 = CARTESIAN_POINT ( 'NONE',  ( -69.86226356453386188, -25.11033435731149055, 2.832404375966413479 ) ) ;
#34997 = EDGE_CURVE ( 'NONE', #79255, #937, #65847, .T. ) ;
#34998 = CARTESIAN_POINT ( 'NONE',  ( -71.62287095715005592, -29.50250243563736774, 8.947779886222143375 ) ) ;
#34999 = CARTESIAN_POINT ( 'NONE',  ( -121.5228709571500190, -24.66019654487199730, 8.947790411086119278 ) ) ;
#35000 = CARTESIAN_POINT ( 'NONE',  ( -80.48373552459977986, -25.29534346072172823, 4.508937073655467032 ) ) ;
#35001 = CARTESIAN_POINT ( 'NONE',  ( -129.5896970873678242, -24.35071581493544457, 9.817618358456021710 ) ) ;
#35002 = CARTESIAN_POINT ( 'NONE',  ( 2.710298230372018669, -21.94706154713207980, -1.500000000000002220 ) ) ;
#35003 = ORIENTED_EDGE ( 'NONE', *, *, #40279, .T. ) ;
#35004 = CARTESIAN_POINT ( 'NONE',  ( -81.62948795153646131, -24.35071581493543391, 9.817618358456037697 ) ) ;
#35005 = ADVANCED_FACE ( 'NONE', ( #51437 ), #11864, .F. ) ;
#35006 = CARTESIAN_POINT ( 'NONE',  ( 9.071512145086499501, -1.000000000000000000, 7.567128810856562637 ) ) ;
#35007 = CARTESIAN_POINT ( 'NONE',  ( -41.71489324084514294, -25.27955919863082812, 4.846374523598886874 ) ) ;
#35008 = EDGE_CURVE ( 'NONE', #38489, #60035, #60057, .T. ) ;
#35009 = CIRCLE ( 'NONE', #47979, 1.249999999999996003 ) ;
#35010 = FACE_OUTER_BOUND ( 'NONE', #18239, .T. ) ;
#35011 = B_SPLINE_CURVE_WITH_KNOTS ( 'NONE', 3,
 ( #8879, #84571, #93683, #69356, #86576, #24665, #16054, #100272, #22658, #85572, #92183, #47026, #39404, #15559 ),
 .UNSPECIFIED., .F., .F.,
 ( 4, 2, 2, 2, 2, 2, 4 ),
 ( 0.000000000000000000, 0.0001867446169474697279, 0.0003734892338949394558, 0.0007469784677898988609, 0.001120467701684858212, 0.001307212318632341519, 0.001493956935579824827 ),
 .UNSPECIFIED. ) ;
#35012 = EDGE_CURVE ( 'NONE', #80512, #62158, #43821, .T. ) ;
#35013 = CARTESIAN_POINT ( 'NONE',  ( -47.58953762381672448, -24.64898659630367916, 1.056161002820380279 ) ) ;
#35014 = CARTESIAN_POINT ( 'NONE',  ( -13.85510387911049079, -16.26762222697724880, -1.500000000000002220 ) ) ;
#35015 = CARTESIAN_POINT ( 'NONE',  ( 10.34999999999999254, 2.239999999999996216, 2.100000000000000977 ) ) ;
#35016 = EDGE_CURVE ( 'NONE', #22424, #65090, #75500, .T. ) ;
#35017 = B_SPLINE_CURVE_WITH_KNOTS ( 'NONE', 3,
 ( #1541, #18257, #87775, #95879 ),
 .UNSPECIFIED., .F., .F.,
 ( 4, 4 ),
 ( 0.000000000000000000, 9.999999999998206125E-05 ),
 .UNSPECIFIED. ) ;
#35018 = FACE_OUTER_BOUND ( 'NONE', #2903, .T. ) ;
#35019 = B_SPLINE_CURVE_WITH_KNOTS ( 'NONE', 3,
 ( #23131, #16524, #30762, #94153 ),
 .UNSPECIFIED., .F., .F.,
 ( 4, 4 ),
 ( 1.734723475976806902E-18, 0.002763707449907618768 ),
 .UNSPECIFIED. ) ;
#35020 = CARTESIAN_POINT ( 'NONE',  ( -64.56596816803553907, -23.48786465467241058, 11.44779295918254824 ) ) ;
#35021 = CARTESIAN_POINT ( 'NONE',  ( -80.48900664166535535, -25.12298712672050982, 7.101635559041870494 ) ) ;
#35022 = CARTESIAN_POINT ( 'NONE',  ( 15.50834587592193259, -16.38432980155966590, -1.500000000000002220 ) ) ;
#35023 = AXIS2_PLACEMENT_3D ( 'NONE', #65792, #89108, #35325 ) ;
#35024 = DIRECTION ( 'NONE',  ( -0.5656310827093756766, -2.995395837334948290E-15, 0.8246584009594636333 ) ) ;
#35025 = VERTEX_POINT ( 'NONE', #12357 ) ;
#35026 = CIRCLE ( 'NONE', #91714, 18.35000000000000142 ) ;
#35027 = LINE ( 'NONE', #18786, #38476 ) ;
#35028 = CARTESIAN_POINT ( 'NONE',  ( -79.58202583663157270, -24.65952944569304606, 1.056160979905701902 ) ) ;
#35029 = CARTESIAN_POINT ( 'NONE',  ( -18.83419513347712737, -5.836681878196540829, 11.49999999999999645 ) ) ;
#35030 = LINE ( 'NONE', #44137, #61804 ) ;
#35031 = AXIS2_PLACEMENT_3D ( 'NONE', #71723, #87944, #2218 ) ;
#35032 = CARTESIAN_POINT ( 'NONE',  ( -67.62364343387676513, -24.65952944569304961, 1.056160979905700570 ) ) ;
#35033 = VERTEX_POINT ( 'NONE', #98589 ) ;
#35034 = AXIS2_PLACEMENT_3D ( 'NONE', #72598, #72102, #49769 ) ;
#35035 = CARTESIAN_POINT ( 'NONE',  ( 1.949999999999999956, -0.1925000000000001155, -0.1925000000000000600 ) ) ;
#35036 = CARTESIAN_POINT ( 'NONE',  ( -29.31644179857717347, -24.60094090469272743, 2.549175303124721292 ) ) ;
#35037 = CARTESIAN_POINT ( 'NONE',  ( -101.0369185477202336, -25.12268536277769471, 6.965963272030491815 ) ) ;
#35038 = CARTESIAN_POINT ( 'NONE',  ( -18.67883320684159543, -10.89015303950203517, 11.49999999999998934 ) ) ;
#35039 = CARTESIAN_POINT ( 'NONE',  ( -126.6228709571499991, -24.33927499327855415, 9.819080762295802955 ) ) ;
#35041 = CARTESIAN_POINT ( 'NONE',  ( -1.428710472040144452, 19.32843595812722626, -1.500000000000002220 ) ) ;
#35040 = CIRCLE ( 'NONE', #91729, 91.74549126261079834 ) ;
#35042 = CARTESIAN_POINT ( 'NONE',  ( -10.26072176705811145, -4.666310954396869271, 28.98969649327457532 ) ) ;
#35043 = DIRECTION ( 'NONE',  ( -3.773278334453079618E-23, 0.9999999999976377785, 2.173523156925979975E-06 ) ) ;
#35044 = CARTESIAN_POINT ( 'NONE',  ( 13.37688099249405127, 14.58279310912311111, -1.500000000000002220 ) ) ;
#35045 = ORIENTED_EDGE ( 'NONE', *, *, #47496, .T. ) ;
#35046 = CARTESIAN_POINT ( 'NONE',  ( -18.77428246231291808, -7.638711222589018135, 11.49999999999999645 ) ) ;
#35047 = CARTESIAN_POINT ( 'NONE',  ( -10.11875734969026297, 6.376774720514426953, 30.51402280011862089 ) ) ;
#35048 = CARTESIAN_POINT ( 'NONE',  ( -41.62287095715006302, -29.50250786944525672, 11.44777988621624232 ) ) ;
#35049 = VERTEX_POINT ( 'NONE', #50942 ) ;
#35050 = CARTESIAN_POINT ( 'NONE',  ( -99.53087172303294494, -25.26929610620923228, 4.063316286417863132 ) ) ;
#35051 = CARTESIAN_POINT ( 'NONE',  ( 14.78484767477524819, -3.316774720514429120, -28.43034250232787841 ) ) ;
#35052 = CARTESIAN_POINT ( 'NONE',  ( 22.81105451610979173, 2.682774720514426559, -16.21691820600746681 ) ) ;
#35053 = CARTESIAN_POINT ( 'NONE',  ( 7.160000000000000142, -6.754662360505033547, 8.925641719537455998 ) ) ;
#35054 = CARTESIAN_POINT ( 'NONE',  ( -71.62287095715002749, -24.33832256527048088, 0.1851278514138635367 ) ) ;
#35055 = CARTESIAN_POINT ( 'NONE',  ( -4.446071851354966853, 19.53225066162704948, -1.500000000000002220 ) ) ;
#35056 = B_SPLINE_CURVE_WITH_KNOTS ( 'NONE', 3,
 ( #86806, #24406, #9180, #94919, #71096, #78178 ),
 .UNSPECIFIED., .F., .F.,
 ( 4, 2, 4 ),
 ( 0.000000000000000000, 0.001380901958385397218, 0.002761803916770794436 ),
 .UNSPECIFIED. ) ;
#35057 = CARTESIAN_POINT ( 'NONE',  ( -124.6228709571500559, -29.50250786944525672, 11.44777988621622811 ) ) ;
#35058 = EDGE_LOOP ( 'NONE', ( #22785, #45855, #34, #60298 ) ) ;
#35059 = B_SPLINE_CURVE_WITH_KNOTS ( 'NONE', 3,
 ( #24825, #33441, #95843, #1509 ),
 .UNSPECIFIED., .F., .F.,
 ( 4, 4 ),
 ( 0.000000000000000000, 1.000000000000000000 ),
 .UNSPECIFIED. ) ;
#35060 = CARTESIAN_POINT ( 'NONE',  ( -82.62287095715005592, -29.50247984919015209, -1.443849546365053582 ) ) ;
#35061 = B_SPLINE_CURVE_WITH_KNOTS ( 'NONE', 3,
 ( #37922, #355, #54656, #68377, #22179, #99791 ),
 .UNSPECIFIED., .F., .F.,
 ( 4, 2, 4 ),
 ( 0.000000000000000000, 0.001380901958385381606, 0.002761803916770763211 ),
 .UNSPECIFIED. ) ;
#35062 = CARTESIAN_POINT ( 'NONE',  ( -127.5228709571500616, -23.94994826722565406, -0.6494450866342692530 ) ) ;
#35063 = CARTESIAN_POINT ( 'NONE',  ( -79.35172094158247091, -25.27805121895104534, 5.822999711083195251 ) ) ;
#35064 = CARTESIAN_POINT ( 'NONE',  ( -9.940598223437577374, -5.876774720514426953, 17.91871304725684766 ) ) ;
#35066 = EDGE_CURVE ( 'NONE', #31571, #54541, #90750, .T. ) ;
#35065 = CARTESIAN_POINT ( 'NONE',  ( -73.50297087286094211, -24.34968618360933590, 0.1864209137778806424 ) ) ;
#35067 = DIRECTION ( 'NONE',  ( -1.000000000000000000, 0.000000000000000000, 0.000000000000000000 ) ) ;
#35068 = ADVANCED_FACE ( 'NONE', ( #90984 ), #21455, .F. ) ;
#35069 = DIRECTION ( 'NONE',  ( 0.000000000000000000, -1.000000000000000000, 0.000000000000000000 ) ) ;
#35070 = ORIENTED_EDGE ( 'NONE', *, *, #5842, .T. ) ;
#35071 = CARTESIAN_POINT ( 'NONE',  ( 18.91379238805564356, 7.493326543281090935, 11.49999999999998934 ) ) ;
#35072 = ORIENTED_EDGE ( 'NONE', *, *, #33540, .T. ) ;
#35073 = CARTESIAN_POINT ( 'NONE',  ( -22.40196285382242536, -4.882868457752029379, 11.49999999999998934 ) ) ;
#35074 = CARTESIAN_POINT ( 'NONE',  ( -32.50393181231471118, -23.96119346886880663, -0.6495511937831992544 ) ) ;
#35075 = ORIENTED_EDGE ( 'NONE', *, *, #70413, .T. ) ;
#35076 = CARTESIAN_POINT ( 'NONE',  ( -49.22373291780066751, -25.29465393801191553, 4.480743166237341590 ) ) ;
#35077 = AXIS2_PLACEMENT_3D ( 'NONE', #38396, #47021, #77939 ) ;
#35078 = CARTESIAN_POINT ( 'NONE',  ( -49.84148113843717454, -25.12215395822629560, 6.992078084850652964 ) ) ;
#35079 = CARTESIAN_POINT ( 'NONE',  ( -87.62287095715004170, -24.64898659630528854, 1.056161002820827921 ) ) ;
#35080 = CARTESIAN_POINT ( 'NONE',  ( 7.993063233546146229, -19.64520799392144568, 11.49999999999999645 ) ) ;
#35081 = CARTESIAN_POINT ( 'NONE',  ( -18.13406196532287140, 12.77545654309102474, 11.49999999999998934 ) ) ;
#35084 = ADVANCED_FACE ( 'NONE', ( #28098 ), #96599, .T. ) ;
#35083 = CARTESIAN_POINT ( 'NONE',  ( 17.26003113218828489, 11.23261964116016642, 11.49999999999998934 ) ) ;
#35082 = CC_DESIGN_DATE_AND_TIME_ASSIGNMENT ( #22659, #54151, ( #31288 ) ) ;
#35085 = AXIS2_PLACEMENT_3D ( 'NONE', #39660, #94955, #23934 ) ;
#35086 = ORIENTED_EDGE ( 'NONE', *, *, #95473, .F. ) ;
#35087 = DIRECTION ( 'NONE',  ( -3.773278334453079618E-23, 0.9999999999976377785, 2.173523156925979975E-06 ) ) ;
#35088 = ORIENTED_EDGE ( 'NONE', *, *, #42263, .F. ) ;
#35089 = CARTESIAN_POINT ( 'NONE',  ( -36.92287095715006018, -23.47596703998600276, 11.44779298504227683 ) ) ;
#35090 = DIRECTION ( 'NONE',  ( -0.4009304992412300317, -6.845827386180410961E-16, -0.9161084732596779245 ) ) ;
#35091 = VERTEX_POINT ( 'NONE', #98083 ) ;
#35092 = AXIS2_PLACEMENT_3D ( 'NONE', #47691, #39570, #40581 ) ;
#35093 = ORIENTED_EDGE ( 'NONE', *, *, #37973, .T. ) ;
#35094 = VECTOR ( 'NONE', #83873, 1000.000000000000000 ) ;
#35095 = ORIENTED_EDGE ( 'NONE', *, *, #74802, .F. ) ;
#35096 = CARTESIAN_POINT ( 'NONE',  ( -77.52287095715009002, -24.35013146730204170, 9.818937971375095941 ) ) ;
#35097 = CARTESIAN_POINT ( 'NONE',  ( -71.55620429048337883, -24.64965694238574301, 8.947790433994201820 ) ) ;
#35098 = CARTESIAN_POINT ( 'NONE',  ( 14.70028154892705707, -3.418387289272210250, -28.41026772490150876 ) ) ;
#35099 = CARTESIAN_POINT ( 'NONE',  ( 18.78520451414993531, -8.817701518030307994, -1.500000000000002220 ) ) ;
#35100 = B_SPLINE_CURVE_WITH_KNOTS ( 'NONE', 3,
 ( #26896, #16025, #99749, #37879, #15526, #30252 ),
 .UNSPECIFIED., .F., .F.,
 ( 4, 2, 4 ),
 ( 0.000000000000000000, 0.0002698174196818396231, 0.0005396348393636792463 ),
 .UNSPECIFIED. ) ;
#35101 = CARTESIAN_POINT ( 'NONE',  ( 19.96715809174937561, -8.635335823514383335, 11.49999999999999645 ) ) ;
#35102 = ORIENTED_EDGE ( 'NONE', *, *, #84031, .T. ) ;
#35103 = LINE ( 'NONE', #28971, #12624 ) ;
#35104 = CARTESIAN_POINT ( 'NONE',  ( -115.5917283184090394, -24.15503026093916716, -0.2815557561904330486 ) ) ;
#35105 = CARTESIAN_POINT ( 'NONE',  ( -22.05133119090760019, 4.102169094691678453, -1.500000000000002220 ) ) ;
#35106 = AXIS2_PLACEMENT_3D ( 'NONE', #26693, #27194, #34305 ) ;
#35107 = LINE ( 'NONE', #68052, #1148 ) ;
#35108 = CARTESIAN_POINT ( 'NONE',  ( -65.66192201872799217, -23.48783264082477018, -1.443836473390096353 ) ) ;
#35109 = VERTEX_POINT ( 'NONE', #51936 ) ;
#35110 = DIRECTION ( 'NONE',  ( -1.000000000000000000, 0.000000000000000000, 0.000000000000000000 ) ) ;
#35111 = CARTESIAN_POINT ( 'NONE',  ( -4.621320343559261801, 12.74999999999999645, 2.100000000000000089 ) ) ;
#35112 = ORIENTED_EDGE ( 'NONE', *, *, #43922, .T. ) ;
#35113 = VERTEX_POINT ( 'NONE', #82865 ) ;
#35114 = CARTESIAN_POINT ( 'NONE',  ( 8.971512145086521173, -7.528487854913501920, 6.500000000000000888 ) ) ;
#35115 = ORIENTED_EDGE ( 'NONE', *, *, #18638, .F. ) ;
#35116 = CARTESIAN_POINT ( 'NONE',  ( 17.78463046036513617, -11.72987588014745342, -1.500000000000002220 ) ) ;
#35117 = ORIENTED_EDGE ( 'NONE', *, *, #69596, .T. ) ;
#35118 = CARTESIAN_POINT ( 'NONE',  ( -89.81226385320383088, -25.23397913219354649, 6.409327625488847602 ) ) ;
#35119 = CARTESIAN_POINT ( 'NONE',  ( -11.22809577558575000, 18.72649003030000259, 11.49999999999998934 ) ) ;
#35120 = CARTESIAN_POINT ( 'NONE',  ( -38.52287095715009002, -23.72773821059535848, 11.05748984161097326 ) ) ;
#35121 = CARTESIAN_POINT ( 'NONE',  ( 19.67839991682829748, -11.23141783594569354, 11.49999999999998934 ) ) ;
#35122 = DIRECTION ( 'NONE',  ( -0.9161084732596777025, 4.164321980682960499E-15, 0.4009304992412306978 ) ) ;
#35123 = CARTESIAN_POINT ( 'NONE',  ( -99.52287095715006160, -29.50250786944525672, 11.44777988621623166 ) ) ;
#35124 = CARTESIAN_POINT ( 'NONE',  ( 19.95399986947220583, -8.914707708046476498, -1.500000000000002220 ) ) ;
#35125 = CARTESIAN_POINT ( 'NONE',  ( 7.081057417352553784, -6.376774720514424288, 21.11453472826393352 ) ) ;
#35126 = ORIENTED_EDGE ( 'NONE', *, *, #31078, .T. ) ;
#35127 = FACE_BOUND ( 'NONE', #3551, .T. ) ;
#35128 = CARTESIAN_POINT ( 'NONE',  ( -73.62287095715005592, -24.64898659630367916, 1.056161002820824368 ) ) ;
#35129 = EDGE_CURVE ( 'NONE', #30069, #95739, #73006, .T. ) ;
#35130 = VECTOR ( 'NONE', #45957, 1000.000000000000000 ) ;
#35131 = ORIENTED_EDGE ( 'NONE', *, *, #57250, .T. ) ;
#35132 = CARTESIAN_POINT ( 'NONE',  ( -30.60851184801261837, -24.48743478789338468, 9.418369803765530790 ) ) ;
#35133 = ORIENTED_EDGE ( 'NONE', *, *, #49216, .T. ) ;
#35134 = ADVANCED_FACE ( 'NONE', ( #53934 ), #92970, .T. ) ;
#35135 = LINE ( 'NONE', #96522, #5432 ) ;
#35136 = VECTOR ( 'NONE', #23884, 1000.000000000000114 ) ;
#35137 = CARTESIAN_POINT ( 'NONE',  ( -120.6228709571500417, -23.47596703998600631, 11.44779298504227683 ) ) ;
#35138 = CARTESIAN_POINT ( 'NONE',  ( -20.90244970016518877, -3.954922567530639199, 11.49999999999998934 ) ) ;
#35139 = CARTESIAN_POINT ( 'NONE',  ( -30.49308942697465952, -23.47593901973084485, -1.443836476861628970 ) ) ;
#35140 = EDGE_CURVE ( 'NONE', #63070, #50327, #37949, .T. ) ;
#35141 = CARTESIAN_POINT ( 'NONE',  ( -27.08002768120591242, -24.75186003446978944, 2.428019306975902847 ) ) ;
#35142 = CARTESIAN_POINT ( 'NONE',  ( -114.5228709571500616, -24.65952944569305316, 1.056160979905704123 ) ) ;
#35143 = CARTESIAN_POINT ( 'NONE',  ( -84.62287095715005592, -24.66019654487199730, 8.947790411086128159 ) ) ;
#35144 = CARTESIAN_POINT ( 'NONE',  ( -44.62287095715007013, -23.95044443724992078, 10.65354141964649237 ) ) ;
#35145 = ORIENTED_EDGE ( 'NONE', *, *, #33917, .T. ) ;
#35146 = CARTESIAN_POINT ( 'NONE',  ( 3.994393897313025743, -19.14333888664780048, 11.49999999999999645 ) ) ;
#35147 = CARTESIAN_POINT ( 'NONE',  ( 29.73860345376319358, -5.356774720496559894, 7.190646357373898680E-15 ) ) ;
#35148 = LINE ( 'NONE', #67107, #30159 ) ;
#35149 = EDGE_CURVE ( 'NONE', #58528, #40542, #14847, .T. ) ;
#35150 = ORIENTED_EDGE ( 'NONE', *, *, #51980, .T. ) ;
#35151 = DIRECTION ( 'NONE',  ( -3.773278334453079618E-23, 0.9999999999976377785, 2.173523156925979975E-06 ) ) ;
#35152 = CARTESIAN_POINT ( 'NONE',  ( -100.9051445215427947, -25.04466488984843764, 7.507873723526761189 ) ) ;
#35153 = VECTOR ( 'NONE', #34540, 1000.000000000000114 ) ;
#35154 = CARTESIAN_POINT ( 'NONE',  ( -51.58953762381672448, -23.48783264082478084, -1.443836473390070596 ) ) ;
#35155 = CARTESIAN_POINT ( 'NONE',  ( -80.51244414166535535, -25.24813991317089545, 7.563173748558941867 ) ) ;
#35156 = CARTESIAN_POINT ( 'NONE',  ( 0.7877182283408599162, 19.66719298131377514, -1.500000000000002220 ) ) ;
#35157 = VERTEX_POINT ( 'NONE', #22451 ) ;
#35158 = DIRECTION ( 'NONE',  ( -1.000000000000000000, -3.773278334444166432E-23, -8.201307841325785021E-29 ) ) ;
#35159 = CARTESIAN_POINT ( 'NONE',  ( -118.5228709571501184, -23.48783264082477373, -1.443836473390083475 ) ) ;
#35160 = VECTOR ( 'NONE', #33311, 1000.000000000000114 ) ;
#35161 = APPROVAL_DATE_TIME ( #21401, #82276 ) ;
#35162 = B_SPLINE_CURVE_WITH_KNOTS ( 'NONE', 3,
 ( #82450, #75330, #91556, #14428 ),
 .UNSPECIFIED., .F., .F.,
 ( 4, 4 ),
 ( 0.000000000000000000, 9.999999999996123101E-05 ),
 .UNSPECIFIED. ) ;
#35163 = VERTEX_POINT ( 'NONE', #22943 ) ;
#35164 = CARTESIAN_POINT ( 'NONE',  ( 9.071512145086506607, 0.000000000000000000, 3.687490859131163479 ) ) ;
#35165 = DIRECTION ( 'NONE',  ( -3.773278334444167608E-23, 1.000000000000000000, 0.000000000000000000 ) ) ;
#35166 = CARTESIAN_POINT ( 'NONE',  ( -69.62287095715005592, -23.94994826722515313, -0.6494450866351728635 ) ) ;
#35167 = CARTESIAN_POINT ( 'NONE',  ( -118.5546855235172785, -24.15543982623907482, -0.2315651400026558782 ) ) ;
#35168 = CARTESIAN_POINT ( 'NONE',  ( -80.90938632151146237, -25.31249729222309597, 5.276660411446114196 ) ) ;
#35169 = TOROIDAL_SURFACE ( 'NONE', #7561, 80.18232118519038920, 8.160000000000000142 ) ;
#35170 = CIRCLE ( 'NONE', #43285, 3.060000000000000053 ) ;
#35171 = CARTESIAN_POINT ( 'NONE',  ( 27.86270917940689174, 0.3587747205144265483, 29.02104833056109001 ) ) ;
#35172 = DIRECTION ( 'NONE',  ( -3.773278334453079618E-23, 0.9999999999976377785, 2.173523156925979975E-06 ) ) ;
#35173 = CARTESIAN_POINT ( 'NONE',  ( 18.80405327530603543, -6.659971710459020144, -1.500000000000002220 ) ) ;
#35174 = CARTESIAN_POINT ( 'NONE',  ( -0.08148069157530678230, -21.99516841672774348, 10.01542119451336887 ) ) ;
#35175 = CARTESIAN_POINT ( 'NONE',  ( 0.1862606309321278575, -19.90735222434816976, -1.500000000000002220 ) ) ;
#35176 = ORIENTED_EDGE ( 'NONE', *, *, #92591, .T. ) ;
#35177 = LINE ( 'NONE', #66147, #65378 ) ;
#35178 = EDGE_CURVE ( 'NONE', #55445, #84745, #97264, .T. ) ;
#35179 = DIRECTION ( 'NONE',  ( 1.000000000000000000, 0.000000000000000000, 0.000000000000000000 ) ) ;
#35180 = CARTESIAN_POINT ( 'NONE',  ( 9.146648804574669001, -3.316774720514593433, -28.07004961703220758 ) ) ;
#35181 = CARTESIAN_POINT ( 'NONE',  ( -26.36173610263349687, -24.88504641058569433, 6.596543391192986938 ) ) ;
#35182 = CARTESIAN_POINT ( 'NONE',  ( -7.138063944469604571, -5.876774720514408301, 19.21974929698718881 ) ) ;
#35183 = EDGE_CURVE ( 'NONE', #39855, #28152, #30077, .T. ) ;
#35184 = CARTESIAN_POINT ( 'NONE',  ( -62.55620429048343567, -23.47596703998600276, 11.44779298504227505 ) ) ;
#35185 = ORIENTED_EDGE ( 'NONE', *, *, #72263, .F. ) ;
#35186 = CARTESIAN_POINT ( 'NONE',  ( 30.53060340732036337, -5.022552014119394670, -1.287656715832136367 ) ) ;
#35187 = LINE ( 'NONE', #66159, #22516 ) ;
#35188 = ORIENTED_EDGE ( 'NONE', *, *, #85418, .F. ) ;
#35189 = B_SPLINE_CURVE_WITH_KNOTS ( 'NONE', 3,
 ( #17590, #55672, #33306, #64294, #24195, #32313, #867, #55171 ),
 .UNSPECIFIED., .F., .F.,
 ( 4, 2, 2, 4 ),
 ( -0.001240355328176873757, -0.0002398155169399556787, 0.0007607242942969623997, 0.002761803916770794003 ),
 .UNSPECIFIED. ) ;
#35190 = CARTESIAN_POINT ( 'NONE',  ( 13.55758662847591900, -15.04642845256218031, -1.500000000000002220 ) ) ;
#35191 = CARTESIAN_POINT ( 'NONE',  ( -68.97719918508434489, -25.28711388198359700, 5.838800831980617723 ) ) ;
#35192 = CARTESIAN_POINT ( 'NONE',  ( 13.57581083383197296, -5.876774720514426953, 19.78786796564403616 ) ) ;
#35193 = AXIS2_PLACEMENT_3D ( 'NONE', #48351, #95011, #16378 ) ;
#35194 = CARTESIAN_POINT ( 'NONE',  ( -23.62875734969026453, 6.143225279485574397, 23.50402280011862288 ) ) ;
#35195 = EDGE_LOOP ( 'NONE', ( #37674, #88259 ) ) ;
#35196 = CARTESIAN_POINT ( 'NONE',  ( -80.43221577628075636, -25.31553502933635968, 4.967019755914117596 ) ) ;
#35197 = CARTESIAN_POINT ( 'NONE',  ( -1.836964591723098117, -6.376774720514410077, 19.23384392940399223 ) ) ;
#35198 = CARTESIAN_POINT ( 'NONE',  ( -19.91332876899582160, 2.521106391696132931, -1.500000000000002220 ) ) ;
#35199 = CARTESIAN_POINT ( 'NONE',  ( -1.027814097295878693, -20.98676634966329146, 11.49999999999999645 ) ) ;
#35200 = VECTOR ( 'NONE', #63743, 1000.000000000000114 ) ;
#35201 = LINE ( 'NONE', #75242, #46955 ) ;
#35202 = CARTESIAN_POINT ( 'NONE',  ( -70.63224074161550448, -24.63419186844611275, 9.035850630976918652 ) ) ;
#35203 = CARTESIAN_POINT ( 'NONE',  ( 5.627179592841175193, 21.36305014179116668, -1.500000000000002220 ) ) ;
#35204 = CC_DESIGN_PERSON_AND_ORGANIZATION_ASSIGNMENT ( #59127, #52505, ( #2853 ) ) ;
#35205 = CARTESIAN_POINT ( 'NONE',  ( -39.51244657141699435, -25.31589210260499101, 4.531907284092489441 ) ) ;
#35206 = DIRECTION ( 'NONE',  ( -9.779078418496698369E-14, 0.000000000000000000, -1.000000000000000000 ) ) ;
#35207 = FACE_OUTER_BOUND ( 'NONE', #347, .T. ) ;
#35208 = ORIENTED_EDGE ( 'NONE', *, *, #81857, .F. ) ;
#35209 = PLANE ( 'NONE',  #38128 ) ;
#35210 = CARTESIAN_POINT ( 'NONE',  ( -31.61026445906011517, -23.73766607897669800, -1.055555164236445131 ) ) ;
#35211 = ORIENTED_EDGE ( 'NONE', *, *, #56792, .F. ) ;
#35212 = VERTEX_POINT ( 'NONE', #61552 ) ;
#35213 = FACE_OUTER_BOUND ( 'NONE', #48423, .T. ) ;
#35214 = CARTESIAN_POINT ( 'NONE',  ( -125.5228709571500616, -23.47596703998600631, 11.44779298504227683 ) ) ;
#35215 = CARTESIAN_POINT ( 'NONE',  ( -61.92287095715004597, -23.47593901973090169, -1.443836447538997758 ) ) ;
#35216 = CARTESIAN_POINT ( 'NONE',  ( 20.45670835789597319, 2.398913822417158226, -1.500000000000002220 ) ) ;
#35217 = CARTESIAN_POINT ( 'NONE',  ( 18.51311748589099082, 11.02308708543723270, 11.49999999999999645 ) ) ;
#35218 = ORIENTED_EDGE ( 'NONE', *, *, #39225, .F. ) ;
#35219 = CARTESIAN_POINT ( 'NONE',  ( 9.071512145086501278, 0.000000000000000000, -3.687490859131163479 ) ) ;
#35220 = EDGE_CURVE ( 'NONE', #65068, #48069, #17881, .T. ) ;
#35221 = CARTESIAN_POINT ( 'NONE',  ( 6.910430652544937935, -5.876774720514418071, 20.24472806504191169 ) ) ;
#35222 = PLANE ( 'NONE',  #5900 ) ;
#35223 = CARTESIAN_POINT ( 'NONE',  ( -10.28394192611005842, 19.82837715243953625, -1.500000000000002220 ) ) ;
#35224 = AXIS2_PLACEMENT_3D ( 'NONE', #6551, #36998, #89793 ) ;
#35225 = CARTESIAN_POINT ( 'NONE',  ( 29.71608694565284026, -4.561299274004467996, 27.78615310300602559 ) ) ;
#35226 = CARTESIAN_POINT ( 'NONE',  ( 5.097264368844747651, 3.299463065352477908, -27.56135813788838718 ) ) ;
#35227 = ORIENTED_EDGE ( 'NONE', *, *, #34378, .F. ) ;
#35228 = DIRECTION ( 'NONE',  ( -1.000000000000000000, -0.000000000000000000, -0.000000000000000000 ) ) ;
#35229 = CARTESIAN_POINT ( 'NONE',  ( -29.49875734969026198, 5.965225279485572685, 10.11402280011862587 ) ) ;
#35230 = CARTESIAN_POINT ( 'NONE',  ( 18.76864855846692492, -9.085702381504452418, 11.49999999999998934 ) ) ;
#35231 = VERTEX_POINT ( 'NONE', #91475 ) ;
#35233 = VERTEX_POINT ( 'NONE', #6742 ) ;
#35232 = LINE ( 'NONE', #66204, #70124 ) ;
#35234 = AXIS2_PLACEMENT_3D ( 'NONE', #27841, #72530, #56816 ) ;
#35235 = ORIENTED_EDGE ( 'NONE', *, *, #22607, .F. ) ;
#35236 = CARTESIAN_POINT ( 'NONE',  ( -100.5472794312289295, -24.73531770709095312, 8.716586749053508498 ) ) ;
#35237 = CARTESIAN_POINT ( 'NONE',  ( 15.50021099394596646, 14.30638080151107694, -1.500000000000002220 ) ) ;
#35238 = EDGE_LOOP ( 'NONE', ( #40570, #19350, #59968, #13628 ) ) ;
#35239 = CARTESIAN_POINT ( 'NONE',  ( -28.52287095715005805, -24.48836230353387222, 1.056161703005638719 ) ) ;
#35240 = CARTESIAN_POINT ( 'NONE',  ( -49.20721729649422826, -25.30221391860467151, 5.306624793317872957 ) ) ;
#35241 = CARTESIAN_POINT ( 'NONE',  ( -120.5936535130245773, -23.48786465467241769, 11.44779295918253936 ) ) ;
#35242 = AXIS2_PLACEMENT_3D ( 'NONE', #45117, #15645, #16143 ) ;
#35243 = CARTESIAN_POINT ( 'NONE',  ( -64.62287095715005592, -23.48786465467241413, 11.44779295918254824 ) ) ;
#35244 = CARTESIAN_POINT ( 'NONE',  ( 7.089543269230769162, -6.376774720514413630, 19.75741185897435415 ) ) ;
#35245 = CARTESIAN_POINT ( 'NONE',  ( -21.36891742734480104, 3.643610035731704055, -1.500000000000002220 ) ) ;
#35246 = CARTESIAN_POINT ( 'NONE',  ( -63.52287095715006160, -23.48786465467241058, 11.44779295918254824 ) ) ;
#35247 = EDGE_CURVE ( 'NONE', #17897, #20245, #13852, .T. ) ;
#35249 = ORIENTED_EDGE ( 'NONE', *, *, #36328, .T. ) ;
#35248 = CARTESIAN_POINT ( 'NONE',  ( -16.22183044023116238, -15.26045173261249310, 11.49999999999999645 ) ) ;
#35250 = B_SPLINE_CURVE_WITH_KNOTS ( 'NONE', 3,
 ( #43507, #35883, #59227, #51616, #9292, #24016 ),
 .UNSPECIFIED., .F., .F.,
 ( 4, 2, 4 ),
 ( 1.570755371633718645E-05, 0.001396183895866086452, 0.002776660238015836012 ),
 .UNSPECIFIED. ) ;
#35251 = CARTESIAN_POINT ( 'NONE',  ( -76.92287095715008149, -23.47593901973090524, -1.443836447538997980 ) ) ;
#35252 = CARTESIAN_POINT ( 'NONE',  ( 7.087697398486194622, -6.376774720514418959, 20.45710073441444621 ) ) ;
#35253 = CYLINDRICAL_SURFACE ( 'NONE', #87760, 0.3000000000000016542 ) ;
#35254 = ORIENTED_EDGE ( 'NONE', *, *, #15557, .T. ) ;
#35255 = B_SPLINE_CURVE_WITH_KNOTS ( 'NONE', 3,
 ( #75347, #82470, #98186, #81485 ),
 .UNSPECIFIED., .F., .F.,
 ( 4, 4 ),
 ( 0.1188422306059488676, 0.1198429776467144353 ),
 .UNSPECIFIED. ) ;
#35256 = B_SPLINE_CURVE_WITH_KNOTS ( 'NONE', 3,
 ( #48340, #10269, #94999, #72181 ),
 .UNSPECIFIED., .F., .F.,
 ( 4, 4 ),
 ( 0.5909219629093517279, 0.5999283941814672616 ),
 .UNSPECIFIED. ) ;
#35258 = ORIENTED_EDGE ( 'NONE', *, *, #47320, .F. ) ;
#35257 = DIRECTION ( 'NONE',  ( 3.469446951953612611E-15, -1.000000000000000000, 0.000000000000000000 ) ) ;
#35259 = VERTEX_POINT ( 'NONE', #99573 ) ;
#35260 = EDGE_CURVE ( 'NONE', #52403, #50453, #13672, .T. ) ;
#35261 = CARTESIAN_POINT ( 'NONE',  ( -103.6228709571500417, -23.47596703998600631, 11.44779298504227860 ) ) ;
#35262 = PLANE ( 'NONE',  #90283 ) ;
#35263 = EDGE_CURVE ( 'NONE', #40347, #47659, #26985, .T. ) ;
#35264 = CARTESIAN_POINT ( 'NONE',  ( -63.55620429048339304, -24.65952944569304606, 1.056160979905694131 ) ) ;
#35265 = CARTESIAN_POINT ( 'NONE',  ( -87.52287095715006160, -23.95044443724992789, 10.65354141964649415 ) ) ;
#35266 = CARTESIAN_POINT ( 'NONE',  ( -16.89397143409390623, -5.876774720514426953, 16.89397143409405899 ) ) ;
#35267 = ORIENTED_EDGE ( 'NONE', *, *, #39985, .F. ) ;
#35268 = CARTESIAN_POINT ( 'NONE',  ( -9.899997732206244905, -16.63842163800745766, 11.49999999999999645 ) ) ;
#35269 = CARTESIAN_POINT ( 'NONE',  ( -22.05275734969026047, -0.3587747205144262708, 31.02402280011862246 ) ) ;
#35270 = CARTESIAN_POINT ( 'NONE',  ( -16.84940295534276800, 14.81145437567392698, -1.500000000000002220 ) ) ;
#35271 = EDGE_CURVE ( 'NONE', #26418, #28486, #83867, .T. ) ;
#35272 = ORIENTED_EDGE ( 'NONE', *, *, #37206, .T. ) ;
#35273 = DIRECTION ( 'NONE',  ( -0.000000000000000000, -1.000000000000000000, -0.000000000000000000 ) ) ;
#35274 = CARTESIAN_POINT ( 'NONE',  ( 11.25623914429021788, 3.316774720514424235, -27.04805245727492391 ) ) ;
#35275 = VECTOR ( 'NONE', #94763, 1000.000000000000000 ) ;
#35276 = PLANE ( 'NONE',  #44992 ) ;
#35277 = CARTESIAN_POINT ( 'NONE',  ( -130.5728709571500588, -24.57143472585066846, 0.8294870405985542705 ) ) ;
#35278 = CARTESIAN_POINT ( 'NONE',  ( -12.94911239430987315, -14.73082512860577609, -1.500000000000002220 ) ) ;
#35279 = B_SPLINE_SURFACE_WITH_KNOTS ( 'NONE', 3, 3, ( 
 ( #77037, #7538, #38492, #69442 ),
 ( #31375, #1941, #9538, #32885 ),
 ( #85157, #62853, #16643, #48115 ),
 ( #79043, #46614, #55734, #93771 ),
 ( #71956, #77536, #63857, #2437 ),
 ( #24261, #61842, #23753, #23249 ),
 ( #54231, #94771, #78029, #55236 ) ),
 .UNSPECIFIED., .F., .F., .F.,
 ( 4, 3, 4 ),
 ( 4, 4 ),
 ( 0.3495694201709305671, 0.5199404137006313764, 0.6903114072303322413 ),
 ( 0.6891232925396537645, 0.7171688452333530028 ),
 .UNSPECIFIED. ) ;
#35280 = CARTESIAN_POINT ( 'NONE',  ( -49.51094237493734340, -25.27738574500889257, 4.037618946434144540 ) ) ;
#35281 = ORIENTED_EDGE ( 'NONE', *, *, #21227, .F. ) ;
#35282 = CARTESIAN_POINT ( 'NONE',  ( -17.63906703526961550, 12.34593017946836291, -1.500000000000002220 ) ) ;
#35283 = AXIS2_PLACEMENT_3D ( 'NONE', #61872, #92797, #37022 ) ;
#35284 = CARTESIAN_POINT ( 'NONE',  ( 9.843544857143434967, -5.965225279485572685, -27.49819965379373343 ) ) ;
#35285 = CARTESIAN_POINT ( 'NONE',  ( -71.01839045479064794, -25.25639544905377321, 6.841306829129303324 ) ) ;
#35286 = CARTESIAN_POINT ( 'NONE',  ( -100.5228709571500900, -23.48783264082477018, -1.443836473390086583 ) ) ;
#35287 = CARTESIAN_POINT ( 'NONE',  ( -128.6228709571500417, -29.50248528299804818, 1.056150453629047137 ) ) ;
#35288 = CARTESIAN_POINT ( 'NONE',  ( -10.52143791818333085, 20.43947972196396989, -1.500000000000002220 ) ) ;
#35289 = DATE_TIME_ROLE ( 'creation_date' ) ;
#35290 = DIRECTION ( 'NONE',  ( 0.1489078231574191002, -6.845827386180410961E-16, -0.9888510809027407644 ) ) ;
#35291 = CARTESIAN_POINT ( 'NONE',  ( -49.49485161334624195, -24.34968618360933590, 0.1864209137778799485 ) ) ;
#35292 = CARTESIAN_POINT ( 'NONE',  ( 17.00595499256408871, 10.69956108467327205, 11.49999999999999645 ) ) ;
#35293 = CARTESIAN_POINT ( 'NONE',  ( 30.53060340732036337, -5.297812262124697469, 1.539714685317310483 ) ) ;
#35294 = CARTESIAN_POINT ( 'NONE',  ( -32.53787845003378720, -24.35071581493542681, 9.817618358456035921 ) ) ;
#35296 = B_SPLINE_CURVE_WITH_KNOTS ( 'NONE', 3,
 ( #33675, #63641, #9323, #96073, #26055, #95072 ),
 .UNSPECIFIED., .F., .F.,
 ( 4, 2, 4 ),
 ( 0.000000000000000000, 0.001380901958385387894, 0.002761803916770775788 ),
 .UNSPECIFIED. ) ;
#35295 = PRODUCT_DEFINITION_SHAPE ( 'NONE', 'NONE',  #100432 ) ;
#35297 = FACE_OUTER_BOUND ( 'NONE', #2606, .T. ) ;
#35298 = DIRECTION ( 'NONE',  ( 0.000000000000000000, -1.000000000000000000, 0.000000000000000000 ) ) ;
#35299 = DIRECTION ( 'NONE',  ( 3.773278334444166432E-23, -1.000000000000000000, 0.000000000000000000 ) ) ;
#35300 = CARTESIAN_POINT ( 'NONE',  ( -13.97081141688431138, 14.13901428111770819, -1.500000000000002220 ) ) ;
#35301 = B_SPLINE_CURVE_WITH_KNOTS ( 'NONE', 3,
 ( #74960, #59766, #27802, #66883, #44532, #75456 ),
 .UNSPECIFIED., .F., .F.,
 ( 4, 2, 4 ),
 ( 6.391158118955276782E-06, 0.001387004593080777256, 0.002767618028042598960 ),
 .UNSPECIFIED. ) ;
#35302 = CARTESIAN_POINT ( 'NONE',  ( -113.5871619926412990, -24.65952944569305316, 1.056160979905705011 ) ) ;
#35303 = CARTESIAN_POINT ( 'NONE',  ( -2.117704968268854682, 19.61795684621070990, -1.500000000000002220 ) ) ;
#35304 = AXIS2_PLACEMENT_3D ( 'NONE', #58371, #10185, #4075 ) ;
#35305 = CARTESIAN_POINT ( 'NONE',  ( -27.15721599100127648, 6.376774720514425177, -10.22292133548837256 ) ) ;
#35306 = CARTESIAN_POINT ( 'NONE',  ( -72.92287095715006728, -23.47596703998600631, 11.44779298504227860 ) ) ;
#35307 = FACE_OUTER_BOUND ( 'NONE', #7859, .T. ) ;
#35308 = CARTESIAN_POINT ( 'NONE',  ( -18.80638259998596951, 8.471300643254643603, 11.49999999999999645 ) ) ;
#35309 = AXIS2_PLACEMENT_3D ( 'NONE', #22456, #16862, #78745 ) ;
#35310 = DIRECTION ( 'NONE',  ( 0.000000000000000000, -2.173523156925980399E-06, 0.9999999999976378895 ) ) ;
#35312 = EDGE_CURVE ( 'NONE', #34388, #44867, #19462, .T. ) ;
#35311 = CARTESIAN_POINT ( 'NONE',  ( 20.48348528492645571, -9.684159049092739835, 11.49999999999999645 ) ) ;
#35313 = ORIENTED_EDGE ( 'NONE', *, *, #47248, .T. ) ;
#35314 = FACE_OUTER_BOUND ( 'NONE', #34339, .T. ) ;
#35315 = CARTESIAN_POINT ( 'NONE',  ( 6.365284455128204399, -5.876774720514413630, 19.73076923076922640 ) ) ;
#35316 = VECTOR ( 'NONE', #65992, 1000.000000000000114 ) ;
#35317 = CARTESIAN_POINT ( 'NONE',  ( -27.12300167417273045, -24.61460094789499564, 8.164242432340882871 ) ) ;
#35318 = CARTESIAN_POINT ( 'NONE',  ( -36.55620429048339304, -23.48783264082477373, -1.443836473390072372 ) ) ;
#35319 = ORIENTED_EDGE ( 'NONE', *, *, #91098, .T. ) ;
#35320 = ORIENTED_EDGE ( 'NONE', *, *, #58597, .T. ) ;
#35321 = DIRECTION ( 'NONE',  ( -3.773278334453079030E-23, 0.9999999999976377785, 2.173523156925979128E-06 ) ) ;
#35322 = CARTESIAN_POINT ( 'NONE',  ( -14.01358469492184966, -18.07645309290061064, 11.49999999999998934 ) ) ;
#35323 = DIRECTION ( 'NONE',  ( 0.000000000000000000, 3.563215788492900483E-15, -1.000000000000000000 ) ) ;
#35324 = CARTESIAN_POINT ( 'NONE',  ( 19.31049906410359895, -9.575588319827552652, -1.500000000000002220 ) ) ;
#35325 = DIRECTION ( 'NONE',  ( 0.000000000000000000, 0.000000000000000000, -1.000000000000000000 ) ) ;
#35326 = LINE ( 'NONE', #98702, #90610 ) ;
#35327 = CARTESIAN_POINT ( 'NONE',  ( -12.86601690267178100, 18.50254183665605012, 11.49999999999999645 ) ) ;
#35328 = VERTEX_POINT ( 'NONE', #14347 ) ;
#35329 = CARTESIAN_POINT ( 'NONE',  ( -29.23535468533444259, -25.19827913475990400, 4.357126516840850172 ) ) ;
#35330 = CARTESIAN_POINT ( 'NONE',  ( 20.22059317821533853, 8.664326447042464352, -1.500000000000002220 ) ) ;
#35331 = EDGE_CURVE ( 'NONE', #59549, #27337, #74246, .T. ) ;
#35332 = DIRECTION ( 'NONE',  ( 0.000000000000000000, 1.000000000000000000, 0.000000000000000000 ) ) ;
#35333 = CARTESIAN_POINT ( 'NONE',  ( -69.97769073112337423, -25.04188339297948218, 7.520920306927235011 ) ) ;
#35334 = ORIENTED_EDGE ( 'NONE', *, *, #99, .F. ) ;
#35335 = DIRECTION ( 'NONE',  ( -3.773278334453079618E-23, 0.9999999999976377785, 2.173523156925979975E-06 ) ) ;
#35336 = DIRECTION ( 'NONE',  ( -3.773278334444166432E-23, 1.000000000000000000, 0.000000000000000000 ) ) ;
#35337 = EDGE_LOOP ( 'NONE', ( #18793, #4801, #69004, #12630 ) ) ;
#35338 = CARTESIAN_POINT ( 'NONE',  ( -84.62287095715004170, -24.33832256526968862, 0.1851278514119911178 ) ) ;
#35339 = ADVANCED_FACE ( 'NONE', ( #29581 ), #44298, .T. ) ;
#35340 = ORIENTED_EDGE ( 'NONE', *, *, #5717, .F. ) ;
#35341 = ORIENTED_EDGE ( 'NONE', *, *, #67768, .T. ) ;
#35342 = ORIENTED_EDGE ( 'NONE', *, *, #12424, .T. ) ;
#35343 = LINE ( 'NONE', #20597, #12878 ) ;
#35344 = LINE ( 'NONE', #74878, #85888 ) ;
#35345 = LINE ( 'NONE', #50074, #6601 ) ;
#35346 = CARTESIAN_POINT ( 'NONE',  ( -20.42006937447004233, 0.3101567295262241952, -1.500000000000002220 ) ) ;
#35347 = ORIENTED_EDGE ( 'NONE', *, *, #45604, .F. ) ;
#35348 = CARTESIAN_POINT ( 'NONE',  ( -71.57279388816485266, -25.17182522529348532, 6.802880960782522912 ) ) ;
#35349 = EDGE_CURVE ( 'NONE', #38339, #20357, #2156, .T. ) ;
#35350 = CARTESIAN_POINT ( 'NONE',  ( -29.57432519004955296, -24.58082521808944421, 8.947790440257527678 ) ) ;
#35351 = EDGE_CURVE ( 'NONE', #96258, #70136, #44069, .T. ) ;
#35352 = B_SPLINE_CURVE_WITH_KNOTS ( 'NONE', 3,
 ( #72209, #87418, #95534, #40252 ),
 .UNSPECIFIED., .F., .F.,
 ( 4, 4 ),
 ( 0.000000000000000000, 9.999999999997510880E-05 ),
 .UNSPECIFIED. ) ;
#35353 = CARTESIAN_POINT ( 'NONE',  ( -97.52287095715004739, -24.50216790748205398, 0.6166512839542558355 ) ) ;
#35354 = CARTESIAN_POINT ( 'NONE',  ( -70.87191485471986141, -25.03149828777604213, 7.466452049494895604 ) ) ;
#35355 = ORIENTED_EDGE ( 'NONE', *, *, #89586, .T. ) ;
#35356 = CARTESIAN_POINT ( 'NONE',  ( -28.29914910988898669, -25.21531691454156032, 2.427550070888207401 ) ) ;
#35357 = FACE_OUTER_BOUND ( 'NONE', #61549, .T. ) ;
#35358 = ADVANCED_FACE ( 'NONE', ( #93976 ), #63562, .T. ) ;
#35359 = ORIENTED_EDGE ( 'NONE', *, *, #58676, .T. ) ;
#35360 = CARTESIAN_POINT ( 'NONE',  ( -19.11632921840048738, -8.121837694355717119, 11.49999999999998934 ) ) ;
#35361 = EDGE_LOOP ( 'NONE', ( #56507, #69892, #18870, #62775 ) ) ;
#35363 = EDGE_LOOP ( 'NONE', ( #12015, #81554, #29362, #65313 ) ) ;
#35362 = DIRECTION ( 'NONE',  ( 0.000000000000000000, -0.9999999999976377785, -2.173523156925979975E-06 ) ) ;
#35364 = B_SPLINE_SURFACE_WITH_KNOTS ( 'NONE', 3, 3, ( 
 ( #16584, #64301, #39438, #54671 ),
 ( #17598, #47561, #25202, #78482 ),
 ( #55679, #31828, #85602, #93211 ),
 ( #63803, #17094, #25705, #2384 ),
 ( #8981, #33314, #48056, #95224 ),
 ( #56684, #78985, #86107, #87616 ),
 ( #71395, #16090, #77974, #18099 ) ),
 .UNSPECIFIED., .F., .F., .F.,
 ( 4, 3, 4 ),
 ( 4, 4 ),
 ( 0.7945040050992243641, 0.8970133687736507877, 0.9995227324480771003 ),
 ( 0.9597378799379333580, 0.9611936831856934260 ),
 .UNSPECIFIED. ) ;
#35365 = PLANE ( 'NONE',  #24394 ) ;
#35366 = CARTESIAN_POINT ( 'NONE',  ( -97.52287095715003318, -24.66019654487200441, 8.947790411086119278 ) ) ;
#35367 = ORIENTED_EDGE ( 'NONE', *, *, #12539, .F. ) ;
#35368 = EDGE_LOOP ( 'NONE', ( #48717, #11205, #36960, #94993 ) ) ;
#35369 = CARTESIAN_POINT ( 'NONE',  ( -114.6228709571500701, -23.48783264082478794, -1.443836473390060382 ) ) ;
#35370 = CARTESIAN_POINT ( 'NONE',  ( 29.73860345376319003, -1.682774720514426114, -1.272392034746785860 ) ) ;
#35371 = CARTESIAN_POINT ( 'NONE',  ( -86.52287095715009002, -23.72747288104470087, -1.053458166803225682 ) ) ;
#35372 = CARTESIAN_POINT ( 'NONE',  ( -70.74035176281489612, -25.31201604152037987, 5.376055887764303876 ) ) ;
#35373 = EDGE_CURVE ( 'NONE', #35718, #50270, #18536, .T. ) ;
#35375 = VERTEX_POINT ( 'NONE', #94482 ) ;
#35374 = CARTESIAN_POINT ( 'NONE',  ( -21.55788180805707555, 4.768121097544787190, 11.49999999999999645 ) ) ;
#35376 = FACE_OUTER_BOUND ( 'NONE', #59287, .T. ) ;
#35377 = CARTESIAN_POINT ( 'NONE',  ( 20.74359285767136640, 8.971229656761206428, 11.49999999999998934 ) ) ;
#35378 = AXIS2_PLACEMENT_3D ( 'NONE', #47388, #45397, #55006 ) ;
#35380 = VERTEX_POINT ( 'NONE', #24966 ) ;
#35379 = CARTESIAN_POINT ( 'NONE',  ( -115.5161475269273836, -24.52399227489127043, 9.353111116836528183 ) ) ;
#35381 = ORIENTED_EDGE ( 'NONE', *, *, #82988, .F. ) ;
#35382 = CARTESIAN_POINT ( 'NONE',  ( -10.11875734969026297, -3.316774720514426456, 30.51402280011862089 ) ) ;
#35383 = ADVANCED_FACE ( 'NONE', ( #55940 ), #72163, .T. ) ;
#35384 = AXIS2_PLACEMENT_3D ( 'NONE', #2540, #56340, #17755 ) ;
#35385 = EDGE_CURVE ( 'NONE', #2131, #55067, #13233, .T. ) ;
#35386 = CARTESIAN_POINT ( 'NONE',  ( -57.60487676331112539, -23.73791477778911840, 11.05961554403170588 ) ) ;
#35387 = ORIENTED_EDGE ( 'NONE', *, *, #95823, .F. ) ;
#35388 = CARTESIAN_POINT ( 'NONE',  ( -15.68702345270385834, -14.21367052863537417, -1.500000000000002220 ) ) ;
#35389 = AXIS2_PLACEMENT_3D ( 'NONE', #58892, #3612, #11702 ) ;
#35390 = CARTESIAN_POINT ( 'NONE',  ( 6.132272708306365949, -5.876774720514424288, 21.80683391321003839 ) ) ;
#35391 = CARTESIAN_POINT ( 'NONE',  ( -41.68883930382232705, -25.30531595339526163, 4.893887653588548048 ) ) ;
#35392 = CARTESIAN_POINT ( 'NONE',  ( -19.83904684311861644, 10.14288308415042827, -1.500000000000002220 ) ) ;
#35393 = B_SPLINE_CURVE_WITH_KNOTS ( 'NONE', 3,
 ( #60410, #4113, #43179, #35563 ),
 .UNSPECIFIED., .F., .F.,
 ( 4, 4 ),
 ( 0.000000000000000000, 0.0001000000000000167422 ),
 .UNSPECIFIED. ) ;
#35394 = PLANE ( 'NONE',  #24114 ) ;
#35395 = ADVANCED_FACE ( 'NONE', ( #26485 ), #90369, .T. ) ;
#35396 = ORIENTED_EDGE ( 'NONE', *, *, #42263, .T. ) ;
#35397 = CARTESIAN_POINT ( 'NONE',  ( -66.52287095715007581, -23.47593901973090524, -1.443836447538997092 ) ) ;
#35398 = CARTESIAN_POINT ( 'NONE',  ( -78.64728755545458228, -23.48783264082477018, -1.443836473390096797 ) ) ;
#35399 = EDGE_CURVE ( 'NONE', #50327, #55686, #80362, .T. ) ;
#35400 = CARTESIAN_POINT ( 'NONE',  ( 8.160000000000000142, -9.636585826567532820, 1.623587105904843675 ) ) ;
#35401 = DIRECTION ( 'NONE',  ( 0.000000000000000000, -1.000000000000000000, 0.000000000000000000 ) ) ;
#35402 = EDGE_CURVE ( 'NONE', #82156, #89020, #11742, .T. ) ;
#35404 = VECTOR ( 'NONE', #20560, 1000.000000000000114 ) ;
#35403 = CARTESIAN_POINT ( 'NONE',  ( -19.08498223313328168, 4.104482590468319536, 11.49999999999998934 ) ) ;
#35405 = CARTESIAN_POINT ( 'NONE',  ( -2.751442626040462081, 21.25944542233241563, -1.500000000000002220 ) ) ;
#35406 = CARTESIAN_POINT ( 'NONE',  ( -0.9988807608215116707, -6.376774720514411854, 19.30497968945844889 ) ) ;
#35407 = CARTESIAN_POINT ( 'NONE',  ( -6.660000000000001030, 7.578413286920094194, 5.288828319098143105 ) ) ;
#35408 = CARTESIAN_POINT ( 'NONE',  ( 1.437548984227666304, -5.319565594357255733, 0.000000000000000000 ) ) ;
#35409 = CARTESIAN_POINT ( 'NONE',  ( 20.42703387425654427, 10.12935691860780985, -1.500000000000002220 ) ) ;
#35410 = B_SPLINE_CURVE_WITH_KNOTS ( 'NONE', 3,
 ( #2929, #33859, #80531, #35856, #5405, #34365 ),
 .UNSPECIFIED., .F., .F.,
 ( 4, 2, 4 ),
 ( 0.000000000000000000, 0.001381509967656051590, 0.002763019935312103180 ),
 .UNSPECIFIED. ) ;
#35411 = COORDINATED_UNIVERSAL_TIME_OFFSET ( 0, 0, .AHEAD. ) ;
#35412 = CARTESIAN_POINT ( 'NONE',  ( -129.5228709571500758, -29.50248528299804818, 1.056150453629047137 ) ) ;
#35413 = CARTESIAN_POINT ( 'NONE',  ( 7.160000000000000142, -6.754662360505033547, 7.925641719537452445 ) ) ;
#35414 = CARTESIAN_POINT ( 'NONE',  ( 19.82558669001425500, -2.195561414069463702, 11.49999999999999645 ) ) ;
#35415 = CARTESIAN_POINT ( 'NONE',  ( -31.52287095715006160, -23.72747288104469732, -1.053458166803228124 ) ) ;
#35416 = CARTESIAN_POINT ( 'NONE',  ( -39.56088531193996261, -23.73791477778911130, 11.05961554403170943 ) ) ;
#35417 = CARTESIAN_POINT ( 'NONE',  ( -48.49451331086643791, -24.34968618360933945, 0.1864209137778883862 ) ) ;
#35418 = ORIENTED_EDGE ( 'NONE', *, *, #9937, .T. ) ;
#35419 = DIRECTION ( 'NONE',  ( 0.7071067811865507924, 0.000000000000000000, -0.7071067811865442421 ) ) ;
#35420 = CARTESIAN_POINT ( 'NONE',  ( -32.40344810634569939, -25.31516574674648368, 3.894478520810415567 ) ) ;
#35421 = CARTESIAN_POINT ( 'NONE',  ( -13.51661872714272405, -17.00040112538478709, -1.500000000000002220 ) ) ;
#35422 = DIRECTION ( 'NONE',  ( -0.000000000000000000, 1.000000000000000000, -0.000000000000000000 ) ) ;
#35423 = CARTESIAN_POINT ( 'NONE',  ( -4.042178566331402045, 19.10766070095605684, -1.500000000000002220 ) ) ;
#35424 = CARTESIAN_POINT ( 'NONE',  ( -55.56003084844635964, -23.85049219812686161, 10.88485053497527133 ) ) ;
#35425 = VERTEX_POINT ( 'NONE', #36576 ) ;
#35426 = APPROVAL_ROLE ( '' ) ;
#35427 = CARTESIAN_POINT ( 'NONE',  ( -69.62287095715005592, -23.72773821059535848, 11.05748984161097503 ) ) ;
#35428 = CARTESIAN_POINT ( 'NONE',  ( 6.539103723289373171, -19.38406401830294712, 11.49999999999999645 ) ) ;
#35429 = DIRECTION ( 'NONE',  ( -0.7071067811865475727, 0.000000000000000000, 0.7071067811865475727 ) ) ;
#35430 = DIRECTION ( 'NONE',  ( -3.773278334453079618E-23, 0.9999999999976377785, 2.173523156925979975E-06 ) ) ;
#35431 = ORIENTED_EDGE ( 'NONE', *, *, #50928, .T. ) ;
#35432 = FACE_OUTER_BOUND ( 'NONE', #18304, .T. ) ;
#35433 = DIRECTION ( 'NONE',  ( -0.1875268396392987258, 0.000000000000000000, -0.9822594791677485837 ) ) ;
#35434 = DIRECTION ( 'NONE',  ( 0.000000000000000000, 0.000000000000000000, 1.000000000000000000 ) ) ;
#35435 = DIRECTION ( 'NONE',  ( 0.000000000000000000, 2.173523156925980399E-06, -0.9999999999976378895 ) ) ;
#35436 = ORIENTED_EDGE ( 'NONE', *, *, #92176, .T. ) ;
#35437 = CARTESIAN_POINT ( 'NONE',  ( 5.817949855437939632, -6.376774720514417183, 20.34349022145623209 ) ) ;
#35438 = VECTOR ( 'NONE', #44771, 1000.000000000000000 ) ;
#35439 = CARTESIAN_POINT ( 'NONE',  ( 5.527175565732886042, -22.34193536506064603, 11.49999999999999645 ) ) ;
#35440 = CARTESIAN_POINT ( 'NONE',  ( -17.61067154241388977, 14.45706175128816184, 11.49999999999998934 ) ) ;
#35441 = CARTESIAN_POINT ( 'NONE',  ( -70.43669851199418019, -25.04371149268589392, 7.560212913825585801 ) ) ;
#35442 = CARTESIAN_POINT ( 'NONE',  ( -28.62287095715006657, -24.50666107542846461, 1.056161637124864550 ) ) ;
#35443 = CARTESIAN_POINT ( 'NONE',  ( 7.160000000000000142, 0.1579206558577708475, 5.788828319098143105 ) ) ;
#35444 = CARTESIAN_POINT ( 'NONE',  ( -70.52287095715009002, -24.52232992886363050, 0.6492154411905990408 ) ) ;
#35445 = CARTESIAN_POINT ( 'NONE',  ( -110.6324688656087432, -23.85016227208580375, -0.8807180028928308646 ) ) ;
#35446 = CARTESIAN_POINT ( 'NONE',  ( -4.983756199382824548, -21.29032736245130053, -1.500000000000002220 ) ) ;
#35447 = LINE ( 'NONE', #74008, #10600 ) ;
#35448 = EDGE_CURVE ( 'NONE', #85219, #96161, #51260, .T. ) ;
#35449 = CYLINDRICAL_SURFACE ( 'NONE', #94641, 3.060000000000000053 ) ;
#35450 = CARTESIAN_POINT ( 'NONE',  ( 6.499999999999992895, 0.9999999999999995559, -2.500000000000001332 ) ) ;
#35451 = CARTESIAN_POINT ( 'NONE',  ( -47.62287095715004881, -23.47593901973091235, -1.443836447539009749 ) ) ;
#35452 = ORIENTED_EDGE ( 'NONE', *, *, #1812, .T. ) ;
#35453 = CIRCLE ( 'NONE', #79247, 1.325999999999990298 ) ;
#35454 = CARTESIAN_POINT ( 'NONE',  ( -8.611577853089924517, -18.50786853157798006, -1.500000000000002220 ) ) ;
#35455 = ORIENTED_EDGE ( 'NONE', *, *, #73851, .T. ) ;
#35456 = ORIENTED_EDGE ( 'NONE', *, *, #84590, .F. ) ;
#35457 = ORIENTED_EDGE ( 'NONE', *, *, #24913, .T. ) ;
#35458 = VERTEX_POINT ( 'NONE', #73160 ) ;
#35459 = CARTESIAN_POINT ( 'NONE',  ( 8.428894486204411507, 21.44871590506140890, 11.49999999999998934 ) ) ;
#35460 = LINE ( 'NONE', #50683, #79465 ) ;
#35461 = CARTESIAN_POINT ( 'NONE',  ( 8.473373031455752269, -18.34320851062214430, -1.500000000000002220 ) ) ;
#35462 = ORIENTED_EDGE ( 'NONE', *, *, #48652, .F. ) ;
#35463 = PLANE ( 'NONE',  #16913 ) ;
#35464 = EDGE_CURVE ( 'NONE', #37139, #96748, #45150, .T. ) ;
#35465 = DIRECTION ( 'NONE',  ( 0.000000000000000000, -1.000000000000000000, 0.000000000000000000 ) ) ;
#35466 = ADVANCED_FACE ( 'NONE', ( #65569 ), #20341, .F. ) ;
#35467 = CARTESIAN_POINT ( 'NONE',  ( 13.10664265030973930, 5.965225279485574461, -27.62597719988137612 ) ) ;
#35468 = CARTESIAN_POINT ( 'NONE',  ( -41.62287095715006302, -23.95044443724991368, 10.65354141964650125 ) ) ;
#35470 = ORIENTED_EDGE ( 'NONE', *, *, #88902, .F. ) ;
#35469 = CARTESIAN_POINT ( 'NONE',  ( 19.34736296927903254, -9.154118057783460216, 11.49999999999999645 ) ) ;
#35471 = DIRECTION ( 'NONE',  ( 1.000000000000000000, 2.567145104884906770E-18, 5.579749332669698856E-24 ) ) ;
#35472 = ADVANCED_FACE ( 'NONE', ( #26975 ), #14316, .T. ) ;
#35473 = ORIENTED_EDGE ( 'NONE', *, *, #6931, .T. ) ;
#35474 = CARTESIAN_POINT ( 'NONE',  ( -16.22183044023116238, -15.26045173261249310, -1.500000000000002220 ) ) ;
#35475 = CARTESIAN_POINT ( 'NONE',  ( -14.21563987850626276, 15.01860006206015008, 11.49999999999998934 ) ) ;
#35477 = CLOSED_SHELL ( 'NONE', ( #49721, #58920, #64736, #63365, #50121, #15852, #39918, #44385, #23634, #42486 ) ) ;
#35476 = ORIENTED_EDGE ( 'NONE', *, *, #31459, .T. ) ;
#35478 = DIRECTION ( 'NONE',  ( 0.000000000000000000, 2.173523156925980399E-06, -0.9999999999976378895 ) ) ;
#35479 = ORIENTED_EDGE ( 'NONE', *, *, #21004, .T. ) ;
#35480 = PLANE ( 'NONE',  #75350 ) ;
#35481 = VERTEX_POINT ( 'NONE', #74639 ) ;
#35482 = CARTESIAN_POINT ( 'NONE',  ( 10.62437663934349530, -3.316774720514425567, -27.03002426119959978 ) ) ;
#35483 = CARTESIAN_POINT ( 'NONE',  ( -7.049398010371669798, 19.71092172866906012, -1.500000000000002220 ) ) ;
#35484 = EDGE_CURVE ( 'NONE', #90130, #90525, #74591, .T. ) ;
#35485 = CARTESIAN_POINT ( 'NONE',  ( -9.857428550561325054, -19.57614489166009264, 11.49999999999999645 ) ) ;
#35486 = CARTESIAN_POINT ( 'NONE',  ( -37.49075569243201755, -24.35071581493542325, 9.817618358456030592 ) ) ;
#35487 = CARTESIAN_POINT ( 'NONE',  ( 9.939345090160914609, -20.19931669485651682, 11.49999999999998934 ) ) ;
#35488 = CARTESIAN_POINT ( 'NONE',  ( 17.15856466979341377, 12.00972951212132855, 11.49999999999998934 ) ) ;
#35489 = CARTESIAN_POINT ( 'NONE',  ( -85.52287095715006160, -29.50250243563736774, 8.947779886222139822 ) ) ;
#35490 = DIRECTION ( 'NONE',  ( 0.7682573101345365751, 0.000000000000000000, -0.6401411605457395515 ) ) ;
#35491 = CARTESIAN_POINT ( 'NONE',  ( -119.5565862188256148, -23.73791477778912551, 11.05961554403169878 ) ) ;
#35492 = LINE ( 'NONE', #43601, #50826 ) ;
#35494 = ORIENTED_EDGE ( 'NONE', *, *, #16116, .T. ) ;
#35493 = EDGE_CURVE ( 'NONE', #95501, #33464, #64580, .T. ) ;
#35495 = VERTEX_POINT ( 'NONE', #77511 ) ;
#35496 = VERTEX_POINT ( 'NONE', #8012 ) ;
#35497 = CARTESIAN_POINT ( 'NONE',  ( -7.160000000000000142, -6.446506136384785535, 8.876977486517731109 ) ) ;
#35498 = B_SPLINE_CURVE_WITH_KNOTS ( 'NONE', 3,
 ( #46221, #16270, #62456, #1056, #38607, #15765 ),
 .UNSPECIFIED., .F., .F.,
 ( 4, 2, 4 ),
 ( 0.000000000000000000, 0.001380764517854765182, 0.002761529035709530365 ),
 .UNSPECIFIED. ) ;
#35499 = ADVANCED_FACE ( 'NONE', ( #54209 ), #59701, .T. ) ;
#35500 = CARTESIAN_POINT ( 'NONE',  ( 19.78805588120126302, 8.271231038663975355, -1.500000000000002220 ) ) ;
#35501 = DIRECTION ( 'NONE',  ( -0.000000000000000000, 1.000000000000000000, -0.000000000000000000 ) ) ;
#35502 = ORIENTED_EDGE ( 'NONE', *, *, #48658, .F. ) ;
#35503 = CARTESIAN_POINT ( 'NONE',  ( 19.97611676871187569, -6.800378171449690257, 11.49999999999998934 ) ) ;
#35504 = CARTESIAN_POINT ( 'NONE',  ( -100.0171587537243596, -25.20430878015014287, 3.360470424028859426 ) ) ;
#35505 = AXIS2_PLACEMENT_3D ( 'NONE', #20083, #74373, #27709 ) ;
#35506 = CARTESIAN_POINT ( 'NONE',  ( 13.59451591917074431, -3.316774720514426456, -28.23515841827053308 ) ) ;
#35508 = CARTESIAN_POINT ( 'NONE',  ( -87.62287095715004170, -23.48783264082478794, -1.443836473390063269 ) ) ;
#35507 = AXIS2_PLACEMENT_3D ( 'NONE', #38794, #91582, #69250 ) ;
#35509 = CARTESIAN_POINT ( 'NONE',  ( 5.851028665930490646, 3.316774720514426011, -27.43979700150094558 ) ) ;
#35510 = DIRECTION ( 'NONE',  ( 0.000000000000000000, 1.000000000000000000, -0.000000000000000000 ) ) ;
#35511 = CARTESIAN_POINT ( 'NONE',  ( -4.445301477617020325, 21.63612927058290936, -1.500000000000002220 ) ) ;
#35512 = FACE_OUTER_BOUND ( 'NONE', #61178, .T. ) ;
#35513 = CARTESIAN_POINT ( 'NONE',  ( -3.108974358974359475, -6.376774720514417183, 20.36458333333334281 ) ) ;
#35514 = CARTESIAN_POINT ( 'NONE',  ( -60.53049054233731852, -24.92564183028978775, 1.928384488918253092 ) ) ;
#35515 = AXIS2_PLACEMENT_3D ( 'NONE', #59814, #29342, #82626 ) ;
#35516 = ADVANCED_FACE ( 'NONE', ( #59940 ), #10097, .T. ) ;
#35517 = CARTESIAN_POINT ( 'NONE',  ( -62.59277029813154059, -24.15620529776627379, 10.23563542870660825 ) ) ;
#35518 = ORIENTED_EDGE ( 'NONE', *, *, #59283, .F. ) ;
#35520 = DIRECTION ( 'NONE',  ( 0.000000000000000000, 1.000000000000000000, 0.000000000000000000 ) ) ;
#35519 = VECTOR ( 'NONE', #19683, 1000.000000000000000 ) ;
#35521 = CARTESIAN_POINT ( 'NONE',  ( -9.778911232092227124, -18.99720643767551209, 11.49999999999998934 ) ) ;
#35522 = CARTESIAN_POINT ( 'NONE',  ( -70.34543693012690824, -25.04307398257883577, 7.563174194274490780 ) ) ;
#35523 = CARTESIAN_POINT ( 'NONE',  ( -49.88527226319177288, -25.31392319263090585, 5.203681702801227438 ) ) ;
#35524 = ADVANCED_FACE ( 'NONE', ( #49596 ), #65828, .T. ) ;
#35525 = DIRECTION ( 'NONE',  ( -0.000000000000000000, -1.000000000000000000, -0.000000000000000000 ) ) ;
#35526 = DIRECTION ( 'NONE',  ( 0.000000000000000000, -0.7071067811865513475, 0.7071067811865437980 ) ) ;
#35527 = CARTESIAN_POINT ( 'NONE',  ( 3.867644355387967359, 22.30990608135428488, -1.500000000000002220 ) ) ;
#35528 = CARTESIAN_POINT ( 'NONE',  ( -47.52287095715006870, -23.96127896942173763, -0.6493128930931011400 ) ) ;
#35529 = EDGE_LOOP ( 'NONE', ( #97128, #97085, #58370, #66425 ) ) ;
#35530 = CARTESIAN_POINT ( 'NONE',  ( -50.65946795233809041, -25.31358068923536564, 5.223679172549864802 ) ) ;
#35531 = LINE ( 'NONE', #50255, #34643 ) ;
#35532 = CARTESIAN_POINT ( 'NONE',  ( 19.26447527235507451, 4.322997736827044690, 11.49999999999999645 ) ) ;
#35533 = DIRECTION ( 'NONE',  ( -3.773278334444166432E-23, 1.000000000000000000, 0.000000000000000000 ) ) ;
#35534 = VECTOR ( 'NONE', #65426, 1000.000000000000000 ) ;
#35535 = CARTESIAN_POINT ( 'NONE',  ( -67.54436619133976194, -24.34968618360932879, 0.1864209137778810865 ) ) ;
#35536 = ORIENTED_EDGE ( 'NONE', *, *, #10631, .T. ) ;
#35537 = CARTESIAN_POINT ( 'NONE',  ( -24.90875734969025501, -5.965225279485572685, 30.51402280011862089 ) ) ;
#35538 = PLANE ( 'NONE',  #23777 ) ;
#35539 = CARTESIAN_POINT ( 'NONE',  ( -100.7619115510279926, -25.12268558752044001, 7.069363477253397754 ) ) ;
#35540 = CARTESIAN_POINT ( 'NONE',  ( 2.319523670979641849, -21.48760272935114557, -1.500000000000002220 ) ) ;
#35541 = CARTESIAN_POINT ( 'NONE',  ( -98.52287095715006160, -29.50247984919015209, -1.443849546365050029 ) ) ;
#35542 = CARTESIAN_POINT ( 'NONE',  ( -66.52287095715006160, -23.48786465467241769, 11.44779295918254647 ) ) ;
#35543 = CARTESIAN_POINT ( 'NONE',  ( -109.5562042904833930, -23.47593901973091235, -1.443836447538999312 ) ) ;
#35544 = DIRECTION ( 'NONE',  ( 0.000000000000000000, 0.000000000000000000, 1.000000000000000000 ) ) ;
#35545 = CARTESIAN_POINT ( 'NONE',  ( -18.77405512783484198, 6.205181830411797606, 11.49999999999998934 ) ) ;
#35546 = VERTEX_POINT ( 'NONE', #64337 ) ;
#35547 = CARTESIAN_POINT ( 'NONE',  ( 20.05935882324986963, -3.104462954613115500, 11.49999999999999645 ) ) ;
#35548 = CARTESIAN_POINT ( 'NONE',  ( 3.252401863874215593, 0.3587747205143964613, -29.35688408629929214 ) ) ;
#35549 = AXIS2_PLACEMENT_3D ( 'NONE', #7190, #15302, #31032 ) ;
#35550 = CARTESIAN_POINT ( 'NONE',  ( 5.811591729264017125, -6.376774720514422512, 21.22699980322195046 ) ) ;
#35551 = ORIENTED_EDGE ( 'NONE', *, *, #63314, .F. ) ;
#35552 = B_SPLINE_SURFACE_WITH_KNOTS ( 'NONE', 3, 3, ( 
 ( #96069, #32158, #71235, #78818 ),
 ( #2731, #1722, #10328, #26563 ),
 ( #63637, #64144, #41797, #79830 ),
 ( #40776, #94558, #25552, #72740 ),
 ( #86450, #72237, #8829, #95564 ),
 ( #9826, #56521, #39766, #71738 ),
 ( #33668, #64649, #70728, #1224 ),
 ( #26048, #63131, #94057, #24543 ),
 ( #57021, #55516, #41281, #9314 ),
 ( #87959, #40280, #18438, #32660 ) ),
 .UNSPECIFIED., .F., .F., .F.,
 ( 4, 3, 3, 4 ),
 ( 4, 4 ),
 ( 0.7022005934544808259, 0.7765311282028797280, 0.8508616629512786300, 0.9995227324480764342 ),
 ( 0.5495603210497661539, 0.5509005761542268287 ),
 .UNSPECIFIED. ) ;
#35553 = DIRECTION ( 'NONE',  ( 3.773278334444167608E-23, -1.000000000000000000, 0.000000000000000000 ) ) ;
#35554 = CARTESIAN_POINT ( 'NONE',  ( -107.5228709571500758, -23.47596703998600631, 11.44779298504228038 ) ) ;
#35555 = DIRECTION ( 'NONE',  ( -3.773278334453079030E-23, 0.9999999999976377785, 2.173523156925979128E-06 ) ) ;
#35556 = CARTESIAN_POINT ( 'NONE',  ( -45.62287095715004881, -29.50247984919015209, -1.443849546365058689 ) ) ;
#35557 = CARTESIAN_POINT ( 'NONE',  ( -51.52472467211992324, -25.24108473429059885, 6.254983020916855097 ) ) ;
#35558 = CARTESIAN_POINT ( 'NONE',  ( 9.011679573027636891, 17.89655708981447901, -1.500000000000002220 ) ) ;
#35559 = CARTESIAN_POINT ( 'NONE',  ( 6.600000000000001421, 0.000000000000000000, 0.000000000000000000 ) ) ;
#35560 = ORIENTED_EDGE ( 'NONE', *, *, #52774, .F. ) ;
#35561 = B_SPLINE_CURVE_WITH_KNOTS ( 'NONE', 3,
 ( #59984, #28028, #44256, #12784, #74688, #75677 ),
 .UNSPECIFIED., .F., .F.,
 ( 4, 2, 4 ),
 ( 6.391158118967745954E-06, 0.001387004593080785496, 0.002767618028042603297 ),
 .UNSPECIFIED. ) ;
#35562 = CARTESIAN_POINT ( 'NONE',  ( -32.62287095715004881, -23.48786465467240347, 11.44779295918255535 ) ) ;
#35563 = CARTESIAN_POINT ( 'NONE',  ( -115.5228709571500616, -23.48783264082477018, -1.443836473390083475 ) ) ;
#35564 = DIRECTION ( 'NONE',  ( -0.000000000000000000, -1.000000000000000000, -0.000000000000000000 ) ) ;
#35565 = LINE ( 'NONE', #33560, #15669 ) ;
#35566 = LINE ( 'NONE', #68016, #26763 ) ;
#35567 = CARTESIAN_POINT ( 'NONE',  ( -71.55620429048339304, -24.66019654487199375, 8.947790411086131712 ) ) ;
#35568 = VERTEX_POINT ( 'NONE', #96751 ) ;
#35569 = EDGE_CURVE ( 'NONE', #1158, #24982, #56714, .T. ) ;
#35570 = CARTESIAN_POINT ( 'NONE',  ( 16.70477854660759931, 11.60849435585976153, 11.49999999999998934 ) ) ;
#35572 = EDGE_CURVE ( 'NONE', #65047, #24849, #80527, .T. ) ;
#35571 = ORIENTED_EDGE ( 'NONE', *, *, #90946, .T. ) ;
#35573 = CARTESIAN_POINT ( 'NONE',  ( 19.00551534866085746, 12.86435971046890359, 11.49999999999998934 ) ) ;
#35574 = CARTESIAN_POINT ( 'NONE',  ( -32.58048861069256930, -24.51314013834315375, 0.6176544820404111791 ) ) ;
#35575 = EDGE_CURVE ( 'NONE', #4586, #97579, #19792, .T. ) ;
#35576 = ORIENTED_EDGE ( 'NONE', *, *, #67090, .F. ) ;
#35577 = AXIS2_PLACEMENT_3D ( 'NONE', #83879, #20976, #14360 ) ;
#35578 = CARTESIAN_POINT ( 'NONE',  ( -49.41394411914537699, -25.30232982750377246, 4.714210424874468508 ) ) ;
#35579 = EDGE_CURVE ( 'NONE', #654, #48919, #47087, .T. ) ;
#35580 = CARTESIAN_POINT ( 'NONE',  ( -49.27764846858840997, -25.12215211752863198, 6.145205272392983531 ) ) ;
#35581 = AXIS2_PLACEMENT_3D ( 'NONE', #4740, #35688, #42814 ) ;
#35582 = DIRECTION ( 'NONE',  ( -1.000000000000000000, -0.000000000000000000, -0.000000000000000000 ) ) ;
#35583 = CARTESIAN_POINT ( 'NONE',  ( 18.66760434907605060, -10.05535386721697222, 11.49999999999999645 ) ) ;
#35584 = CIRCLE ( 'NONE', #4804, 83.21379343477475743 ) ;
#35585 = ORIENTED_EDGE ( 'NONE', *, *, #71554, .F. ) ;
#35586 = CARTESIAN_POINT ( 'NONE',  ( -12.04397493737346991, 18.63154960201688226, 11.49999999999998934 ) ) ;
#35587 = CARTESIAN_POINT ( 'NONE',  ( 20.22723401096548201, -3.897675682603606084, 11.49999999999998934 ) ) ;
#35589 = ORIENTED_EDGE ( 'NONE', *, *, #66648, .T. ) ;
#35588 = TOROIDAL_SURFACE ( 'NONE', #92293, 19.00000000000000355, 1.000000000000000000 ) ;
#35590 = VERTEX_POINT ( 'NONE', #71934 ) ;
#35591 = CARTESIAN_POINT ( 'NONE',  ( -61.52287095715006160, -23.47596703998600631, 11.44779298504228926 ) ) ;
#35592 = EDGE_CURVE ( 'NONE', #9229, #46643, #64995, .T. ) ;
#35593 = CARTESIAN_POINT ( 'NONE',  ( -113.6228709571500559, -29.50250243563736774, 8.947779886222136270 ) ) ;
#35594 = ORIENTED_EDGE ( 'NONE', *, *, #77743, .T. ) ;
#35595 = ORIENTED_EDGE ( 'NONE', *, *, #88958, .F. ) ;
#35596 = APPLICATION_CONTEXT ( 'configuration controlled 3d designs of mechanical parts and assemblies' ) ;
#35597 = VERTEX_POINT ( 'NONE', #71426 ) ;
#35598 = FACE_OUTER_BOUND ( 'NONE', #129, .T. ) ;
#35599 = CARTESIAN_POINT ( 'NONE',  ( -28.62169072633495404, -23.33141450733164390, 11.44779300624183982 ) ) ;
#35600 = CARTESIAN_POINT ( 'NONE',  ( -119.5562042904834072, -23.48783264082478794, -1.443836473390058384 ) ) ;
#35601 = CARTESIAN_POINT ( 'NONE',  ( 12.20387445076365296, 16.77033177596414504, -1.500000000000002220 ) ) ;
#35602 = CARTESIAN_POINT ( 'NONE',  ( 18.07971092720299922, 12.08445254275838465, 11.49999999999999645 ) ) ;
#35603 = ORIENTED_EDGE ( 'NONE', *, *, #71265, .F. ) ;
#35604 = CARTESIAN_POINT ( 'NONE',  ( -121.6228709571500417, -23.47593901973091235, -1.443836447538997536 ) ) ;
#35605 = CARTESIAN_POINT ( 'NONE',  ( -115.5550176680797847, -24.15503026093914940, -0.2815557561904543094 ) ) ;
#35606 = CARTESIAN_POINT ( 'NONE',  ( -21.67104271438225638, 5.786422744429515319, 11.49999999999998934 ) ) ;
#35607 = CARTESIAN_POINT ( 'NONE',  ( 6.660000000000001030, -9.572916487583196243, -0.7764348688322058045 ) ) ;
#35608 = CARTESIAN_POINT ( 'NONE',  ( -65.49048155462992327, -24.73486907724918282, 1.287355809206962354 ) ) ;
#35609 = ORIENTED_EDGE ( 'NONE', *, *, #68826, .T. ) ;
#35610 = CARTESIAN_POINT ( 'NONE',  ( 10.86264265030973952, -0.3587747205144257157, -27.62597719988137612 ) ) ;
#35611 = CARTESIAN_POINT ( 'NONE',  ( -38.62287095715005592, -29.50250243563736774, 8.947779886222148704 ) ) ;
#35612 = ORIENTED_EDGE ( 'NONE', *, *, #49113, .T. ) ;
#35613 = VERTEX_POINT ( 'NONE', #88151 ) ;
#35614 = CARTESIAN_POINT ( 'NONE',  ( 8.499999999999989342, 18.74999999999999645, 2.100000000000000089 ) ) ;
#35615 = EDGE_LOOP ( 'NONE', ( #21297, #64594, #86854, #87810, #95761, #99691, #54305, #817, #93887, #80026, #12864, #50434, #40813, #62926, #6883, #6399, #91186, #30458 ) ) ;
#35616 = CARTESIAN_POINT ( 'NONE',  ( 21.17668642892995834, 2.279540523802085605, -1.500000000000002220 ) ) ;
#35617 = VERTEX_POINT ( 'NONE', #57219 ) ;
#35618 = CARTESIAN_POINT ( 'NONE',  ( -88.58338540734003175, -24.65952944569304606, 1.056160979905700126 ) ) ;
#35619 = CARTESIAN_POINT ( 'NONE',  ( 9.643594380127815668, 19.59848315111488759, 11.49999999999998934 ) ) ;
#35620 = CARTESIAN_POINT ( 'NONE',  ( -124.5228709571500616, -23.47596703998600631, 11.44779298504227860 ) ) ;
#35621 = CARTESIAN_POINT ( 'NONE',  ( 7.379361219544559702, 21.46082085352547963, -1.500000000000002220 ) ) ;
#35622 = CARTESIAN_POINT ( 'NONE',  ( -41.01720553446741491, -25.28892453938848561, 3.440463365724605982 ) ) ;
#35623 = CARTESIAN_POINT ( 'NONE',  ( 5.705253819860196529, -5.876774720514416295, 19.95963554344900714 ) ) ;
#35624 = CARTESIAN_POINT ( 'NONE',  ( 21.83198049998918577, 2.282343850347359648, -1.500000000000002220 ) ) ;
#35625 = DIRECTION ( 'NONE',  ( 0.000000000000000000, 1.000000000000000000, 0.000000000000000000 ) ) ;
#35626 = VERTEX_POINT ( 'NONE', #88651 ) ;
#35627 = CARTESIAN_POINT ( 'NONE',  ( -122.6256518724121349, -23.96169478059714564, 10.65365249895717170 ) ) ;
#35628 = CARTESIAN_POINT ( 'NONE',  ( -49.13273521788515552, -25.26337483015602814, 6.968846308470279638 ) ) ;
#35629 = EDGE_CURVE ( 'NONE', #27877, #61563, #3988, .T. ) ;
#35630 = ORIENTED_EDGE ( 'NONE', *, *, #16568, .T. ) ;
#35631 = CARTESIAN_POINT ( 'NONE',  ( -30.59802378171020720, -24.75939178235423910, 8.616593176194657033 ) ) ;
#35632 = CARTESIAN_POINT ( 'NONE',  ( 6.671786015990716301, 6.475225279485573360, -27.29955796265488033 ) ) ;
#35633 = CARTESIAN_POINT ( 'NONE',  ( -20.38992538795168130, -24.51867817427762120, 3.856996771330998719 ) ) ;
#35634 = CARTESIAN_POINT ( 'NONE',  ( 1.567330217057175901, -21.20382687294985047, 11.49999999999998934 ) ) ;
#35635 = CARTESIAN_POINT ( 'NONE',  ( -112.5515245461530469, -24.51314013834317151, 0.6176544820404297198 ) ) ;
#35636 = CARTESIAN_POINT ( 'NONE',  ( -26.17837527425876942, -24.75186326096774536, 3.912474607469140775 ) ) ;
#35638 = EDGE_CURVE ( 'NONE', #30854, #16991, #50093, .T. ) ;
#35637 = VECTOR ( 'NONE', #22909, 1000.000000000000000 ) ;
#35639 = CARTESIAN_POINT ( 'NONE',  ( -85.58384127135377639, -24.83618233451450408, 1.606449574219535270 ) ) ;
#35640 = CARTESIAN_POINT ( 'NONE',  ( -129.5228709571501327, -23.96127896941634106, -0.6493128931037915885 ) ) ;
#35641 = CARTESIAN_POINT ( 'NONE',  ( -32.55620429048338593, -23.47593901973091235, -1.443836447539013301 ) ) ;
#35642 = ORIENTED_EDGE ( 'NONE', *, *, #65306, .F. ) ;
#35643 = CARTESIAN_POINT ( 'NONE',  ( 17.64699390344983598, -8.409456921668478913, 11.49999999999999645 ) ) ;
#35644 = LINE ( 'NONE', #35147, #34136 ) ;
#35645 = VECTOR ( 'NONE', #91979, 1000.000000000000227 ) ;
#35646 = CARTESIAN_POINT ( 'NONE',  ( -79.35273227324233858, -25.25510918649008829, 6.111704383075113434 ) ) ;
#35647 = ORIENTED_EDGE ( 'NONE', *, *, #35572, .F. ) ;
#35648 = CARTESIAN_POINT ( 'NONE',  ( 14.76093561896379214, -5.965225279485572685, -27.88148769130088667 ) ) ;
#35649 = CARTESIAN_POINT ( 'NONE',  ( -101.3289322354959836, -25.08272168729980223, 7.323006979996904420 ) ) ;
#35650 = VECTOR ( 'NONE', #42381, 1000.000000000000114 ) ;
#35651 = CARTESIAN_POINT ( 'NONE',  ( -42.58953762381671737, -23.48783264082477373, -1.443836473390072817 ) ) ;
#35652 = FACE_OUTER_BOUND ( 'NONE', #90361, .T. ) ;
#35653 = CARTESIAN_POINT ( 'NONE',  ( 16.13486940644654766, 11.28601765141728741, -1.500000000000002220 ) ) ;
#35654 = AXIS2_PLACEMENT_3D ( 'NONE', #55935, #41204, #64563 ) ;
#35655 = VERTEX_POINT ( 'NONE', #33855 ) ;
#35656 = AXIS2_PLACEMENT_3D ( 'NONE', #22800, #1500, #53786 ) ;
#35657 = LINE ( 'NONE', #97543, #32664 ) ;
#35658 = CARTESIAN_POINT ( 'NONE',  ( 30.59073162224239084, -4.540774720514408891, 26.30400772315274338 ) ) ;
#35659 = AXIS2_PLACEMENT_3D ( 'NONE', #68444, #75041, #5537 ) ;
#35660 = DATE_AND_TIME ( #96547, #34491 ) ;
#35661 = VERTEX_POINT ( 'NONE', #56211 ) ;
#35662 = CARTESIAN_POINT ( 'NONE',  ( -107.5895376238167387, -24.64965694238407679, 8.947790433994649462 ) ) ;
#35663 = CARTESIAN_POINT ( 'NONE',  ( -45.62287095715005592, -24.63345952396255711, 9.038047939301497635 ) ) ;
#35664 = CARTESIAN_POINT ( 'NONE',  ( -123.6228709571500559, -29.50250786944525672, 11.44777988621622811 ) ) ;
#35665 = FACE_OUTER_BOUND ( 'NONE', #72174, .T. ) ;
#35666 = CARTESIAN_POINT ( 'NONE',  ( -89.52287095715006160, -23.48786465467241769, 11.44779295918254292 ) ) ;
#35667 = CARTESIAN_POINT ( 'NONE',  ( -70.35895856474228083, -25.31201590484430142, 5.313173609717679824 ) ) ;
#35668 = CARTESIAN_POINT ( 'NONE',  ( -107.5907586917641083, -24.15543982623907837, -0.2315651400026443874 ) ) ;
#35669 = CARTESIAN_POINT ( 'NONE',  ( -4.495603250223349612, -19.44740727768710187, -1.500000000000002220 ) ) ;
#35670 = LINE ( 'NONE', #56649, #11045 ) ;
#35671 = CARTESIAN_POINT ( 'NONE',  ( -0.03708603945156426634, -22.56989207558077126, 1.621508199058790511 ) ) ;
#35672 = ORIENTED_EDGE ( 'NONE', *, *, #5693, .T. ) ;
#35673 = CARTESIAN_POINT ( 'NONE',  ( -63.52287095715007581, -24.50216790748205042, 0.6166512839542489521 ) ) ;
#35674 = CARTESIAN_POINT ( 'NONE',  ( 4.653494883475234545, -5.876774720514415407, 20.13747874360300116 ) ) ;
#35675 = EDGE_CURVE ( 'NONE', #18738, #87632, #42491, .T. ) ;
#35676 = CARTESIAN_POINT ( 'NONE',  ( 8.655157120194559184, -6.376774720514430506, -28.10018424674326099 ) ) ;
#35677 = CARTESIAN_POINT ( 'NONE',  ( -126.1689479211560183, -25.21288074133898505, 6.500980345380262371 ) ) ;
#35678 = PLANE ( 'NONE',  #19228 ) ;
#35679 = CARTESIAN_POINT ( 'NONE',  ( -64.52287095715006160, -24.65952944569304606, 1.056160979905695463 ) ) ;
#35680 = CARTESIAN_POINT ( 'NONE',  ( 12.92500000000000249, 14.50000000000000000, 24.00000000000000000 ) ) ;
#35681 = ORIENTED_EDGE ( 'NONE', *, *, #76347, .F. ) ;
#35682 = DIRECTION ( 'NONE',  ( -1.000000000000000000, -3.773278334444167608E-23, -8.201307833595939069E-29 ) ) ;
#35683 = CARTESIAN_POINT ( 'NONE',  ( 6.371704462700114924, -5.876774720514426953, 21.83798798526824214 ) ) ;
#35684 = ORIENTED_EDGE ( 'NONE', *, *, #21233, .F. ) ;
#35685 = EDGE_CURVE ( 'NONE', #77233, #98717, #11351, .T. ) ;
#35686 = CARTESIAN_POINT ( 'NONE',  ( -2.479824388263708990, 20.08073137130260122, -1.500000000000002220 ) ) ;
#35687 = CARTESIAN_POINT ( 'NONE',  ( -43.55620429048337883, -23.48783264082477373, -1.443836473390070596 ) ) ;
#35688 = DIRECTION ( 'NONE',  ( -0.000000000000000000, -1.000000000000000000, -0.000000000000000000 ) ) ;
#35689 = ADVANCED_FACE ( 'NONE', ( #19120 ), #18130, .T. ) ;
#35690 = CARTESIAN_POINT ( 'NONE',  ( -50.62287095715005592, -29.50250786944525672, 11.44777988621624054 ) ) ;
#35691 = ADVANCED_FACE ( 'NONE', ( #48602 ), #79525, .T. ) ;
#35692 = EDGE_LOOP ( 'NONE', ( #10085, #6612, #89511, #5032 ) ) ;
#35693 = CARTESIAN_POINT ( 'NONE',  ( -46.62287095715004881, -24.64965695001467694, 8.947790433994185832 ) ) ;
#35694 = CARTESIAN_POINT ( 'NONE',  ( -52.52287095715009002, -24.51387760970726148, 9.387446482453432495 ) ) ;
#35695 = CARTESIAN_POINT ( 'NONE',  ( 19.65109224456760728, -3.968444974485820786, -1.500000000000002220 ) ) ;
#35696 = EDGE_CURVE ( 'NONE', #17632, #12369, #54854, .T. ) ;
#35697 = CARTESIAN_POINT ( 'NONE',  ( 4.297136154115697160, 20.59472113332480703, 11.49999999999999645 ) ) ;
#35698 = CARTESIAN_POINT ( 'NONE',  ( -0.02075734969026423599, 5.965225279485572685, -0.08597719988137648983 ) ) ;
#35699 = CARTESIAN_POINT ( 'NONE',  ( -111.6228709571500843, -23.47596703998600631, 11.44779298504227860 ) ) ;
#35700 = CARTESIAN_POINT ( 'NONE',  ( -7.692412698405892257, 20.70400481474656118, 11.49999999999998934 ) ) ;
#35701 = EDGE_CURVE ( 'NONE', #75743, #70312, #35780, .T. ) ;
#35702 = VECTOR ( 'NONE', #80769, 1000.000000000000000 ) ;
#35703 = CARTESIAN_POINT ( 'NONE',  ( -40.31138024738270786, -25.27806106079862403, 5.079523691001327279 ) ) ;
#35704 = CARTESIAN_POINT ( 'NONE',  ( -76.62287095715007013, -23.47593901973091235, -1.443836447539004642 ) ) ;
#35705 = LINE ( 'NONE', #96108, #50903 ) ;
#35706 = ORIENTED_EDGE ( 'NONE', *, *, #76878, .F. ) ;
#35707 = DIRECTION ( 'NONE',  ( -3.773278334453080206E-23, 0.9999999999976377785, 2.173523156925979975E-06 ) ) ;
#35708 = B_SPLINE_CURVE_WITH_KNOTS ( 'NONE', 3,
 ( #21982, #76763, #92007, #22478 ),
 .UNSPECIFIED., .F., .F.,
 ( 4, 4 ),
 ( 0.6459941988912109023, 0.6543842573219610381 ),
 .UNSPECIFIED. ) ;
#35709 = CARTESIAN_POINT ( 'NONE',  ( -31.62287095715005947, -23.96127896941631619, -0.6493128931037948082 ) ) ;
#35710 = ORIENTED_EDGE ( 'NONE', *, *, #100353, .T. ) ;
#35711 = EDGE_LOOP ( 'NONE', ( #27152, #92033, #35045, #44585, #70280, #77199 ) ) ;
#35712 = CARTESIAN_POINT ( 'NONE',  ( -43.52287095715006160, -23.47596703998600631, 11.44779298504229281 ) ) ;
#35713 = DIRECTION ( 'NONE',  ( -0.000000000000000000, 1.000000000000000000, -0.000000000000000000 ) ) ;
#35715 = EDGE_CURVE ( 'NONE', #46190, #78417, #57397, .T. ) ;
#35714 = CARTESIAN_POINT ( 'NONE',  ( -76.59214954560788158, -24.15543982623907482, -0.2315651400026599305 ) ) ;
#35716 = CARTESIAN_POINT ( 'NONE',  ( 4.697267095454844998, -20.06606415395816967, -1.500000000000002220 ) ) ;
#35717 = CARTESIAN_POINT ( 'NONE',  ( -19.35566633068252074, -9.524217769563914970, 11.49999999999999645 ) ) ;
#35718 = VERTEX_POINT ( 'NONE', #90139 ) ;
#35719 = CARTESIAN_POINT ( 'NONE',  ( -91.63415237563449978, -23.96119346886881019, -0.6495511937832073590 ) ) ;
#35720 = DIRECTION ( 'NONE',  ( 3.773278334444167608E-23, -1.000000000000000000, 0.000000000000000000 ) ) ;
#35721 = PLANE ( 'NONE',  #93381 ) ;
#35722 = CARTESIAN_POINT ( 'NONE',  ( 18.00092565640838416, -13.26076702590692769, -1.500000000000002220 ) ) ;
#35723 = CARTESIAN_POINT ( 'NONE',  ( -59.62287095715007013, -23.73934037231756733, 11.05740245334329153 ) ) ;
#35724 = CARTESIAN_POINT ( 'NONE',  ( 282.9764569301858046, -4.540774720514427543, 20.79159422840526616 ) ) ;
#35725 = EDGE_LOOP ( 'NONE', ( #37734, #40924, #55470, #5492 ) ) ;
#35726 = LINE ( 'NONE', #5762, #92279 ) ;
#35727 = VECTOR ( 'NONE', #94248, 1000.000000000000000 ) ;
#35728 = CARTESIAN_POINT ( 'NONE',  ( -51.37905358277658507, -25.30232438542244466, 4.713790514697788758 ) ) ;
#35729 = AXIS2_PLACEMENT_3D ( 'NONE', #1870, #10979, #19079 ) ;
#35730 = CARTESIAN_POINT ( 'NONE',  ( -11.44352472427880052, 17.46665840655709090, -1.500000000000002220 ) ) ;
#35731 = ORIENTED_EDGE ( 'NONE', *, *, #66445, .F. ) ;
#35733 = VERTEX_POINT ( 'NONE', #5893 ) ;
#35732 = CARTESIAN_POINT ( 'NONE',  ( -39.98807537358911190, -25.12223002584979881, 2.898744922101010424 ) ) ;
#35734 = ORIENTED_EDGE ( 'NONE', *, *, #78526, .T. ) ;
#35735 = VECTOR ( 'NONE', #42026, 1000.000000000000114 ) ;
#35736 = CARTESIAN_POINT ( 'NONE',  ( -100.5143450367917808, -24.15602025860896163, 10.28564288303535790 ) ) ;
#35737 = CARTESIAN_POINT ( 'NONE',  ( -20.28541985502614509, -5.886007371444655689, -1.500000000000002220 ) ) ;
#35738 = VECTOR ( 'NONE', #99324, 1000.000000000000000 ) ;
#35739 = VERTEX_POINT ( 'NONE', #51584 ) ;
#35740 = CARTESIAN_POINT ( 'NONE',  ( -91.55620429048339304, -24.66019654487199375, 8.947790411086124607 ) ) ;
#35741 = CARTESIAN_POINT ( 'NONE',  ( -58.52287095715004739, -23.48783264082477018, -1.443836473390092801 ) ) ;
#35742 = CARTESIAN_POINT ( 'NONE',  ( -117.6228709571500559, -29.50250243563736774, 8.947779886222134493 ) ) ;
#35743 = CARTESIAN_POINT ( 'NONE',  ( -28.55620429048340370, -23.31439381047619008, -1.443835771460519890 ) ) ;
#35744 = CARTESIAN_POINT ( 'NONE',  ( 7.141559373243376641, -5.876774720514415407, 19.83742167145384983 ) ) ;
#35745 = CARTESIAN_POINT ( 'NONE',  ( 9.899741330608472722, -19.37759744025533593, -1.500000000000002220 ) ) ;
#35746 = DIRECTION ( 'NONE',  ( 0.000000000000000000, -1.000000000000000000, 0.000000000000000000 ) ) ;
#35748 = ORIENTED_EDGE ( 'NONE', *, *, #95135, .T. ) ;
#35747 = CARTESIAN_POINT ( 'NONE',  ( 13.23790625878087468, -17.95846084735695314, 11.49999999999999645 ) ) ;
#35749 = LINE ( 'NONE', #91509, #98792 ) ;
#35750 = CARTESIAN_POINT ( 'NONE',  ( 6.910430652544937935, -6.376774720514418959, 20.24472806504191169 ) ) ;
#35751 = EDGE_CURVE ( 'NONE', #29704, #30337, #34114, .T. ) ;
#35752 = DIRECTION ( 'NONE',  ( -0.000000000000000000, 2.173523156925979552E-06, -0.9999999999976378895 ) ) ;
#35753 = ORIENTED_EDGE ( 'NONE', *, *, #78084, .F. ) ;
#35755 = ORIENTED_EDGE ( 'NONE', *, *, #85977, .T. ) ;
#35754 = CARTESIAN_POINT ( 'NONE',  ( -54.62287095715005592, -24.66019654487199020, 8.947790411086135265 ) ) ;
#35756 = EDGE_CURVE ( 'NONE', #35375, #53340, #16201, .T. ) ;
#35757 = ORIENTED_EDGE ( 'NONE', *, *, #72821, .F. ) ;
#35758 = CARTESIAN_POINT ( 'NONE',  ( 32.16024265030974050, -0.3587747205144265483, 16.27760796525321751 ) ) ;
#35759 = CARTESIAN_POINT ( 'NONE',  ( -86.62287095715001328, -23.47596703998600631, 11.44779298504227683 ) ) ;
#35760 = CARTESIAN_POINT ( 'NONE',  ( -90.52287095715006160, -29.50247984919015209, -1.443849546365051806 ) ) ;
#35761 = CARTESIAN_POINT ( 'NONE',  ( -35.52287095715009713, -24.51163499207175889, 0.6490370598554275894 ) ) ;
#35762 = EDGE_CURVE ( 'NONE', #4160, #50305, #41558, .T. ) ;
#35763 = CARTESIAN_POINT ( 'NONE',  ( 32.42932432802503939, -5.965225279485572685, -0.2107846672978405389 ) ) ;
#35764 = EDGE_LOOP ( 'NONE', ( #24525, #44085, #68120, #47940 ) ) ;
#35765 = CARTESIAN_POINT ( 'NONE',  ( -17.02366064725396555, -9.230830265533395362, 11.49999999999999645 ) ) ;
#35766 = CARTESIAN_POINT ( 'NONE',  ( -88.52287095715006160, -23.47596703998600631, 11.44779298504228393 ) ) ;
#35767 = EDGE_CURVE ( 'NONE', #89034, #33339, #6507, .T. ) ;
#35768 = ORIENTED_EDGE ( 'NONE', *, *, #10061, .F. ) ;
#35769 = CARTESIAN_POINT ( 'NONE',  ( 3.121233215686890272, -6.376774720514404748, 18.93204046835445808 ) ) ;
#35770 = CARTESIAN_POINT ( 'NONE',  ( 9.214646252612421762, 3.316774720514544583, -27.04520690475792222 ) ) ;
#35771 = CYLINDRICAL_SURFACE ( 'NONE', #95173, 1.250000000000001998 ) ;
#35772 = CARTESIAN_POINT ( 'NONE',  ( -30.61342099046267862, -24.26827793580485704, 9.960784317162946877 ) ) ;
#35773 = CARTESIAN_POINT ( 'NONE',  ( -15.04504930077994196, -12.58455232801425794, 11.49999999999998934 ) ) ;
#35774 = CARTESIAN_POINT ( 'NONE',  ( -116.5895376238167103, -24.65952944569305316, 1.056160979905705455 ) ) ;
#35775 = ORIENTED_EDGE ( 'NONE', *, *, #91797, .T. ) ;
#35776 = CARTESIAN_POINT ( 'NONE',  ( 4.073501596442082651, -21.17334570714589859, 11.49999999999998934 ) ) ;
#35777 = CARTESIAN_POINT ( 'NONE',  ( -37.62287095715005592, -23.47593901973091235, -1.443836447539011525 ) ) ;
#35778 = CARTESIAN_POINT ( 'NONE',  ( -81.37613735670856840, -25.31572692185423534, 5.179459861000572651 ) ) ;
#35779 = LINE ( 'NONE', #20046, #21650 ) ;
#35780 = CIRCLE ( 'NONE', #90821, 129.7684398600581517 ) ;
#35781 = FACE_OUTER_BOUND ( 'NONE', #40185, .T. ) ;
#35782 = CARTESIAN_POINT ( 'NONE',  ( -2.116611060711651504, 22.89395876494169002, -1.500000000000002220 ) ) ;
#35783 = CC_DESIGN_DATE_AND_TIME_ASSIGNMENT ( #92050, #204, ( #34522 ) ) ;
#35784 = COORDINATED_UNIVERSAL_TIME_OFFSET ( 0, 0, .AHEAD. ) ;
#35785 = CARTESIAN_POINT ( 'NONE',  ( 30.00738719773716312, -1.477225279485574028, -9.049252915307087974 ) ) ;
#35786 = CARTESIAN_POINT ( 'NONE',  ( -16.67386609800740516, 11.36076560755915033, 11.49999999999999645 ) ) ;
#35787 = CARTESIAN_POINT ( 'NONE',  ( -108.9559085688801616, -25.10927677356297139, 4.125626278649611400 ) ) ;
#35788 = CARTESIAN_POINT ( 'NONE',  ( 25.61870917940689196, 5.965225279485572685, 29.49402280011862487 ) ) ;
#35789 = CARTESIAN_POINT ( 'NONE',  ( 27.86270917940689174, -0.3587747205144265483, 29.49402280011862487 ) ) ;
#35790 = FACE_OUTER_BOUND ( 'NONE', #54096, .T. ) ;
#35791 = LINE ( 'NONE', #72361, #86698 ) ;
#35792 = CARTESIAN_POINT ( 'NONE',  ( 10.41257876278241845, -16.90412932818451353, -1.500000000000002220 ) ) ;
#35793 = CARTESIAN_POINT ( 'NONE',  ( -113.5881261692640152, -24.51314013834316086, 0.6176544820404182845 ) ) ;
#35794 = CARTESIAN_POINT ( 'NONE',  ( 19.18734209777730015, 4.435579877058994036, -1.500000000000002220 ) ) ;
#35795 = CARTESIAN_POINT ( 'NONE',  ( -42.48688622151200178, -24.51314013834315375, 0.6176544820404090697 ) ) ;
#35796 = AXIS2_PLACEMENT_3D ( 'NONE', #56062, #72784, #64188 ) ;
#35797 = CARTESIAN_POINT ( 'NONE',  ( -4.968349358974361252, -6.376774720514411854, 19.46153846153847056 ) ) ;
#35798 = CARTESIAN_POINT ( 'NONE',  ( -100.5228709571500616, -23.48786465467242479, 11.44779295918254114 ) ) ;
#35799 = CARTESIAN_POINT ( 'NONE',  ( 3.034461355793923509, -20.43525710956717845, 11.49999999999999645 ) ) ;
#35800 = CARTESIAN_POINT ( 'NONE',  ( 30.56408408303725466, -2.971977064529662371, 24.90465250750439097 ) ) ;
#35802 = B_SPLINE_CURVE_WITH_KNOTS ( 'NONE', 3,
 ( #66072, #98472, #75633, #20851, #21844, #91369 ),
 .UNSPECIFIED., .F., .F.,
 ( 4, 2, 4 ),
 ( 0.000000000000000000, 0.001380764517854759978, 0.002761529035709519957 ),
 .UNSPECIFIED. ) ;
#35801 = DIRECTION ( 'NONE',  ( 0.000000000000000000, 0.000000000000000000, 1.000000000000000000 ) ) ;
#35803 = CARTESIAN_POINT ( 'NONE',  ( -22.46375958613465684, 3.124547546656453179, 11.49999999999999645 ) ) ;
#35804 = ORIENTED_EDGE ( 'NONE', *, *, #57378, .F. ) ;
#35805 = CARTESIAN_POINT ( 'NONE',  ( 32.73857899460460175, -6.475225279485576024, -13.20677013500359820 ) ) ;
#35806 = CARTESIAN_POINT ( 'NONE',  ( 30.59299694858157892, 5.371884064401012182, 26.41087035901067637 ) ) ;
#35807 = EDGE_CURVE ( 'NONE', #5267, #77096, #27743, .T. ) ;
#35808 = CARTESIAN_POINT ( 'NONE',  ( -63.59779725530248840, -23.96119346886879953, -0.6495511937832106897 ) ) ;
#35809 = CARTESIAN_POINT ( 'NONE',  ( -45.52287095715006160, -25.00158670708908915, 2.256160236439166411 ) ) ;
#35810 = EDGE_LOOP ( 'NONE', ( #50181, #97802, #42366, #92592 ) ) ;
#35811 = ORIENTED_EDGE ( 'NONE', *, *, #46594, .T. ) ;
#35812 = CARTESIAN_POINT ( 'NONE',  ( -44.62287095715004881, -29.50247984919015209, -1.443849546365060466 ) ) ;
#35813 = CARTESIAN_POINT ( 'NONE',  ( 4.181975289622855918, -22.47981636197143374, -1.500000000000002220 ) ) ;
#35814 = CARTESIAN_POINT ( 'NONE',  ( -29.57133676521425514, -23.40473823521239183, -1.443836171194816886 ) ) ;
#35815 = CARTESIAN_POINT ( 'NONE',  ( 7.401388779597747103, 20.28278527911644247, -1.500000000000002220 ) ) ;
#35816 = CARTESIAN_POINT ( 'NONE',  ( -113.5164963221879901, -24.35071581493543746, 9.817618358456018157 ) ) ;
#35817 = PLANE ( 'NONE',  #4714 ) ;
#35818 = EDGE_CURVE ( 'NONE', #40297, #39807, #5401, .T. ) ;
#35819 = CARTESIAN_POINT ( 'NONE',  ( -11.58057713800463162, -19.31455136971746001, 11.49999999999999645 ) ) ;
#35820 = VERTEX_POINT ( 'NONE', #42980 ) ;
#35821 = CARTESIAN_POINT ( 'NONE',  ( -69.64187497903644442, -25.24754278231193894, 5.000677553795553898 ) ) ;
#35822 = CARTESIAN_POINT ( 'NONE',  ( -10.95654650054425794, 19.06054500580150446, -1.500000000000002220 ) ) ;
#35823 = EDGE_CURVE ( 'NONE', #78258, #70560, #56874, .T. ) ;
#35824 = CARTESIAN_POINT ( 'NONE',  ( -44.66289782833593591, -23.48786465467240347, 11.44779295918255180 ) ) ;
#35825 = CARTESIAN_POINT ( 'NONE',  ( 8.971512145086499856, -1.028487854913500810, 6.500000000000000000 ) ) ;
#35826 = VERTEX_POINT ( 'NONE', #12012 ) ;
#35827 = DIRECTION ( 'NONE',  ( 1.000000000000000000, 0.000000000000000000, 0.000000000000000000 ) ) ;
#35828 = PLANE ( 'NONE',  #34892 ) ;
#35829 = ORIENTED_EDGE ( 'NONE', *, *, #94445, .F. ) ;
#35830 = DIRECTION ( 'NONE',  ( -3.773278334444166432E-23, 1.000000000000000000, 0.000000000000000000 ) ) ;
#35831 = VERTEX_POINT ( 'NONE', #44971 ) ;
#35832 = ORIENTED_EDGE ( 'NONE', *, *, #72938, .T. ) ;
#35833 = CARTESIAN_POINT ( 'NONE',  ( -65.52287095715007581, -24.51163499207173402, 0.6490370598554309201 ) ) ;
#35834 = LINE ( 'NONE', #4396, #82703 ) ;
#35836 = ADVANCED_FACE ( 'NONE', ( #67309 ), #35365, .F. ) ;
#35835 = CARTESIAN_POINT ( 'NONE',  ( -57.51496554766011826, -23.73766607897670866, -1.055555164236458454 ) ) ;
#35837 = CARTESIAN_POINT ( 'NONE',  ( -16.87313589883980214, -11.49665204554024989, -1.500000000000002220 ) ) ;
#35838 = ORIENTED_EDGE ( 'NONE', *, *, #78118, .T. ) ;
#35839 = CARTESIAN_POINT ( 'NONE',  ( -70.78845123859034061, -25.04713129051003051, 7.496186878019077682 ) ) ;
#35840 = CARTESIAN_POINT ( 'NONE',  ( -115.6228709571500417, -24.62285846362215835, 9.038163152653526211 ) ) ;
#35841 = CARTESIAN_POINT ( 'NONE',  ( -105.6235594576710781, -25.00158670708910691, 2.256160236439218369 ) ) ;
#35842 = CARTESIAN_POINT ( 'NONE',  ( -63.52287095715006160, -23.47596703998600631, 11.44779298504228926 ) ) ;
#35843 = ORIENTED_EDGE ( 'NONE', *, *, #15745, .F. ) ;
#35844 = CARTESIAN_POINT ( 'NONE',  ( 8.971512145086503409, -2.028487854913500144, 6.500000000000000000 ) ) ;
#35845 = CARTESIAN_POINT ( 'NONE',  ( 1.754398552524098376, 17.92127466780477718, -9.000000000000000000 ) ) ;
#35846 = EDGE_LOOP ( 'NONE', ( #74395, #46560, #42754, #41331 ) ) ;
#35847 = CARTESIAN_POINT ( 'NONE',  ( 5.792680761630559338, -19.98616098212858105, 11.49999999999998934 ) ) ;
#35848 = VECTOR ( 'NONE', #32409, 1000.000000000000114 ) ;
#35849 = ORIENTED_EDGE ( 'NONE', *, *, #54936, .T. ) ;
#35851 = ORIENTED_EDGE ( 'NONE', *, *, #75212, .T. ) ;
#35850 = CARTESIAN_POINT ( 'NONE',  ( -39.47626860353659595, -25.29241910976760366, 4.433561829988058811 ) ) ;
#35852 = CARTESIAN_POINT ( 'NONE',  ( 30.35461040182540415, -5.059010452157854942, 19.84760796525321425 ) ) ;
#35853 = CARTESIAN_POINT ( 'NONE',  ( -54.52287095715006870, -24.64898659630367916, 1.056161002820821038 ) ) ;
#35854 = VERTEX_POINT ( 'NONE', #60202 ) ;
#35855 = VERTEX_POINT ( 'NONE', #21605 ) ;
#35856 = CARTESIAN_POINT ( 'NONE',  ( -29.62287095715005236, -24.26166599405031121, 0.1849422882210577934 ) ) ;
#35857 = B_SPLINE_CURVE_WITH_KNOTS ( 'NONE', 3,
 ( #55743, #80557, #26774, #86669 ),
 .UNSPECIFIED., .F., .F.,
 ( 4, 4 ),
 ( 0.7993502183265108751, 0.8003509653672765678 ),
 .UNSPECIFIED. ) ;
#35858 = CARTESIAN_POINT ( 'NONE',  ( -64.52287095715010423, -24.66019654487200441, 8.947790411086119278 ) ) ;
#35859 = B_SPLINE_CURVE_WITH_KNOTS ( 'NONE', 3,
 ( #50804, #27467, #66049, #51801, #96466, #13214 ),
 .UNSPECIFIED., .F., .F.,
 ( 4, 2, 4 ),
 ( 0.000000000000000000, 0.001380764517853247733, 0.002761529035706495466 ),
 .UNSPECIFIED. ) ;
#35860 = DIRECTION ( 'NONE',  ( 0.000000000000000000, 0.000000000000000000, -1.000000000000000000 ) ) ;
#35861 = FACE_OUTER_BOUND ( 'NONE', #4623, .T. ) ;
#35863 = VERTEX_POINT ( 'NONE', #66327 ) ;
#35862 = CARTESIAN_POINT ( 'NONE',  ( 20.57837473233041692, -7.934362236255416256, 11.49999999999999645 ) ) ;
#35864 = CARTESIAN_POINT ( 'NONE',  ( -108.5876547150312206, -24.51314013834316086, 0.6176544820404235026 ) ) ;
#35865 = CARTESIAN_POINT ( 'NONE',  ( 8.141615846073909424, -21.09679883994429161, 11.49999999999998934 ) ) ;
#35867 = EDGE_LOOP ( 'NONE', ( #72903, #85806, #70410, #23434 ) ) ;
#35866 = CARTESIAN_POINT ( 'NONE',  ( -115.5535801380732295, -24.40133493613050675, 9.663955038902797057 ) ) ;
#35868 = EDGE_CURVE ( 'NONE', #68025, #57950, #52576, .T. ) ;
#35869 = AXIS2_PLACEMENT_3D ( 'NONE', #24404, #41149, #2092 ) ;
#35870 = ORIENTED_EDGE ( 'NONE', *, *, #43126, .F. ) ;
#35871 =( GEOMETRIC_REPRESENTATION_CONTEXT ( 3 ) GLOBAL_UNCERTAINTY_ASSIGNED_CONTEXT ( ( #76330 ) ) GLOBAL_UNIT_ASSIGNED_CONTEXT ( ( #59020, #12815, #71377 ) ) REPRESENTATION_CONTEXT ( 'NONE', 'WORKASPACE' ) );
#35872 = CARTESIAN_POINT ( 'NONE',  ( -10.40290173325841216, -6.376774720514426953, 27.45402280011861862 ) ) ;
#35873 = ADVANCED_FACE ( 'NONE', ( #82027 ), #49006, .T. ) ;
#35874 = ADVANCED_FACE ( 'NONE', ( #31224 ), #61696, .F. ) ;
#35875 = CARTESIAN_POINT ( 'NONE',  ( -57.59851968582830040, -23.96169478059713143, 10.65365249895718058 ) ) ;
#35876 = ORIENTED_EDGE ( 'NONE', *, *, #85630, .F. ) ;
#35877 = DIRECTION ( 'NONE',  ( 0.000000000000000000, 1.000000000000000000, 2.891205793294678326E-16 ) ) ;
#35878 = CARTESIAN_POINT ( 'NONE',  ( -7.755428854246955161, -20.87388092083558888, -1.500000000000002220 ) ) ;
#35879 = LINE ( 'NONE', #66849, #27390 ) ;
#35880 = ORIENTED_EDGE ( 'NONE', *, *, #40223, .F. ) ;
#35881 = CARTESIAN_POINT ( 'NONE',  ( -120.5228709571500616, -24.99132157543167310, 2.256160258750667502 ) ) ;
#35882 = CARTESIAN_POINT ( 'NONE',  ( -37.53291846491953976, -24.51314013834316796, 0.6176544820404176184 ) ) ;
#35883 = CARTESIAN_POINT ( 'NONE',  ( -108.6228709571500275, -24.51283580621365132, 0.6167428607019852516 ) ) ;
#35884 = CARTESIAN_POINT ( 'NONE',  ( -49.55620429048339304, -24.66019654487199020, 8.947790411086135265 ) ) ;
#35885 = CARTESIAN_POINT ( 'NONE',  ( -19.34354882100874562, 2.624169249526263403, -1.500000000000002220 ) ) ;
#35886 = CARTESIAN_POINT ( 'NONE',  ( -11.90495014755217618, 17.82271480561356469, 11.49999999999998934 ) ) ;
#35887 = B_SPLINE_CURVE_WITH_KNOTS ( 'NONE', 3,
 ( #60360, #35997, #97886, #28382, #13648, #67964 ),
 .UNSPECIFIED., .F., .F.,
 ( 4, 2, 4 ),
 ( 0.000000000000000000, 0.001380901958385389412, 0.002761803916770778824 ),
 .UNSPECIFIED. ) ;
#35888 = CARTESIAN_POINT ( 'NONE',  ( -65.05438548721848235, 5.356774720514425603, 27.45402280011862572 ) ) ;
#35889 = FACE_OUTER_BOUND ( 'NONE', #66691, .T. ) ;
#35890 = FACE_BOUND ( 'NONE', #32490, .T. ) ;
#35891 = CARTESIAN_POINT ( 'NONE',  ( -15.22011711465338912, -17.00649957279452451, -1.500000000000002220 ) ) ;
#35892 = EDGE_CURVE ( 'NONE', #66793, #18886, #45474, .T. ) ;
#35893 = EDGE_CURVE ( 'NONE', #65974, #91108, #7886, .T. ) ;
#35894 = CARTESIAN_POINT ( 'NONE',  ( -24.90875734969025501, -6.475225279485573360, 30.00402280011862288 ) ) ;
#35895 = DIRECTION ( 'NONE',  ( -1.000000000000000000, -0.000000000000000000, 0.000000000000000000 ) ) ;
#35896 = CARTESIAN_POINT ( 'NONE',  ( 10.22567584263966722, 17.17405255344276682, 11.49999999999999645 ) ) ;
#35897 = FACE_OUTER_BOUND ( 'NONE', #22465, .T. ) ;
#35898 = DIRECTION ( 'NONE',  ( -3.773278334444167608E-23, 1.000000000000000000, 0.000000000000000000 ) ) ;
#35899 = CARTESIAN_POINT ( 'NONE',  ( -48.50692445814570419, -23.96119346886881019, -0.6495511937831938143 ) ) ;
#35900 = ORIENTED_EDGE ( 'NONE', *, *, #74274, .F. ) ;
#35901 = CARTESIAN_POINT ( 'NONE',  ( -112.6228709571500559, -29.50250786944525672, 11.44777988621622988 ) ) ;
#35902 = CARTESIAN_POINT ( 'NONE',  ( 10.84340024150424497, -4.021317321268781164, -26.91457715659927175 ) ) ;
#35903 = CARTESIAN_POINT ( 'NONE',  ( -14.78470843206283902, -15.91074852019131924, 11.49999999999998934 ) ) ;
#35904 = EDGE_CURVE ( 'NONE', #87999, #50459, #76879, .T. ) ;
#35905 = FACE_OUTER_BOUND ( 'NONE', #7510, .T. ) ;
#35906 = CARTESIAN_POINT ( 'NONE',  ( -12.10551386448753064, 15.32171617432465816, -1.500000000000002220 ) ) ;
#35907 = EDGE_CURVE ( 'NONE', #14750, #96384, #81446, .T. ) ;
#35909 = B_SPLINE_CURVE_WITH_KNOTS ( 'NONE', 3,
 ( #90853, #12717, #97468, #5117 ),
 .UNSPECIFIED., .F., .F.,
 ( 4, 4 ),
 ( 0.000000000000000000, 9.999999999998206125E-05 ),
 .UNSPECIFIED. ) ;
#35908 = CARTESIAN_POINT ( 'NONE',  ( -20.27875734969026311, 6.143225279485574397, 24.00402280011862288 ) ) ;
#35910 = ORIENTED_EDGE ( 'NONE', *, *, #18035, .F. ) ;
#35911 = DATE_AND_TIME ( #12571, #16660 ) ;
#35912 = FACE_OUTER_BOUND ( 'NONE', #47913, .T. ) ;
#35913 = CARTESIAN_POINT ( 'NONE',  ( 10.78675619948152864, -17.38023510967517637, 11.49999999999999645 ) ) ;
#35914 = CARTESIAN_POINT ( 'NONE',  ( 8.255033872309153864, -6.475225279485571583, -27.10684724722607442 ) ) ;
#35915 = AXIS2_PLACEMENT_3D ( 'NONE', #21162, #37898, #98785 ) ;
#35916 = DIRECTION ( 'NONE',  ( -3.773278334453079030E-23, 0.9999999999976377785, 2.173523156925979128E-06 ) ) ;
#35917 = ORIENTED_EDGE ( 'NONE', *, *, #64959, .F. ) ;
#35918 = CARTESIAN_POINT ( 'NONE',  ( 3.509873074917118085, -5.965225279485572685, 29.15869884040363758 ) ) ;
#35919 = CARTESIAN_POINT ( 'NONE',  ( -106.6228709571500701, -24.50321055353805022, 9.387540953477515160 ) ) ;
#35920 = CARTESIAN_POINT ( 'NONE',  ( -78.62287095715007013, -23.72747288104442021, -1.053458166803662666 ) ) ;
#35921 = EDGE_CURVE ( 'NONE', #32470, #11757, #34177, .T. ) ;
#35922 = CARTESIAN_POINT ( 'NONE',  ( -41.62287095715006302, -29.50250243563736774, 8.947779886222148704 ) ) ;
#35923 = ORIENTED_EDGE ( 'NONE', *, *, #34671, .T. ) ;
#35924 = CARTESIAN_POINT ( 'NONE',  ( 10.54059822343757880, -6.376774720514426953, 22.82308057603841078 ) ) ;
#35925 = AXIS2_PLACEMENT_3D ( 'NONE', #42778, #11808, #87435 ) ;
#35926 = CARTESIAN_POINT ( 'NONE',  ( -10.52143791818333085, 20.43947972196396989, 11.49999999999999645 ) ) ;
#35927 = CARTESIAN_POINT ( 'NONE',  ( -16.34568771794417685, -15.85656593008108750, 11.49999999999998934 ) ) ;
#35928 = DIRECTION ( 'NONE',  ( 0.000000000000000000, -1.000000000000000000, 0.000000000000000000 ) ) ;
#35929 = B_SPLINE_CURVE_WITH_KNOTS ( 'NONE', 3,
 ( #80381, #752, #41322, #85990, #71271, #16464 ),
 .UNSPECIFIED., .F., .F.,
 ( 4, 2, 4 ),
 ( 0.000000000000000000, 0.001380901958385391580, 0.002761803916770783161 ),
 .UNSPECIFIED. ) ;
#35930 = CARTESIAN_POINT ( 'NONE',  ( -94.52287095715007581, -23.47593901973090524, -1.443836447538996648 ) ) ;
#35931 = CARTESIAN_POINT ( 'NONE',  ( -57.52287095715005449, -24.64898659630528854, 1.056161002820822592 ) ) ;
#35932 = APPROVAL_PERSON_ORGANIZATION ( #49398, #88468, #25542 ) ;
#35933 = CARTESIAN_POINT ( 'NONE',  ( -48.62287095715004881, -24.64898659630528144, 1.056161002820821038 ) ) ;
#35934 = CARTESIAN_POINT ( 'NONE',  ( -110.5546935055277800, -24.15503026093914229, -0.2815557561904443729 ) ) ;
#35935 = CARTESIAN_POINT ( 'NONE',  ( 15.24057855588860377, 15.72025634131890470, 11.49999999999998934 ) ) ;
#35936 = EDGE_CURVE ( 'NONE', #56269, #14843, #98308, .T. ) ;
#35937 = PLANE ( 'NONE',  #57553 ) ;
#35938 = EDGE_CURVE ( 'NONE', #85031, #59154, #30558, .T. ) ;
#35939 = CARTESIAN_POINT ( 'NONE',  ( -28.62287095715004526, -23.57175044478372783, -1.053577738039204847 ) ) ;
#35940 = CARTESIAN_POINT ( 'NONE',  ( -71.63959028355270675, -25.28439402384261925, 5.729062157909068809 ) ) ;
#35941 = DIRECTION ( 'NONE',  ( 0.9951627101165076983, -0.09824042138329622254, -8.881784197001249168E-15 ) ) ;
#35942 = EDGE_LOOP ( 'NONE', ( #76286, #7061, #30072, #22467, #21335, #27360 ) ) ;
#35943 = CARTESIAN_POINT ( 'NONE',  ( 16.50020720150075348, -12.08490501797973238, 11.49999999999998934 ) ) ;
#35944 = ORIENTED_EDGE ( 'NONE', *, *, #5960, .T. ) ;
#35945 = ORIENTED_EDGE ( 'NONE', *, *, #2256, .F. ) ;
#35946 = ORIENTED_EDGE ( 'NONE', *, *, #30938, .T. ) ;
#35947 = ORIENTED_EDGE ( 'NONE', *, *, #95872, .F. ) ;
#35948 = CARTESIAN_POINT ( 'NONE',  ( 21.10734164270438029, -9.282589649079691085, -1.500000000000002220 ) ) ;
#35950 = EDGE_CURVE ( 'NONE', #23355, #56728, #71421, .T. ) ;
#35949 = DIRECTION ( 'NONE',  ( -3.773278334453079618E-23, 0.9999999999976377785, 2.173523156925979975E-06 ) ) ;
#35951 = CARTESIAN_POINT ( 'NONE',  ( -19.21899500656021331, -6.280627263257740900, -1.500000000000002220 ) ) ;
#35952 = ORIENTED_EDGE ( 'NONE', *, *, #78761, .F. ) ;
#35953 = DIRECTION ( 'NONE',  ( -3.773278334453079618E-23, 0.9999999999976377785, 2.173523156925979975E-06 ) ) ;
#35954 = DIRECTION ( 'NONE',  ( -3.773278334453079030E-23, 0.9999999999976377785, 2.173523156925979128E-06 ) ) ;
#35955 = EDGE_CURVE ( 'NONE', #57247, #39449, #72800, .T. ) ;
#35956 = CARTESIAN_POINT ( 'NONE',  ( -95.62858950667747138, -24.63355581998386157, 0.9682620441943944334 ) ) ;
#35957 = CARTESIAN_POINT ( 'NONE',  ( -53.54175972517899140, -24.35071581493542681, 9.817618358456032368 ) ) ;
#35959 = VERTEX_POINT ( 'NONE', #26117 ) ;
#35958 = CARTESIAN_POINT ( 'NONE',  ( 13.34776491790984210, -16.67230741956907991, 11.49999999999999645 ) ) ;
#35960 = CARTESIAN_POINT ( 'NONE',  ( -128.6228709571500417, -24.64898659630529565, 1.056161002820834804 ) ) ;
#35961 = ORIENTED_EDGE ( 'NONE', *, *, #98794, .T. ) ;
#35962 = CARTESIAN_POINT ( 'NONE',  ( 5.670930919660429836, -21.52877996283707418, -1.500000000000002220 ) ) ;
#35963 = CARTESIAN_POINT ( 'NONE',  ( -1.398219401198234957, 20.63772364298462847, -1.500000000000002220 ) ) ;
#35964 = ORIENTED_EDGE ( 'NONE', *, *, #45668, .T. ) ;
#35965 = B_SPLINE_SURFACE_WITH_KNOTS ( 'NONE', 3, 3, ( 
 ( #51190, #59301, #90245, #20720 ),
 ( #75005, #5503, #67420, #28848 ),
 ( #18726, #21710, #29840, #99828 ),
 ( #99342, #84123, #100324, #45580 ),
 ( #15113, #83623, #6509, #22210 ),
 ( #52684, #29339, #44573, #61309 ),
 ( #77499, #14105, #60808, #6002 ) ),
 .UNSPECIFIED., .F., .F., .F.,
 ( 4, 3, 4 ),
 ( 4, 4 ),
 ( 0.7945040050992240310, 0.8970133687736498995, 0.9995227324480757680 ),
 ( 0.3095726639491566123, 0.3107283077887884049 ),
 .UNSPECIFIED. ) ;
#35966 = CARTESIAN_POINT ( 'NONE',  ( 15.29947330337542688, -3.316774720514426456, -27.16854002387010070 ) ) ;
#35967 = VERTEX_POINT ( 'NONE', #55582 ) ;
#35968 = CARTESIAN_POINT ( 'NONE',  ( -129.5228709571500190, -23.94994826722565406, -0.6494450866342675877 ) ) ;
#35969 = ORIENTED_EDGE ( 'NONE', *, *, #42597, .T. ) ;
#35970 = CARTESIAN_POINT ( 'NONE',  ( 11.42219733811748306, 17.55150860717643724, -1.500000000000002220 ) ) ;
#35971 = B_SPLINE_CURVE_WITH_KNOTS ( 'NONE', 3,
 ( #74945, #7943, #48389, #41791, #10821, #15551 ),
 .UNSPECIFIED., .F., .F.,
 ( 4, 2, 4 ),
 ( 1.570755371634033063E-05, 0.001396183895866087103, 0.002776660238015833844 ),
 .UNSPECIFIED. ) ;
#35972 = CARTESIAN_POINT ( 'NONE',  ( -1.606994170628035068, 21.82944698466814870, 11.49999999999999645 ) ) ;
#35973 = CARTESIAN_POINT ( 'NONE',  ( -37.50484986390183195, -23.96169478059712432, 10.65365249895718591 ) ) ;
#35974 = CARTESIAN_POINT ( 'NONE',  ( -15.53634343318938704, 16.32316209468629253, 11.49999999999998934 ) ) ;
#35975 = CARTESIAN_POINT ( 'NONE',  ( 20.89173079421859214, 1.537965369061287557, -1.500000000000002220 ) ) ;
#35976 = CARTESIAN_POINT ( 'NONE',  ( -80.55620429048342146, -24.99132157543166954, 2.256160258750668834 ) ) ;
#35977 = DIRECTION ( 'NONE',  ( 1.000000000000000000, 3.773278334444165844E-23, 8.201307836089272790E-29 ) ) ;
#35979 = EDGE_CURVE ( 'NONE', #76617, #87834, #85021, .T. ) ;
#35978 = CARTESIAN_POINT ( 'NONE',  ( -30.64427850938830389, -23.56000036390796737, -1.497999999999532594 ) ) ;
#35980 = EDGE_LOOP ( 'NONE', ( #92225, #15490, #55907, #94388, #69676 ) ) ;
#35981 = ORIENTED_EDGE ( 'NONE', *, *, #11572, .F. ) ;
#35982 = ORIENTED_EDGE ( 'NONE', *, *, #21019, .T. ) ;
#35983 = VECTOR ( 'NONE', #3117, 1000.000000000000000 ) ;
#35984 = CARTESIAN_POINT ( 'NONE',  ( -128.6228709571500417, -23.96177878511308634, 10.65340807706329151 ) ) ;
#35985 = CARTESIAN_POINT ( 'NONE',  ( 14.05358622956002357, 16.19628355576825385, -1.500000000000002220 ) ) ;
#35986 = CARTESIAN_POINT ( 'NONE',  ( -127.6228709571500559, -29.50248528299804818, 1.056150453629047137 ) ) ;
#35987 = EDGE_LOOP ( 'NONE', ( #3770, #56696, #56709, #52313 ) ) ;
#35988 = CARTESIAN_POINT ( 'NONE',  ( -18.71117167593497399, 9.704403692310313190, 11.49999999999998934 ) ) ;
#35989 = CARTESIAN_POINT ( 'NONE',  ( -60.52287095715007581, -25.00182538069855198, 7.747789668514453609 ) ) ;
#35990 = CARTESIAN_POINT ( 'NONE',  ( -52.62287095715005592, -23.48783264082478794, -1.443836473390070596 ) ) ;
#35991 = CARTESIAN_POINT ( 'NONE',  ( -51.62287095715005592, -29.50250243563736774, 8.947779886222146928 ) ) ;
#35992 = CARTESIAN_POINT ( 'NONE',  ( 6.620851319379956301, -6.475225279485576024, -27.30756699305372592 ) ) ;
#35993 = DIRECTION ( 'NONE',  ( 0.000000000000000000, 0.9999999999976377785, 2.173523156925979128E-06 ) ) ;
#35994 = CARTESIAN_POINT ( 'NONE',  ( -21.12782282263547984, 6.412464199276892707, -1.500000000000002220 ) ) ;
#35995 = FACE_OUTER_BOUND ( 'NONE', #6623, .T. ) ;
#35996 = CARTESIAN_POINT ( 'NONE',  ( -109.0052451887007550, -25.29780460623759808, 4.561057382153821393 ) ) ;
#35997 = CARTESIAN_POINT ( 'NONE',  ( -99.52287095715003318, -24.50321055353804667, 9.387540953477522265 ) ) ;
#35998 = B_SPLINE_CURVE_WITH_KNOTS ( 'NONE', 3,
 ( #33547, #11210, #64532, #95444, #10714, #41677 ),
 .UNSPECIFIED., .F., .F.,
 ( 4, 2, 4 ),
 ( 1.570755371633718645E-05, 0.001396183895866087103, 0.002776660238015837313 ),
 .UNSPECIFIED. ) ;
#35999 = DIRECTION ( 'NONE',  ( 4.089440751051245812E-15, 1.000000000000000000, -1.042451643221144600E-15 ) ) ;
#36000 = AXIS2_PLACEMENT_3D ( 'NONE', #93186, #69864, #37912 ) ;
#36001 = CARTESIAN_POINT ( 'NONE',  ( -14.39514105012195344, 13.04300321504834947, 11.49999999999998934 ) ) ;
#36002 = CC_DESIGN_APPROVAL ( #39556, ( #57555 ) ) ;
#36003 = CARTESIAN_POINT ( 'NONE',  ( 21.01207135711032237, 3.775690236426352264, 11.49999999999998934 ) ) ;
#36004 = CARTESIAN_POINT ( 'NONE',  ( -123.5228709571500616, -23.47596703998600631, 11.44779298504227860 ) ) ;
#36005 = DIRECTION ( 'NONE',  ( -0.000000000000000000, 1.000000000000000000, -0.000000000000000000 ) ) ;
#36006 = CARTESIAN_POINT ( 'NONE',  ( -64.53959531558551532, -24.51419770103158058, 9.386484678747169852 ) ) ;
#36007 = CYLINDRICAL_SURFACE ( 'NONE', #28193, 3.349999999999998757 ) ;
#36008 = CARTESIAN_POINT ( 'NONE',  ( 22.61563695565308407, -1.323143620866313208, -1.500000000000002220 ) ) ;
#36009 = EDGE_CURVE ( 'NONE', #85275, #20569, #40636, .T. ) ;
#36010 = ORIENTED_EDGE ( 'NONE', *, *, #96968, .T. ) ;
#36011 = CARTESIAN_POINT ( 'NONE',  ( -87.52287095715009002, -23.96177878511308990, 10.65340807706329862 ) ) ;
#36012 = CARTESIAN_POINT ( 'NONE',  ( -79.63744315085436654, -23.96119346886880308, -0.6495511937832122440 ) ) ;
#36013 = CARTESIAN_POINT ( 'NONE',  ( -6.535591236171724105, 18.61618873491671877, 11.49999999999999645 ) ) ;
#36014 = CARTESIAN_POINT ( 'NONE',  ( -10.34999999999997833, 22.00000000000000000, 2.100000000000000089 ) ) ;
#36015 = CYLINDRICAL_SURFACE ( 'NONE', #17200, 1.325999999999969647 ) ;
#36016 = VERTEX_POINT ( 'NONE', #18997 ) ;
#36017 = CARTESIAN_POINT ( 'NONE',  ( -53.62287095715003460, -23.72773821059535493, 11.05748984161097503 ) ) ;
#36018 = CARTESIAN_POINT ( 'NONE',  ( -29.22648335530837471, -24.60094061072802063, 2.413927280369137396 ) ) ;
#36020 = EDGE_CURVE ( 'NONE', #3816, #59423, #56588, .T. ) ;
#36019 = CARTESIAN_POINT ( 'NONE',  ( -75.52287095715004739, -23.85229601348995487, 10.88205029486208986 ) ) ;
#36021 = CARTESIAN_POINT ( 'NONE',  ( 0.6597851148675514255, -21.60297929554585394, -1.500000000000002220 ) ) ;
#36022 = EDGE_CURVE ( 'NONE', #50770, #57758, #87523, .T. ) ;
#36023 = CARTESIAN_POINT ( 'NONE',  ( -26.71664755962209981, -24.80833360015218148, 7.192517110868322128 ) ) ;
#36024 = CARTESIAN_POINT ( 'NONE',  ( 12.39309347844599252, 14.90900669795185252, -1.500000000000002220 ) ) ;
#36025 = ADVANCED_FACE ( 'NONE', ( #18500 ), #21604, .T. ) ;
#36026 = CARTESIAN_POINT ( 'NONE',  ( -50.62287095715005592, -23.47593901973091235, -1.443836447539009749 ) ) ;
#36027 = B_SPLINE_CURVE_WITH_KNOTS ( 'NONE', 3,
 ( #13933, #98667, #60139, #12933 ),
 .UNSPECIFIED., .F., .F.,
 ( 4, 4 ),
 ( 6.938893903907228378E-18, 9.999999999999591193E-05 ),
 .UNSPECIFIED. ) ;
#36028 = CARTESIAN_POINT ( 'NONE',  ( -66.52287095715006160, -23.48786465467241769, 11.44779295918254647 ) ) ;
#36029 = CARTESIAN_POINT ( 'NONE',  ( 19.75791096855702733, 1.210928449428283038, 11.49999999999998934 ) ) ;
#36030 = VERTEX_POINT ( 'NONE', #49474 ) ;
#36031 = EDGE_CURVE ( 'NONE', #13191, #64103, #57205, .T. ) ;
#36032 = CARTESIAN_POINT ( 'NONE',  ( -14.64122064730360862, 14.02963135428074004, 11.49999999999999645 ) ) ;
#36033 = CARTESIAN_POINT ( 'NONE',  ( -99.16166289166532977, -25.31166538673566180, 5.311370725864150266 ) ) ;
#36035 = CIRCLE ( 'NONE', #74915, 25.90800000000000125 ) ;
#36034 = CARTESIAN_POINT ( 'NONE',  ( 0.1553305729023591875, 1.423459158329793306, 1.743234701965566823E-16 ) ) ;
#36036 = ORIENTED_EDGE ( 'NONE', *, *, #17837, .F. ) ;
#36037 = DIRECTION ( 'NONE',  ( 0.09824042138329590335, -0.9951627101165079203, -3.519298150595267883E-15 ) ) ;
#36038 = CARTESIAN_POINT ( 'NONE',  ( 31.62416306531753918, 4.295372699094516022, 26.87458401151571508 ) ) ;
#36039 = CARTESIAN_POINT ( 'NONE',  ( -44.62287095715004881, -23.48783264082478084, -1.443836473390072150 ) ) ;
#36040 = B_SPLINE_CURVE_WITH_KNOTS ( 'NONE', 3,
 ( #32549, #63521, #94952, #101, #25438, #94449 ),
 .UNSPECIFIED., .F., .F.,
 ( 4, 2, 4 ),
 ( 1.570887131794333942E-05, 0.001396322306279760422, 0.002776935741241577573 ),
 .UNSPECIFIED. ) ;
#36041 = CARTESIAN_POINT ( 'NONE',  ( -92.55620429048339304, -24.66019654487199730, 8.947790411086126383 ) ) ;
#36042 = CARTESIAN_POINT ( 'NONE',  ( -85.52287095715006160, -29.50247984919015209, -1.443849546365051806 ) ) ;
#36043 = CARTESIAN_POINT ( 'NONE',  ( 18.34943919012036773, 8.063251210807163005, -1.500000000000002220 ) ) ;
#36044 = EDGE_CURVE ( 'NONE', #55518, #9188, #56080, .T. ) ;
#36045 = LINE ( 'NONE', #3120, #85562 ) ;
#36046 = ORIENTED_EDGE ( 'NONE', *, *, #63449, .F. ) ;
#36047 = EDGE_CURVE ( 'NONE', #100181, #27742, #23178, .T. ) ;
#36048 = CARTESIAN_POINT ( 'NONE',  ( -50.05252738782304789, -25.31297205221429891, 4.679464295789098394 ) ) ;
#36049 = VECTOR ( 'NONE', #10441, 1000.000000000000114 ) ;
#36050 = DIRECTION ( 'NONE',  ( -3.773278334453079618E-23, 0.9999999999976377785, 2.173523156925979975E-06 ) ) ;
#36051 = LINE ( 'NONE', #29428, #15995 ) ;
#36052 = CARTESIAN_POINT ( 'NONE',  ( 30.55456828421201720, -1.252966014080255430, 24.28055799599966846 ) ) ;
#36053 = EDGE_CURVE ( 'NONE', #14276, #52727, #3307, .T. ) ;
#36054 = FACE_OUTER_BOUND ( 'NONE', #36512, .T. ) ;
#36055 = CARTESIAN_POINT ( 'NONE',  ( -19.78178409256797465, 10.57734301857266246, 11.49999999999999645 ) ) ;
#36056 = DIRECTION ( 'NONE',  ( 0.000000000000000000, -1.000000000000000000, 0.000000000000000000 ) ) ;
#36057 = ORIENTED_EDGE ( 'NONE', *, *, #12569, .T. ) ;
#36058 = CARTESIAN_POINT ( 'NONE',  ( -2.495337616714382367, -20.20711602426958819, 11.49999999999998934 ) ) ;
#36059 = ORIENTED_EDGE ( 'NONE', *, *, #48010, .F. ) ;
#36060 = CARTESIAN_POINT ( 'NONE',  ( 22.95104020007722667, -0.4190376320207603866, -1.500000000000002220 ) ) ;
#36061 = EDGE_CURVE ( 'NONE', #30291, #30754, #89881, .T. ) ;
#36062 = DIRECTION ( 'NONE',  ( 0.000000000000000000, 0.000000000000000000, -1.000000000000000000 ) ) ;
#36063 = ORIENTED_EDGE ( 'NONE', *, *, #58868, .T. ) ;
#36064 = CARTESIAN_POINT ( 'NONE',  ( -109.5228709571501327, -23.96127896941632685, -0.6493128931037961404 ) ) ;
#36065 = ADVANCED_FACE ( 'NONE', ( #43353 ), #73787, .F. ) ;
#36066 = CARTESIAN_POINT ( 'NONE',  ( -77.55422458372758854, -23.96169478059713498, 10.65365249895717703 ) ) ;
#36067 = VECTOR ( 'NONE', #52606, 1000.000000000000114 ) ;
#36068 = ADVANCED_FACE ( 'NONE', ( #81408 ), #83173, .T. ) ;
#36069 = CARTESIAN_POINT ( 'NONE',  ( -117.5895376238167245, -23.48786465467241769, 11.44779295918253759 ) ) ;
#36071 = ORIENTED_EDGE ( 'NONE', *, *, #42483, .F. ) ;
#36070 = CARTESIAN_POINT ( 'NONE',  ( -21.08860491664495029, 2.407354197416772035, 11.49999999999999645 ) ) ;
#36072 = LOCAL_TIME ( 0, 54, 15.00000000000000000, #47772 ) ;
#36073 = ORIENTED_EDGE ( 'NONE', *, *, #52474, .T. ) ;
#36074 = CARTESIAN_POINT ( 'NONE',  ( 4.260453091581613450, -21.75001586557718980, 11.49999999999998934 ) ) ;
#36075 = B_SPLINE_CURVE_WITH_KNOTS ( 'NONE', 3,
 ( #24384, #38105, #22860, #39609 ),
 .UNSPECIFIED., .F., .F.,
 ( 4, 4 ),
 ( 0.07984293836553946200, 0.08884936963765502349 ),
 .UNSPECIFIED. ) ;
#36076 = CARTESIAN_POINT ( 'NONE',  ( -6.273408026305254737, 19.60348359158234288, -1.500000000000002220 ) ) ;
#36077 = VERTEX_POINT ( 'NONE', #75276 ) ;
#36079 = ORIENTED_EDGE ( 'NONE', *, *, #2578, .F. ) ;
#36078 = VECTOR ( 'NONE', #44645, 1000.000000000000114 ) ;
#36080 = CARTESIAN_POINT ( 'NONE',  ( 14.52511747680497933, 5.965225279485572685, -27.86035006098926559 ) ) ;
#36081 = CARTESIAN_POINT ( 'NONE',  ( -126.6228709571500843, -24.51387760970726859, 9.387446482453416507 ) ) ;
#36082 = EDGE_LOOP ( 'NONE', ( #57900, #61335, #71592, #58692 ) ) ;
#36083 = EDGE_LOOP ( 'NONE', ( #52263, #37668, #73649, #14013 ) ) ;
#36084 = ORIENTED_EDGE ( 'NONE', *, *, #53589, .T. ) ;
#36085 = VECTOR ( 'NONE', #39854, 1000.000000000000114 ) ;
#36086 = FACE_OUTER_BOUND ( 'NONE', #73371, .T. ) ;
#36087 = CARTESIAN_POINT ( 'NONE',  ( -28.66135699505452550, -23.58527356016855236, 11.05961558438220749 ) ) ;
#36088 = CARTESIAN_POINT ( 'NONE',  ( -130.5728709571500588, -23.56000036390796737, 11.50200000000000244 ) ) ;
#36089 = CARTESIAN_POINT ( 'NONE',  ( 1.902724757927627408, 20.64897553884969028, -1.500000000000002220 ) ) ;
#36090 = CARTESIAN_POINT ( 'NONE',  ( -13.51661872714272405, -17.00040112538478709, 11.49999999999999645 ) ) ;
#36091 = ORIENTED_EDGE ( 'NONE', *, *, #40556, .T. ) ;
#36092 = CARTESIAN_POINT ( 'NONE',  ( -40.91098280806539833, -25.27806118004114211, 4.981854051466827471 ) ) ;
#36093 = CARTESIAN_POINT ( 'NONE',  ( -77.55620429048339304, -23.48786465467241058, 11.44779295918254469 ) ) ;
#36094 = CARTESIAN_POINT ( 'NONE',  ( -115.5902995085408094, -24.40034930558991277, 0.3402023900116066257 ) ) ;
#36095 = CARTESIAN_POINT ( 'NONE',  ( -0.1411031551986380028, 22.44022050402121948, -1.500000000000002220 ) ) ;
#36096 = CARTESIAN_POINT ( 'NONE',  ( -20.27875734969026311, -6.376774720514428729, 21.00402280011862644 ) ) ;
#36097 = CARTESIAN_POINT ( 'NONE',  ( -124.5228709571500900, -24.35013146730205236, 9.818937971375092388 ) ) ;
#36098 = VERTEX_POINT ( 'NONE', #5769 ) ;
#36099 = CARTESIAN_POINT ( 'NONE',  ( -71.33442243081988465, -25.31573830894388166, 5.086045725258812489 ) ) ;
#36100 = B_SPLINE_SURFACE_WITH_KNOTS ( 'NONE', 3, 1, ( 
 ( #36474, #66946 ),
 ( #90763, #27373 ),
 ( #28360, #27865 ),
 ( #13623, #59321 ),
 ( #20740, #65961 ),
 ( #51708, #81157 ),
 ( #96881, #88781 ),
 ( #13126, #82646 ),
 ( #75022, #65463 ),
 ( #75523, #42612 ),
 ( #96380, #89269 ),
 ( #50710, #5521 ),
 ( #67437, #19247 ),
 ( #74047, #28867 ),
 ( #50215, #12131 ),
 ( #4545, #58823 ),
 ( #59829, #21238 ),
 ( #19738, #44595 ),
 ( #73548, #76024 ) ),
 .UNSPECIFIED., .F., .F., .F.,
 ( 4, 1, 1, 1, 1, 1, 1, 1, 1, 1, 1, 1, 1, 1, 1, 1, 4 ),
 ( 2, 2 ),
 ( 0.000000000000000000, 0.06891237672743111276, 0.1352246433344312937, 0.2001606018079680194, 0.2639831308323357106, 0.3270287715257772510, 0.3902418945738325151, 0.4541682297891322939, 0.5193355915291701930, 0.5832703360758352273, 0.6452842511902443512, 0.7050706230450887180, 0.7637435797381000313, 0.8217746784923816161, 0.8800061561487860784, 0.9388620850843768517, 1.000000000000000000 ),
 ( 0.000000000000000000, 1.000000000000000000 ),
 .UNSPECIFIED. ) ;
#36101 = ORIENTED_EDGE ( 'NONE', *, *, #24053, .T. ) ;
#36102 = ORIENTED_EDGE ( 'NONE', *, *, #34081, .T. ) ;
#36103 = CARTESIAN_POINT ( 'NONE',  ( -46.51385822909820433, -23.73791477778911840, 11.05961554403171299 ) ) ;
#36104 = ORIENTED_EDGE ( 'NONE', *, *, #8293, .F. ) ;
#36105 = VECTOR ( 'NONE', #76663, 1000.000000000000000 ) ;
#36106 = CARTESIAN_POINT ( 'NONE',  ( 14.87313431965483801, 15.23822737908125902, -1.500000000000002220 ) ) ;
#36107 = VERTEX_POINT ( 'NONE', #76267 ) ;
#36108 = CARTESIAN_POINT ( 'NONE',  ( -41.52287095715006870, -24.64965694238406613, 8.947790433994205372 ) ) ;
#36109 = PRODUCT_DEFINITION_SHAPE ( 'NONE', 'NONE',  #57555 ) ;
#36110 = CARTESIAN_POINT ( 'NONE',  ( -5.042499505632127565, 21.24692939306837758, -1.500000000000002220 ) ) ;
#36111 = CARTESIAN_POINT ( 'NONE',  ( -101.6228709571500559, -29.50250243563736774, 8.947779886222138046 ) ) ;
#36112 = CARTESIAN_POINT ( 'NONE',  ( 22.70222466501550329, 0.2752559529566028229, -1.500000000000002220 ) ) ;
#36113 = CARTESIAN_POINT ( 'NONE',  ( -40.49257998994310270, -25.28892422309372634, 3.294941674263239140 ) ) ;
#36114 = CARTESIAN_POINT ( 'NONE',  ( 22.02124265030973760, -4.776774720514394446, 16.20402280011862217 ) ) ;
#36115 = CARTESIAN_POINT ( 'NONE',  ( 20.57779966680088890, -7.652443150423321683, -1.500000000000002220 ) ) ;
#36116 = CARTESIAN_POINT ( 'NONE',  ( -87.62875567979766345, -24.34968618360935011, 0.1864209137778971292 ) ) ;
#36117 = EDGE_LOOP ( 'NONE', ( #55579, #39171, #19839, #18973 ) ) ;
#36118 = CARTESIAN_POINT ( 'NONE',  ( -40.17570312657086617, -25.29422630904218039, 5.527950596489476176 ) ) ;
#36119 = CARTESIAN_POINT ( 'NONE',  ( 8.000000000000003553, -5.876774720514426953, 17.50000000000000000 ) ) ;
#36120 = VECTOR ( 'NONE', #79518, 1000.000000000000000 ) ;
#36121 = B_SPLINE_CURVE_WITH_KNOTS ( 'NONE', 3,
 ( #63158, #52169, #91219, #94086, #29323, #21695, #72771 ),
 .UNSPECIFIED., .F., .F.,
 ( 4, 1, 1, 1, 4 ),
 ( 0.000000000000000000, 0.2835948081386949760, 0.5433948405759660982, 0.7806456291745647036, 1.000000000000000000 ),
 .UNSPECIFIED. ) ;
#36122 = ORIENTED_EDGE ( 'NONE', *, *, #29854, .T. ) ;
#36123 = CARTESIAN_POINT ( 'NONE',  ( -84.55445823045992881, -23.96169478059713498, 10.65365249895717881 ) ) ;
#36124 = B_SPLINE_CURVE_WITH_KNOTS ( 'NONE', 3,
 ( #44950, #84490, #78859, #33201 ),
 .UNSPECIFIED., .F., .F.,
 ( 4, 4 ),
 ( 0.3707647540354188642, 0.3797711853075343980 ),
 .UNSPECIFIED. ) ;
#36125 = VECTOR ( 'NONE', #92426, 1000.000000000000227 ) ;
#36126 = DIRECTION ( 'NONE',  ( -3.773278334453079618E-23, 0.9999999999976377785, 2.173523156925978705E-06 ) ) ;
#36127 = CARTESIAN_POINT ( 'NONE',  ( -20.45437310074456860, -23.26047912157225994, -0.4716817114508955466 ) ) ;
#36128 = CARTESIAN_POINT ( 'NONE',  ( -16.85803360905838488, 12.98640638483674259, -1.500000000000002220 ) ) ;
#36129 = CARTESIAN_POINT ( 'NONE',  ( -98.58670432545206097, -24.51419770103156992, 9.386484678747175181 ) ) ;
#36130 = DIRECTION ( 'NONE',  ( 0.000000000000000000, -1.000000000000000000, 0.000000000000000000 ) ) ;
#36131 = CARTESIAN_POINT ( 'NONE',  ( -70.32380231474228083, -29.50249842297920466, 7.101626040072651413 ) ) ;
#36132 = CARTESIAN_POINT ( 'NONE',  ( -85.62287095715007013, -23.84081130438200802, 10.88220057463249546 ) ) ;
#36133 = CARTESIAN_POINT ( 'NONE',  ( -90.58953762381672448, -24.99132157543084531, 2.256160258750496972 ) ) ;
#36134 = EDGE_LOOP ( 'NONE', ( #26857, #12355, #58587, #60188 ) ) ;
#36135 = ADVANCED_FACE ( 'NONE', ( #70167 ), #14869, .F. ) ;
#36136 = CARTESIAN_POINT ( 'NONE',  ( -1.979602623192304955, -19.45764201480039901, 11.49999999999999645 ) ) ;
#36137 = CARTESIAN_POINT ( 'NONE',  ( -99.12672508963875373, -25.28202003831819056, 4.094530911986962174 ) ) ;
#36138 = EDGE_CURVE ( 'NONE', #44563, #17901, #9834, .T. ) ;
#36139 = CARTESIAN_POINT ( 'NONE',  ( 19.24418710706453339, -0.5000000000000000000, 2.346898003627108320 ) ) ;
#36140 = ORIENTED_EDGE ( 'NONE', *, *, #49972, .F. ) ;
#36141 = ADVANCED_FACE ( 'NONE', ( #62566 ), #61572, .F. ) ;
#36142 = CARTESIAN_POINT ( 'NONE',  ( 4.400426145423703694, -5.876774720514425177, 21.64763382324305852 ) ) ;
#36143 = CARTESIAN_POINT ( 'NONE',  ( -99.33274021282838362, -25.25095929706067821, 5.901068790733613234 ) ) ;
#36144 = EDGE_CURVE ( 'NONE', #803, #77182, #42637, .T. ) ;
#36145 = CARTESIAN_POINT ( 'NONE',  ( -25.67705512370713095, -24.85598980928401147, 6.414578969243027728 ) ) ;
#36146 = EDGE_CURVE ( 'NONE', #32109, #79759, #99550, .T. ) ;
#36147 = CIRCLE ( 'NONE', #83139, 19.00000000000000000 ) ;
#36148 = CARTESIAN_POINT ( 'NONE',  ( -45.62287095715006302, -24.82558206586143612, 1.605769216559445045 ) ) ;
#36149 = CARTESIAN_POINT ( 'NONE',  ( -10.80270875523330965, -16.48872379891551532, -1.500000000000002220 ) ) ;
#36151 = ORIENTED_EDGE ( 'NONE', *, *, #2762, .T. ) ;
#36150 = CC_DESIGN_APPROVAL ( #42550, ( #78282 ) ) ;
#36152 = CARTESIAN_POINT ( 'NONE',  ( -108.5228709571500616, -23.47596703998600631, 11.44779298504228038 ) ) ;
#36153 = CARTESIAN_POINT ( 'NONE',  ( 3.004381791450704942, -5.876774720514420736, 20.78526834885430219 ) ) ;
#36154 = VECTOR ( 'NONE', #53510, 999.9999999999998863 ) ;
#36155 = DATE_AND_TIME ( #13794, #68459 ) ;
#36156 = ORIENTED_EDGE ( 'NONE', *, *, #73631, .T. ) ;
#36157 = CARTESIAN_POINT ( 'NONE',  ( -54.52287095715006870, -24.64965694238575011, 8.947790433994203596 ) ) ;
#36158 = CARTESIAN_POINT ( 'NONE',  ( -1.359251851468251449, -6.376774720514420736, 20.71116975788854120 ) ) ;
#36159 = CARTESIAN_POINT ( 'NONE',  ( -47.57719180744601317, -24.65952944569304606, 1.056160979905696129 ) ) ;
#36160 = DIRECTION ( 'NONE',  ( 0.06283980576413539243, 0.000000000000000000, 0.9980236263794188822 ) ) ;
#36161 = CARTESIAN_POINT ( 'NONE',  ( -7.282824509310913186, -6.376774720514415407, 19.84584863393302356 ) ) ;
#36162 = DIRECTION ( 'NONE',  ( 0.000000000000000000, -0.9999999999976377785, -2.173523156925979975E-06 ) ) ;
#36163 = AXIS2_PLACEMENT_3D ( 'NONE', #15616, #80025, #41469 ) ;
#36164 = CARTESIAN_POINT ( 'NONE',  ( -91.52287095715006160, -24.64965694238575011, 8.947790433994196491 ) ) ;
#36165 = CARTESIAN_POINT ( 'NONE',  ( -15.85412420263326538, -12.13584807887712458, -1.500000000000002220 ) ) ;
#36166 = ADVANCED_FACE ( 'NONE', ( #78259 ), #95169, .T. ) ;
#36167 = CARTESIAN_POINT ( 'NONE',  ( 30.93860345374796594, 0.6647747205144264315, 19.84760796525321780 ) ) ;
#36168 = CARTESIAN_POINT ( 'NONE',  ( -0.02330722796118872564, -22.74826961827042382, 7.709244911848460724 ) ) ;
#36169 = ORIENTED_EDGE ( 'NONE', *, *, #17709, .T. ) ;
#36170 = LINE ( 'NONE', #67626, #34571 ) ;
#36171 = CARTESIAN_POINT ( 'NONE',  ( 8.971512145086524725, -7.528487854913503696, -4.499999999999999112 ) ) ;
#36172 = EDGE_CURVE ( 'NONE', #70078, #41837, #77755, .T. ) ;
#36173 = CARTESIAN_POINT ( 'NONE',  ( -107.2228709571500929, -23.47593901973090169, -1.443836447538996648 ) ) ;
#36174 = CARTESIAN_POINT ( 'NONE',  ( -80.55868461798210944, -23.85049219812685806, 10.88485053497527311 ) ) ;
#36175 = CARTESIAN_POINT ( 'NONE',  ( 30.93860345374796594, -5.965225279485573573, 28.83647319851474933 ) ) ;
#36176 = CARTESIAN_POINT ( 'NONE',  ( -39.64841240158730074, -23.96119346886879597, -0.6495511937832143534 ) ) ;
#36177 = CARTESIAN_POINT ( 'NONE',  ( -26.09950011358278843, -24.96552080349164981, 4.651270459924270462 ) ) ;
#36178 = CARTESIAN_POINT ( 'NONE',  ( -1.743696941008423984, -6.376774720514413630, 19.59984006504825160 ) ) ;
#36179 = ORIENTED_EDGE ( 'NONE', *, *, #14227, .F. ) ;
#36180 = B_SPLINE_SURFACE_WITH_KNOTS ( 'NONE', 3, 3, ( 
 ( #68591, #85815, #99515, #60985 ),
 ( #84299, #14786, #45752, #100007 ),
 ( #56389, #72603, #87821, #18308 ),
 ( #64009, #41154, #63503, #48264 ),
 ( #9184, #24906, #18797, #86312 ),
 ( #33530, #41656, #25915, #78678 ),
 ( #17299, #40145, #87311, #2593 ) ),
 .UNSPECIFIED., .F., .F., .F.,
 ( 4, 3, 4 ),
 ( 4, 4 ),
 ( 0.7945040050992233649, 0.8970133687736493444, 0.9995227324480753239 ),
 ( 0.05950911933808800819, 0.06054931725151718042 ),
 .UNSPECIFIED. ) ;
#36181 = CARTESIAN_POINT ( 'NONE',  ( -37.62287095715005592, -24.64965695001467694, 8.947790433994187609 ) ) ;
#36182 = CARTESIAN_POINT ( 'NONE',  ( 5.994920710892026605, -5.876774720514428729, 21.76186867112717138 ) ) ;
#36183 = ORIENTED_EDGE ( 'NONE', *, *, #33054, .F. ) ;
#36184 = CARTESIAN_POINT ( 'NONE',  ( -6.993686169601437186, 18.98418669460116348, -1.500000000000002220 ) ) ;
#36185 = CARTESIAN_POINT ( 'NONE',  ( -43.52287095715004739, -23.48783264083374078, -1.443836473376152840 ) ) ;
#36186 = CARTESIAN_POINT ( 'NONE',  ( 12.16765770914787304, 6.475225279485573360, -27.57618308014988173 ) ) ;
#36187 = CIRCLE ( 'NONE', #62127, 0.3000000000000016542 ) ;
#36188 = CARTESIAN_POINT ( 'NONE',  ( -82.58953762381673869, -24.66019654487199730, 8.947790411086119278 ) ) ;
#36190 = ORIENTED_EDGE ( 'NONE', *, *, #97028, .T. ) ;
#36189 = ADVANCED_FACE ( 'NONE', ( #23467 ), #85382, .T. ) ;
#36191 = CARTESIAN_POINT ( 'NONE',  ( -24.90875734969025501, 3.316774720514426456, 30.51402280011862089 ) ) ;
#36192 = CARTESIAN_POINT ( 'NONE',  ( -1.967852706420949005, -6.376774720514408301, 19.18381548539530357 ) ) ;
#36193 = CARTESIAN_POINT ( 'NONE',  ( 11.39338536883839659, -16.50304575528446804, -1.500000000000002220 ) ) ;
#36194 = AXIS2_PLACEMENT_3D ( 'NONE', #84950, #98678, #6336 ) ;
#36195 = CARTESIAN_POINT ( 'NONE',  ( 21.00884048613226440, 1.293913838035418040, 11.49999999999999645 ) ) ;
#36196 = DIRECTION ( 'NONE',  ( 0.000000000000000000, 0.000000000000000000, -1.000000000000000000 ) ) ;
#36197 = CARTESIAN_POINT ( 'NONE',  ( -70.58187708969072105, -24.83644354573578994, 8.397322867130100121 ) ) ;
#36198 = CARTESIAN_POINT ( 'NONE',  ( -7.692412698405892257, 20.70400481474656118, -1.500000000000002220 ) ) ;
#36199 = EDGE_CURVE ( 'NONE', #39807, #19418, #20855, .T. ) ;
#36200 = DIRECTION ( 'NONE',  ( 0.9951627101165076983, 0.000000000000000000, 0.09824042138329622254 ) ) ;
#36201 = CARTESIAN_POINT ( 'NONE',  ( -76.52287095715007581, -23.47593901973090169, -1.443836447538996648 ) ) ;
#36202 = CARTESIAN_POINT ( 'NONE',  ( -64.55620429048339304, -23.47596703998600276, 11.44779298504227505 ) ) ;
#36203 = ORIENTED_EDGE ( 'NONE', *, *, #69702, .F. ) ;
#36204 = CARTESIAN_POINT ( 'NONE',  ( 33.13288845015618023, 5.965225279485572685, -0.1650522222209214185 ) ) ;
#36205 = CARTESIAN_POINT ( 'NONE',  ( -31.53142997842084938, -24.51314013834316086, 0.6176544820404139546 ) ) ;
#36206 = VERTEX_POINT ( 'NONE', #17380 ) ;
#36207 = ORIENTED_EDGE ( 'NONE', *, *, #54588, .T. ) ;
#36208 = DIRECTION ( 'NONE',  ( -0.000000000000000000, -1.000000000000000000, -0.000000000000000000 ) ) ;
#36209 = DIRECTION ( 'NONE',  ( -0.000000000000000000, -0.000000000000000000, -1.000000000000000000 ) ) ;
#36210 = CARTESIAN_POINT ( 'NONE',  ( -89.62287095715004170, -24.65952944569305316, 1.056160979905700348 ) ) ;
#36211 = CARTESIAN_POINT ( 'NONE',  ( -19.86366060283327784, 5.362777492974458049, -1.500000000000002220 ) ) ;
#36212 = CARTESIAN_POINT ( 'NONE',  ( -16.60028029328060128, 13.79055755010687356, 11.49999999999999645 ) ) ;
#36213 = EDGE_LOOP ( 'NONE', ( #87432, #1447, #14166, #60822 ) ) ;
#36214 = CARTESIAN_POINT ( 'NONE',  ( -91.63754064921776887, -23.73766607897670156, -1.055555164236454235 ) ) ;
#36215 = CARTESIAN_POINT ( 'NONE',  ( -128.5228709571500758, -29.50247984919015209, -1.443849546365044922 ) ) ;
#36216 = CARTESIAN_POINT ( 'NONE',  ( -129.6228709571500133, -24.51283580621365132, 0.6167428607019831421 ) ) ;
#36217 = CARTESIAN_POINT ( 'NONE',  ( -15.79502933763849271, 15.79022959414610661, 11.49999999999998934 ) ) ;
#36219 = CARTESIAN_POINT ( 'NONE',  ( -114.6228709571500559, -29.50248528299804818, 1.056150453629043584 ) ) ;
#36218 = VECTOR ( 'NONE', #11577, 1000.000000000000000 ) ;
#36220 = CARTESIAN_POINT ( 'NONE',  ( -84.51766577851211082, -23.73766607897669445, -1.055555164236457344 ) ) ;
#36221 = ORIENTED_EDGE ( 'NONE', *, *, #12024, .T. ) ;
#36222 = LINE ( 'NONE', #59070, #25801 ) ;
#36223 = CARTESIAN_POINT ( 'NONE',  ( -25.92875734969026169, 5.356774720514426491, 24.50402280011861933 ) ) ;
#36224 = CARTESIAN_POINT ( 'NONE',  ( 18.69404101259207707, 9.334567778723176446, -1.500000000000002220 ) ) ;
#36225 = ORIENTED_EDGE ( 'NONE', *, *, #71603, .T. ) ;
#36227 = EDGE_LOOP ( 'NONE', ( #85357, #42123, #70185, #18582 ) ) ;
#36226 = CARTESIAN_POINT ( 'NONE',  ( -39.32675481643261861, -25.19484965671346188, 3.363571302307362565 ) ) ;
#36228 = ORIENTED_EDGE ( 'NONE', *, *, #22043, .T. ) ;
#36229 = AXIS2_PLACEMENT_3D ( 'NONE', #6430, #37384, #67342 ) ;
#36230 = CARTESIAN_POINT ( 'NONE',  ( -100.5053545878111407, -24.92592662359561473, 8.075495903018000021 ) ) ;
#36231 = CARTESIAN_POINT ( 'NONE',  ( 9.152908845159860363, 19.05633030926415472, -1.500000000000002220 ) ) ;
#36232 = B_SPLINE_CURVE_WITH_KNOTS ( 'NONE', 3,
 ( #25810, #89212, #72997, #3486, #96816, #34424 ),
 .UNSPECIFIED., .F., .F.,
 ( 4, 2, 4 ),
 ( 0.000000000000000000, 0.001380764517854765182, 0.002761529035709530365 ),
 .UNSPECIFIED. ) ;
#36233 = ORIENTED_EDGE ( 'NONE', *, *, #89695, .F. ) ;
#36234 = CARTESIAN_POINT ( 'NONE',  ( -123.5228709571500616, -23.47596703998600631, 11.44779298504227860 ) ) ;
#36235 = LINE ( 'NONE', #50461, #40121 ) ;
#36236 = CARTESIAN_POINT ( 'NONE',  ( -110.6167804036481925, -25.20868619939636091, 6.586938478111401984 ) ) ;
#36237 = B_SPLINE_CURVE_WITH_KNOTS ( 'NONE', 3,
 ( #65676, #3269, #50429, #81371 ),
 .UNSPECIFIED., .F., .F.,
 ( 4, 4 ),
 ( 0.1599001052287878089, 0.1689065365009033703 ),
 .UNSPECIFIED. ) ;
#36238 = AXIS2_PLACEMENT_3D ( 'NONE', #73207, #89918, #89421 ) ;
#36239 = CARTESIAN_POINT ( 'NONE',  ( -76.54601064557617462, -24.35071581493543036, 9.817618358456028815 ) ) ;
#36240 = B_SPLINE_CURVE_WITH_KNOTS ( 'NONE', 3,
 ( #17374, #71169, #644, #39703, #9254, #48337 ),
 .UNSPECIFIED., .F., .F.,
 ( 4, 2, 4 ),
 ( 0.000000000000000000, 0.001380901958385385509, 0.002761803916770771018 ),
 .UNSPECIFIED. ) ;
#36241 = DIRECTION ( 'NONE',  ( 7.109281096390894329E-15, 0.000000000000000000, 1.000000000000000000 ) ) ;
#36242 = CARTESIAN_POINT ( 'NONE',  ( -21.33044368757495590, -4.375833669458513597, -1.500000000000002220 ) ) ;
#36243 = CARTESIAN_POINT ( 'NONE',  ( -78.94303308397304875, -25.27645460285955181, 5.977536667781793156 ) ) ;
#36245 = ORIENTED_EDGE ( 'NONE', *, *, #28067, .F. ) ;
#36244 = CARTESIAN_POINT ( 'NONE',  ( -15.79502933763849271, 15.79022959414610661, 11.49999999999999645 ) ) ;
#36246 = CARTESIAN_POINT ( 'NONE',  ( -116.6228709571500559, -23.47593901973091235, -1.443836447538997536 ) ) ;
#36247 = CARTESIAN_POINT ( 'NONE',  ( 7.052174998393318184, -6.376774720514418959, 20.39928653130861136 ) ) ;
#36248 = CARTESIAN_POINT ( 'NONE',  ( -31.55620429048340014, -24.64898659630528144, 1.056161002820817263 ) ) ;
#36249 = EDGE_LOOP ( 'NONE', ( #86496, #46934, #65019, #43044 ) ) ;
#36250 = VERTEX_POINT ( 'NONE', #48849 ) ;
#36251 = ORIENTED_EDGE ( 'NONE', *, *, #49557, .T. ) ;
#36252 = CARTESIAN_POINT ( 'NONE',  ( -116.5228709571500616, -23.47596703998600631, 11.44779298504227860 ) ) ;
#36253 = DIRECTION ( 'NONE',  ( -0.000000000000000000, 1.000000000000000000, -0.000000000000000000 ) ) ;
#36254 = CARTESIAN_POINT ( 'NONE',  ( 30.62809631291915835, -4.628857374213141362, 27.84496821199607908 ) ) ;
#36255 = CARTESIAN_POINT ( 'NONE',  ( -29.49875734969025842, 5.965225279485572685, 17.86602280011862476 ) ) ;
#36256 = CARTESIAN_POINT ( 'NONE',  ( -1.480291460309441920, -19.30061035156251847, 11.49999999999998934 ) ) ;
#36257 = DIRECTION ( 'NONE',  ( -0.7071067811865507924, -0.000000000000000000, -0.7071067811865442421 ) ) ;
#36258 = ORIENTED_EDGE ( 'NONE', *, *, #85502, .T. ) ;
#36259 = ADVANCED_FACE ( 'NONE', ( #70669 ), #18383, .T. ) ;
#36260 = CARTESIAN_POINT ( 'NONE',  ( -19.35591191756920892, -0.7100623379298715010, 11.49999999999999645 ) ) ;
#36261 = PLANE ( 'NONE',  #13104 ) ;
#36262 = ORIENTED_EDGE ( 'NONE', *, *, #67007, .F. ) ;
#36264 = CARTESIAN_POINT ( 'NONE',  ( 2.932009311892267434, -6.376774720514410077, 19.53174284846577891 ) ) ;
#36263 = VECTOR ( 'NONE', #75783, 1000.000000000000000 ) ;
#36265 = EDGE_CURVE ( 'NONE', #38164, #33103, #32098, .T. ) ;
#36266 = CARTESIAN_POINT ( 'NONE',  ( -11.64875734969026233, -5.965225279485572685, 30.51402280011862089 ) ) ;
#36267 = CARTESIAN_POINT ( 'NONE',  ( 3.509873074917118085, -0.3587747205144265483, 29.15869884040363758 ) ) ;
#36268 = EDGE_CURVE ( 'NONE', #21016, #12190, #76567, .T. ) ;
#36269 = PLANE ( 'NONE',  #52077 ) ;
#36270 = CARTESIAN_POINT ( 'NONE',  ( 18.24213732562919787, -7.162457363581539838, 11.49999999999998934 ) ) ;
#36271 = CIRCLE ( 'NONE', #44388, 129.7684398600581233 ) ;
#36272 = ADVANCED_FACE ( 'NONE', ( #71678 ), #2175, .F. ) ;
#36273 = CARTESIAN_POINT ( 'NONE',  ( 8.371512145086500212, -1.000000000000001110, 3.746884140868835367 ) ) ;
#36274 = VERTEX_POINT ( 'NONE', #87391 ) ;
#36275 = CARTESIAN_POINT ( 'NONE',  ( -20.03152041342270806, -8.007337437543776915, -1.500000000000002220 ) ) ;
#36276 = CARTESIAN_POINT ( 'NONE',  ( -33.57065171927310132, -23.48786465467240347, 11.44779295918255535 ) ) ;
#36277 = ADVANCED_FACE ( 'NONE', ( #79273 ), #86888, .T. ) ;
#36278 = CARTESIAN_POINT ( 'NONE',  ( -40.52287095715005449, -24.99132157543166244, 2.256160258750667502 ) ) ;
#36279 = PLANE ( 'NONE',  #65454 ) ;
#36281 = B_SPLINE_CURVE_WITH_KNOTS ( 'NONE', 3,
 ( #8306, #39248, #31635, #47376, #8810, #3706 ),
 .UNSPECIFIED., .F., .F.,
 ( 4, 2, 4 ),
 ( 0.000000000000000000, 0.001380764517854768652, 0.002761529035709537304 ),
 .UNSPECIFIED. ) ;
#36280 = CARTESIAN_POINT ( 'NONE',  ( 32.16024265030974050, 0.3587747205144265483, 16.27760796525321751 ) ) ;
#36282 = CARTESIAN_POINT ( 'NONE',  ( 21.12055942831636202, -9.126644407798330860, -1.500000000000002220 ) ) ;
#36283 = SHAPE_DEFINITION_REPRESENTATION ( #26338, #36681 ) ;
#36284 = DIRECTION ( 'NONE',  ( 0.000000000000000000, 0.000000000000000000, -1.000000000000000000 ) ) ;
#36285 = DIRECTION ( 'NONE',  ( 0.9685340172660599212, 0.000000000000000000, -0.2488812114211667037 ) ) ;
#36286 = CARTESIAN_POINT ( 'NONE',  ( -18.22032804147677254, 8.545885342870345625, 11.49999999999999645 ) ) ;
#36287 = CARTESIAN_POINT ( 'NONE',  ( -101.5895376238167245, -24.64898659630368627, 1.056161002820391381 ) ) ;
#36288 = CARTESIAN_POINT ( 'NONE',  ( -32.61006605916473688, -23.73791477778911485, 11.05961554403171299 ) ) ;
#36289 = CARTESIAN_POINT ( 'NONE',  ( -4.152941208099351300, -5.876774720514416295, 20.35309744218305639 ) ) ;
#36290 = FACE_OUTER_BOUND ( 'NONE', #75644, .T. ) ;
#36291 = CARTESIAN_POINT ( 'NONE',  ( -24.90875734969025501, 5.965225279485572685, 26.43402280011862615 ) ) ;
#36292 = CARTESIAN_POINT ( 'NONE',  ( 1.822157996128044299, -19.77364354024053839, -1.500000000000002220 ) ) ;
#36293 = VECTOR ( 'NONE', #88121, 1000.000000000000114 ) ;
#36294 = CARTESIAN_POINT ( 'NONE',  ( -47.55620429048339304, -24.66019654487199020, 8.947790411086135265 ) ) ;
#36295 = CARTESIAN_POINT ( 'NONE',  ( -12.15653940608521566, -15.58205587995076868, -1.500000000000002220 ) ) ;
#36296 = ADVANCED_FACE ( 'NONE', ( #16874 ), #17886, .F. ) ;
#36297 = CARTESIAN_POINT ( 'NONE',  ( 30.53060340732035982, 1.477225279485574028, 19.84760796525321425 ) ) ;
#36298 = DIRECTION ( 'NONE',  ( -0.000000000000000000, -0.000000000000000000, -1.000000000000000000 ) ) ;
#36299 = CARTESIAN_POINT ( 'NONE',  ( -2.243088942307695177, -6.376774720514408301, 19.14743589743590491 ) ) ;
#36300 = CARTESIAN_POINT ( 'NONE',  ( -12.00526669028610272, -16.82065764665920682, 11.49999999999999645 ) ) ;
#36301 = CARTESIAN_POINT ( 'NONE',  ( 8.071512145086531476, -9.528487854913507249, 1.734723475976807094E-15 ) ) ;
#36302 = CARTESIAN_POINT ( 'NONE',  ( 31.21773176006472283, 5.300046855345732943, 2.139914057118826651 ) ) ;
#36303 = CARTESIAN_POINT ( 'NONE',  ( 8.499999999999989342, 19.99999999999999289, 0.000000000000000000 ) ) ;
#36304 = CARTESIAN_POINT ( 'NONE',  ( -11.22117850230010738, 19.66027149220947123, 11.49999999999999645 ) ) ;
#36305 = EDGE_LOOP ( 'NONE', ( #73452, #59095, #36420, #94102 ) ) ;
#36306 = CARTESIAN_POINT ( 'NONE',  ( -107.5228709571500758, -29.50250786944525672, 11.44777988621622988 ) ) ;
#36307 = CARTESIAN_POINT ( 'NONE',  ( 29.70909950603835625, 4.224653874731083114, 27.99670097642948008 ) ) ;
#36308 = DIRECTION ( 'NONE',  ( -1.000000000000000000, -3.773278334444167608E-23, -8.201307833595939069E-29 ) ) ;
#36309 = DIRECTION ( 'NONE',  ( 0.000000000000000000, 0.000000000000000000, -1.000000000000000000 ) ) ;
#36310 = B_SPLINE_CURVE_WITH_KNOTS ( 'NONE', 3,
 ( #47793, #9212, #94959, #70622, #93952, #18338 ),
 .UNSPECIFIED., .F., .F.,
 ( 4, 2, 4 ),
 ( 1.570755371633698994E-05, 0.001396183895866086235, 0.002776660238015835579 ),
 .UNSPECIFIED. ) ;
#36311 = ORIENTED_EDGE ( 'NONE', *, *, #18756, .T. ) ;
#36312 = EDGE_LOOP ( 'NONE', ( #42585, #8156, #35359, #78476 ) ) ;
#36313 = CARTESIAN_POINT ( 'NONE',  ( -99.90107996939670443, -25.13963275720788815, 7.004612396290182730 ) ) ;
#36314 = CARTESIAN_POINT ( 'NONE',  ( -20.40978113611479827, 10.34812579263477872, -1.500000000000002220 ) ) ;
#36315 = FACE_OUTER_BOUND ( 'NONE', #37381, .T. ) ;
#36316 = CARTESIAN_POINT ( 'NONE',  ( 21.55061338234859392, -0.003183148592148328428, -1.500000000000002220 ) ) ;
#36317 = CARTESIAN_POINT ( 'NONE',  ( 13.91401389203221406, 6.475225279485573360, 158.0376437107427137 ) ) ;
#36318 = CARTESIAN_POINT ( 'NONE',  ( -65.52287095715011844, -24.83602698348160231, 1.605859176311265735 ) ) ;
#36319 = B_SPLINE_CURVE_WITH_KNOTS ( 'NONE', 3,
 ( #59032, #66164, #51414, #91448, #44306, #98061 ),
 .UNSPECIFIED., .F., .F.,
 ( 4, 2, 4 ),
 ( 0.000000000000000000, 0.0005107898210030669545, 0.001021579642006133909 ),
 .UNSPECIFIED. ) ;
#36320 = CARTESIAN_POINT ( 'NONE',  ( -11.40494320173684351, 19.43794304404440254, 11.49999999999999645 ) ) ;
#36321 = EDGE_LOOP ( 'NONE', ( #76900, #32969, #39836, #28612 ) ) ;
#36322 = CARTESIAN_POINT ( 'NONE',  ( -32.62287095715004881, -29.50250243563736774, 8.947779886222150481 ) ) ;
#36323 = CARTESIAN_POINT ( 'NONE',  ( 21.66556372666567754, 3.824538051775513647, 11.49999999999998934 ) ) ;
#36324 = CARTESIAN_POINT ( 'NONE',  ( -105.5487305842052308, -24.73531770709095312, 8.716586749053508498 ) ) ;
#36325 = CARTESIAN_POINT ( 'NONE',  ( -28.81656857143860861, -24.79700183405136116, 6.988807522033142483 ) ) ;
#36326 = EDGE_LOOP ( 'NONE', ( #78371, #55106, #17955 ) ) ;
#36327 = CARTESIAN_POINT ( 'NONE',  ( -48.61472421919472708, -23.48786465467241058, 11.44779295918254824 ) ) ;
#36328 = EDGE_CURVE ( 'NONE', #43445, #29369, #32605, .T. ) ;
#36329 = CARTESIAN_POINT ( 'NONE',  ( -90.54956613838091073, -24.40133493613049964, 9.663955038902805939 ) ) ;
#36330 = ORIENTED_EDGE ( 'NONE', *, *, #8611, .F. ) ;
#36331 = FACE_OUTER_BOUND ( 'NONE', #82619, .T. ) ;
#36332 = VERTEX_POINT ( 'NONE', #25494 ) ;
#36333 = VERTEX_POINT ( 'NONE', #40721 ) ;
#36334 = CARTESIAN_POINT ( 'NONE',  ( -126.5228709571500048, -23.94994826722564696, -0.6494450866342701412 ) ) ;
#36335 = PLANE ( 'NONE',  #14619 ) ;
#36336 = CARTESIAN_POINT ( 'NONE',  ( -36.66654255312141686, -23.48783264082477018, -1.443836473390095909 ) ) ;
#36337 = CARTESIAN_POINT ( 'NONE',  ( 12.54693703879240196, 16.07252283493236433, -1.500000000000002220 ) ) ;
#36338 = ADVANCED_FACE ( 'NONE', ( #56465 ), #72183, .T. ) ;
#36339 = VECTOR ( 'NONE', #33439, 1000.000000000000000 ) ;
#36340 = VERTEX_POINT ( 'NONE', #2672 ) ;
#36341 = CARTESIAN_POINT ( 'NONE',  ( -2.606012662418322634, -5.876774720514409189, 19.21974929698718881 ) ) ;
#36342 = CARTESIAN_POINT ( 'NONE',  ( -30.59755354180557418, -24.77158516743337913, 8.907023374642850655 ) ) ;
#36343 = CARTESIAN_POINT ( 'NONE',  ( -108.6228709571500559, -29.50248528299804818, 1.056150453629043584 ) ) ;
#36344 = DIRECTION ( 'NONE',  ( -1.000000000000000000, -0.000000000000000000, -0.000000000000000000 ) ) ;
#36345 = VERTEX_POINT ( 'NONE', #33609 ) ;
#36346 = DIRECTION ( 'NONE',  ( 0.000000000000000000, 0.000000000000000000, -1.000000000000000000 ) ) ;
#36347 = CARTESIAN_POINT ( 'NONE',  ( -28.13918514477506250, -24.63646054457999668, 8.204675463703699378 ) ) ;
#36348 = CARTESIAN_POINT ( 'NONE',  ( -8.262104503270727207, -19.10415460921518971, 11.49999999999998934 ) ) ;
#36349 = VERTEX_POINT ( 'NONE', #64592 ) ;
#36350 = APPROVAL ( #25679, 'UNKNOWN' ) ;
#36352 = ORIENTED_EDGE ( 'NONE', *, *, #72695, .F. ) ;
#36351 = DIRECTION ( 'NONE',  ( 0.9921023176230513441, 0.000000000000000000, -0.1254312216594016538 ) ) ;
#36353 = B_SPLINE_CURVE_WITH_KNOTS ( 'NONE', 3,
 ( #28879, #44607, #75534, #65475, #37490, #100358 ),
 .UNSPECIFIED., .F., .F.,
 ( 4, 2, 4 ),
 ( 0.000000000000000000, 0.001380901958385381606, 0.002761803916770763211 ),
 .UNSPECIFIED. ) ;
#36354 = CARTESIAN_POINT ( 'NONE',  ( -28.98875734969026396, -0.3587747205144265483, 2.362022800118626531 ) ) ;
#36355 = FACE_OUTER_BOUND ( 'NONE', #82144, .T. ) ;
#36356 = ORIENTED_EDGE ( 'NONE', *, *, #98582, .F. ) ;
#36357 = VERTEX_POINT ( 'NONE', #1163 ) ;
#36358 = CARTESIAN_POINT ( 'NONE',  ( -78.62287095715007013, -23.73907113216991860, -1.053371485793229700 ) ) ;
#36359 = CARTESIAN_POINT ( 'NONE',  ( -64.52287095715007581, -24.35013146730204170, 9.818937971375095941 ) ) ;
#36360 = DIRECTION ( 'NONE',  ( 0.000000000000000000, -1.000000000000000000, 0.000000000000000000 ) ) ;
#36361 = CARTESIAN_POINT ( 'NONE',  ( -74.62287095715005592, -23.47593901973091235, -1.443836447539006196 ) ) ;
#36363 = VERTEX_POINT ( 'NONE', #24984 ) ;
#36362 = CARTESIAN_POINT ( 'NONE',  ( -10.56713949322891999, -19.48831581008217384, 11.49999999999999645 ) ) ;
#36364 = B_SPLINE_CURVE_WITH_KNOTS ( 'NONE', 3,
 ( #7921, #23632, #76420, #15028 ),
 .UNSPECIFIED., .F., .F.,
 ( 4, 4 ),
 ( 0.5491634581351279021, 0.5501642051758932617 ),
 .UNSPECIFIED. ) ;
#36365 = CARTESIAN_POINT ( 'NONE',  ( -108.6247772082418948, -24.51314013834316086, 0.6176544820404235026 ) ) ;
#36366 = CARTESIAN_POINT ( 'NONE',  ( 11.26306171725914851, -19.60737681494043727, 11.49999999999998934 ) ) ;
#36368 = ORIENTED_EDGE ( 'NONE', *, *, #6475, .F. ) ;
#36367 = CARTESIAN_POINT ( 'NONE',  ( -115.5917237373192989, -24.15602025860897584, 10.28564288303533836 ) ) ;
#36369 = ORIENTED_EDGE ( 'NONE', *, *, #9242, .T. ) ;
#36370 = CARTESIAN_POINT ( 'NONE',  ( -71.52287095715007581, -29.50250243563736774, 8.947779886222143375 ) ) ;
#36371 = B_SPLINE_SURFACE_WITH_KNOTS ( 'NONE', 3, 1, ( 
 ( #64069, #72661 ),
 ( #96485, #11252 ),
 ( #9749, #87371 ),
 ( #71158, #73161 ),
 ( #25470, #55941 ),
 ( #25974, #79251 ),
 ( #41211, #32583 ),
 ( #33090, #95488 ),
 ( #26976, #17866 ),
 ( #47817, #94983 ),
 ( #80264, #94483 ),
 ( #63563, #17361 ),
 ( #56946, #40704 ),
 ( #80770, #3652 ),
 ( #78739, #48323 ),
 ( #72164, #33590 ),
 ( #87880, #9240 ),
 ( #3158, #41721 ),
 ( #2654, #10249 ) ),
 .UNSPECIFIED., .F., .F., .F.,
 ( 4, 1, 1, 1, 1, 1, 1, 1, 1, 1, 1, 1, 1, 1, 1, 1, 4 ),
 ( 2, 2 ),
 ( 0.000000000000000000, 0.06565904849408699118, 0.1292578964840137568, 0.1914365047840415057, 0.2527174969864875997, 0.3133199640703511202, 0.3744898936696244851, 0.4369089249503372852, 0.5009282752929569149, 0.5649763261437619200, 0.6271371978431706795, 0.6884541671478572322, 0.7490566342317193094, 0.8099329284035216014, 0.8715951039967769765, 0.9347691962579698366, 1.000000000000000000 ),
 ( 0.000000000000000000, 1.000000000000000000 ),
 .UNSPECIFIED. ) ;
#36372 = CARTESIAN_POINT ( 'NONE',  ( -28.52287095715005094, -23.31182002239687989, -1.443836447538998202 ) ) ;
#36373 = ORIENTED_EDGE ( 'NONE', *, *, #43321, .T. ) ;
#36374 = CARTESIAN_POINT ( 'NONE',  ( -0.3059464777392844059, -8.530684776139525027, 8.999999999999998224 ) ) ;
#36375 = CARTESIAN_POINT ( 'NONE',  ( 7.309977242446557888, -21.02818303981469583, -1.500000000000002220 ) ) ;
#36376 = CARTESIAN_POINT ( 'NONE',  ( -50.40895856474225667, -25.13941497071981246, 7.563173984875121825 ) ) ;
#36377 = ORIENTED_EDGE ( 'NONE', *, *, #51609, .T. ) ;
#36378 = DIRECTION ( 'NONE',  ( 0.000000000000000000, -1.000000000000000000, 0.000000000000000000 ) ) ;
#36379 = CARTESIAN_POINT ( 'NONE',  ( -120.6228709571500417, -29.50247984919015209, -1.443849546365046699 ) ) ;
#36380 = CARTESIAN_POINT ( 'NONE',  ( -26.97479289097202582, -24.58642771986267661, 1.762362389447201805 ) ) ;
#36381 = DIRECTION ( 'NONE',  ( 1.000000000000000000, 3.773278334444167608E-23, 8.201307810031802745E-29 ) ) ;
#36382 = CARTESIAN_POINT ( 'NONE',  ( -73.55620429048340725, -24.64965694238574656, 8.947790433994198267 ) ) ;
#36383 = CARTESIAN_POINT ( 'NONE',  ( -17.32436372870746055, -8.985247798433253053, 11.49999999999998934 ) ) ;
#36384 = ADVANCED_FACE ( 'NONE', ( #25993 ), #63072, .T. ) ;
#36385 = CARTESIAN_POINT ( 'NONE',  ( -19.15072323977689095, -9.709862252083167888, 11.49999999999998934 ) ) ;
#36386 = CARTESIAN_POINT ( 'NONE',  ( -25.56915516548917822, -24.58000038722270020, 4.121107147866038822 ) ) ;
#36387 = EDGE_CURVE ( 'NONE', #50456, #62223, #7883, .T. ) ;
#36388 = CARTESIAN_POINT ( 'NONE',  ( 24.71017632900190719, -3.356774720514427379, 1.647607965253211848 ) ) ;
#36389 = CARTESIAN_POINT ( 'NONE',  ( -85.52287095715006160, -23.48786465467241058, 11.44779295918254292 ) ) ;
#36391 = VECTOR ( 'NONE', #19682, 1000.000000000000114 ) ;
#36390 = CARTESIAN_POINT ( 'NONE',  ( -10.92962168092244823, 19.99562239114850826, -1.500000000000002220 ) ) ;
#36392 = SECURITY_CLASSIFICATION_LEVEL ( 'unclassified' ) ;
#36393 = LINE ( 'NONE', #35894, #36950 ) ;
#36394 = DIRECTION ( 'NONE',  ( -0.000000000000000000, 1.000000000000000000, -0.000000000000000000 ) ) ;
#36395 = CARTESIAN_POINT ( 'NONE',  ( -18.23705311251027794, 8.147635122911419003, 11.49999999999999645 ) ) ;
#36396 = CARTESIAN_POINT ( 'NONE',  ( -50.52287095715005449, -24.83602698348160231, 1.605859176311259073 ) ) ;
#36397 = CARTESIAN_POINT ( 'NONE',  ( -74.58443573574729157, -24.51419770103159124, 9.386484678747162747 ) ) ;
#36398 = LINE ( 'NONE', #100263, #26209 ) ;
#36399 = VERTEX_POINT ( 'NONE', #46453 ) ;
#36400 = ADVANCED_FACE ( 'NONE', ( #38834 ), #6889, .F. ) ;
#36401 = CARTESIAN_POINT ( 'NONE',  ( -27.61157986406360365, -24.60851323062442475, 1.630394788138983753 ) ) ;
#36402 = CARTESIAN_POINT ( 'NONE',  ( 33.74607884027702909, 0.3587747205144265483, -4.999864028243830916 ) ) ;
#36403 = AXIS2_PLACEMENT_3D ( 'NONE', #65550, #89358, #49820 ) ;
#36404 = CARTESIAN_POINT ( 'NONE',  ( 21.66353188042378974, 1.267531592894010739, -1.500000000000002220 ) ) ;
#36405 = CARTESIAN_POINT ( 'NONE',  ( -60.58953762381672448, -25.00158670708909270, 2.256160236439167299 ) ) ;
#36406 = CARTESIAN_POINT ( 'NONE',  ( -16.16875682573952133, 10.94412424577950915, -1.500000000000002220 ) ) ;
#36407 = CARTESIAN_POINT ( 'NONE',  ( -99.30650101624107151, -25.24758513798436610, 6.287525626990708716 ) ) ;
#36408 = ORIENTED_EDGE ( 'NONE', *, *, #62637, .F. ) ;
#36409 = DATE_AND_TIME ( #91681, #75028 ) ;
#36410 = CARTESIAN_POINT ( 'NONE',  ( -108.8968792378191921, -25.05712065398430966, 7.447789548358837663 ) ) ;
#36411 = DIRECTION ( 'NONE',  ( -0.9994733861282923959, 0.000000000000000000, -0.03244919754393515293 ) ) ;
#36412 = CARTESIAN_POINT ( 'NONE',  ( 12.80116962295325322, 15.99954467330607244, 11.49999999999999645 ) ) ;
#36413 = CARTESIAN_POINT ( 'NONE',  ( -49.73739581626914230, -25.30026926557708578, 5.371920104873852075 ) ) ;
#36414 = CARTESIAN_POINT ( 'NONE',  ( -40.55620429048340725, -23.48783264082477729, -1.443836473390073705 ) ) ;
#36415 = VERTEX_POINT ( 'NONE', #76876 ) ;
#36416 = CARTESIAN_POINT ( 'NONE',  ( -8.160000000000000142, 0.000000000000000000, 0.000000000000000000 ) ) ;
#36417 = CARTESIAN_POINT ( 'NONE',  ( -106.6228709571500559, -23.47596703998600631, 11.44779298504227860 ) ) ;
#36418 = CARTESIAN_POINT ( 'NONE',  ( -114.5228709571500758, -23.47593901973090524, -1.443836447538996204 ) ) ;
#36419 = CARTESIAN_POINT ( 'NONE',  ( 8.160000000000000142, -10.15233964170348457, 0.003711184059992174607 ) ) ;
#36420 = ORIENTED_EDGE ( 'NONE', *, *, #38473, .T. ) ;
#36421 = CARTESIAN_POINT ( 'NONE',  ( 32.45853543194704116, -5.965225279485572685, 9.169203677920338080 ) ) ;
#36422 = EDGE_CURVE ( 'NONE', #58657, #82541, #70481, .T. ) ;
#36423 = CARTESIAN_POINT ( 'NONE',  ( -13.44081803467414638, 18.71018530922267686, 11.49999999999999645 ) ) ;
#36424 = CARTESIAN_POINT ( 'NONE',  ( -13.85039312988123150, 18.09399583546626289, 11.49999999999998934 ) ) ;
#36425 = CARTESIAN_POINT ( 'NONE',  ( 3.063121397228215859, -6.376774720514420736, 20.95210102656095685 ) ) ;
#36426 = CARTESIAN_POINT ( 'NONE',  ( -40.52287095715006870, -23.47593901973090169, -1.443836447538997092 ) ) ;
#36427 = DIRECTION ( 'NONE',  ( 1.000000000000000000, 3.773278334444166432E-23, 8.201307841325785021E-29 ) ) ;
#36428 = AXIS2_PLACEMENT_3D ( 'NONE', #53998, #38749, #100125 ) ;
#36429 = CARTESIAN_POINT ( 'NONE',  ( -22.05275734969026047, 0.3587747205144262708, 31.02402280011862246 ) ) ;
#36430 = CARTESIAN_POINT ( 'NONE',  ( -110.5141208177188048, -24.52300882791530512, 0.6510814631126329299 ) ) ;
#36431 = CARTESIAN_POINT ( 'NONE',  ( 4.863445656156933694, -21.36585520573490626, -1.500000000000002220 ) ) ;
#36432 = EDGE_CURVE ( 'NONE', #27620, #21016, #37356, .T. ) ;
#36433 = CARTESIAN_POINT ( 'NONE',  ( 6.561060095583167495, -5.876774720514427841, 21.83518827598938117 ) ) ;
#36434 = FACE_OUTER_BOUND ( 'NONE', #8473, .T. ) ;
#36435 = CARTESIAN_POINT ( 'NONE',  ( -58.62287095715004881, -29.50250243563736774, 8.947779886222145151 ) ) ;
#36436 = CARTESIAN_POINT ( 'NONE',  ( -94.62287095715005592, -24.66019654487199730, 8.947790411086126383 ) ) ;
#36437 = CARTESIAN_POINT ( 'NONE',  ( -0.02075734969026423599, -0.3587747205144213303, -0.08597719988137648983 ) ) ;
#36438 = VERTEX_POINT ( 'NONE', #91619 ) ;
#36439 = CARTESIAN_POINT ( 'NONE',  ( -1.999887071766271784, 20.33596237858139233, -1.500000000000002220 ) ) ;
#36440 = ORIENTED_EDGE ( 'NONE', *, *, #46920, .T. ) ;
#36441 = B_SPLINE_CURVE_WITH_KNOTS ( 'NONE', 3,
 ( #91208, #8478, #83590, #76472, #21683, #7971, #52654, #14581 ),
 .UNSPECIFIED., .F., .F.,
 ( 4, 2, 2, 4 ),
 ( 0.000000000000000000, 0.002001098010032797709, 0.003001647015049196780, 0.004002196020065595418 ),
 .UNSPECIFIED. ) ;
#36442 = ORIENTED_EDGE ( 'NONE', *, *, #87942, .T. ) ;
#36443 = ORIENTED_EDGE ( 'NONE', *, *, #10615, .F. ) ;
#36444 = VERTEX_POINT ( 'NONE', #99715 ) ;
#36445 = CARTESIAN_POINT ( 'NONE',  ( -17.35246277222573141, 15.15038115719275424, 11.49999999999998934 ) ) ;
#36446 = CARTESIAN_POINT ( 'NONE',  ( -61.49452177658557872, -24.51314013834316086, 0.6176544820404138436 ) ) ;
#36447 = CARTESIAN_POINT ( 'NONE',  ( -0.6865706486018943178, -20.24796467851281179, -1.500000000000002220 ) ) ;
#36448 = VERTEX_POINT ( 'NONE', #23595 ) ;
#36449 = CARTESIAN_POINT ( 'NONE',  ( -27.13986186919794008, -25.04474643995085614, 5.848370260082334404 ) ) ;
#36450 = CARTESIAN_POINT ( 'NONE',  ( -87.62287095715001328, -23.48786465467241769, 11.44779295918254114 ) ) ;
#36451 = CARTESIAN_POINT ( 'NONE',  ( -95.62584188182231060, -24.83618233451450408, 1.606449574219538157 ) ) ;
#36452 = CARTESIAN_POINT ( 'NONE',  ( -41.62287095715006302, -24.33927499327853639, 9.819080762295824272 ) ) ;
#36454 = ORIENTED_EDGE ( 'NONE', *, *, #47832, .T. ) ;
#36453 = CARTESIAN_POINT ( 'NONE',  ( 5.910897418159350103, -20.63055655796343757, 11.49999999999999645 ) ) ;
#36455 = CARTESIAN_POINT ( 'NONE',  ( -55.62287095715005592, -29.50247984919015209, -1.443849546365056913 ) ) ;
#36456 = EDGE_LOOP ( 'NONE', ( #39560, #65587, #8164, #43309 ) ) ;
#36457 = CARTESIAN_POINT ( 'NONE',  ( 18.07348078632662691, -10.09602009226539288, -1.500000000000002220 ) ) ;
#36458 = VECTOR ( 'NONE', #71379, 1000.000000000000000 ) ;
#36459 = EDGE_CURVE ( 'NONE', #32994, #28964, #66896, .T. ) ;
#36460 = CC_DESIGN_PERSON_AND_ORGANIZATION_ASSIGNMENT ( #12432, #5819, ( #30849 ) ) ;
#36461 = ORIENTED_EDGE ( 'NONE', *, *, #87194, .T. ) ;
#36462 = CARTESIAN_POINT ( 'NONE',  ( -28.49465926560497309, -23.99116614675283543, -0.2315644524145782090 ) ) ;
#36463 = ORIENTED_EDGE ( 'NONE', *, *, #54781, .T. ) ;
#36464 = DIRECTION ( 'NONE',  ( 1.000000000000000000, 0.000000000000000000, 1.084136044942898696E-16 ) ) ;
#36465 = EDGE_LOOP ( 'NONE', ( #13565, #93225, #48807, #11261 ) ) ;
#36466 = CARTESIAN_POINT ( 'NONE',  ( 11.32296221242833667, -17.63459971646239310, -1.500000000000002220 ) ) ;
#36467 = CARTESIAN_POINT ( 'NONE',  ( -8.471812324360341151, -20.26817064352238162, 11.49999999999999645 ) ) ;
#36468 = AXIS2_PLACEMENT_3D ( 'NONE', #2533, #24850, #71543 ) ;
#36469 = DIRECTION ( 'NONE',  ( 0.000000000000000000, -1.000000000000000000, 0.000000000000000000 ) ) ;
#36470 = CARTESIAN_POINT ( 'NONE',  ( -5.199590022849982063, -21.90925200621149571, -1.500000000000002220 ) ) ;
#36471 = EDGE_CURVE ( 'NONE', #92240, #76194, #7380, .T. ) ;
#36472 = CIRCLE ( 'NONE', #15451, 7.652410033082758467 ) ;
#36473 = CARTESIAN_POINT ( 'NONE',  ( -17.07941033872765146, 12.18221932706078370, 11.49999999999998934 ) ) ;
#36474 = CARTESIAN_POINT ( 'NONE',  ( 6.431189903846153300, -6.376774720514415407, 20.08974358974358765 ) ) ;
#36475 = CARTESIAN_POINT ( 'NONE',  ( -119.5886893414437679, -24.51419770103158768, 9.386484678747159194 ) ) ;
#36476 = CARTESIAN_POINT ( 'NONE',  ( -8.978253834636468866, -5.876774720514426953, 21.48128695274316158 ) ) ;
#36477 = ORIENTED_EDGE ( 'NONE', *, *, #89716, .F. ) ;
#36478 = VERTEX_POINT ( 'NONE', #54565 ) ;
#36479 = VERTEX_POINT ( 'NONE', #22099 ) ;
#36480 = DIRECTION ( 'NONE',  ( -1.000000000000000000, -3.773278334444167608E-23, -8.201307833595939069E-29 ) ) ;
#36481 = CARTESIAN_POINT ( 'NONE',  ( -18.34654256122676941, -11.15389649534839833, -1.500000000000002220 ) ) ;
#36482 = DIRECTION ( 'NONE',  ( -1.000000000000000000, 0.000000000000000000, -0.000000000000000000 ) ) ;
#36483 = ORIENTED_EDGE ( 'NONE', *, *, #94702, .F. ) ;
#36484 = CARTESIAN_POINT ( 'NONE',  ( -13.65698368949537311, 16.12507722524849996, 11.49999999999998934 ) ) ;
#36485 = DIRECTION ( 'NONE',  ( 0.000000000000000000, 0.000000000000000000, -1.000000000000000000 ) ) ;
#36486 = CARTESIAN_POINT ( 'NONE',  ( -64.59767678124504187, -23.96119346886879953, -0.6495511937832134652 ) ) ;
#36487 = CYLINDRICAL_SURFACE ( 'NONE', #82656, 1.530000000000001359 ) ;
#36488 = DIRECTION ( 'NONE',  ( -1.000000000000000000, -0.000000000000000000, -0.000000000000000000 ) ) ;
#36489 = CARTESIAN_POINT ( 'NONE',  ( -100.3562339080374102, -25.11078286826155193, 2.834876632948881259 ) ) ;
#36490 = CARTESIAN_POINT ( 'NONE',  ( -21.57569705560537088, 4.917917830663471435, -1.500000000000002220 ) ) ;
#36491 = CARTESIAN_POINT ( 'NONE',  ( -116.5517209740605864, -24.65952944569305316, 1.056160979905712338 ) ) ;
#36492 = EDGE_CURVE ( 'NONE', #12606, #93033, #29306, .T. ) ;
#36493 = B_SPLINE_CURVE_WITH_KNOTS ( 'NONE', 3,
 ( #94783, #34894, #56749, #25270 ),
 .UNSPECIFIED., .F., .F.,
 ( 4, 4 ),
 ( 0.000000000000000000, 9.999999999998897304E-05 ),
 .UNSPECIFIED. ) ;
#36494 = LINE ( 'NONE', #66971, #6020 ) ;
#36495 = CARTESIAN_POINT ( 'NONE',  ( -9.940598223437577374, -5.876774720514426953, 22.08128695274315945 ) ) ;
#36496 = FACE_OUTER_BOUND ( 'NONE', #76084, .T. ) ;
#36497 = CARTESIAN_POINT ( 'NONE',  ( 10.34999999999998010, 27.69999999999999929, 2.100000000000000089 ) ) ;
#36498 = CARTESIAN_POINT ( 'NONE',  ( -18.22486019313910077, 6.713856318530649681, 11.49999999999998934 ) ) ;
#36499 = CARTESIAN_POINT ( 'NONE',  ( -17.73838780825237649, 11.93509662624355450, -1.500000000000002220 ) ) ;
#36500 = CARTESIAN_POINT ( 'NONE',  ( -26.29203710134576610, -24.90485257105619965, 6.397296682987914984 ) ) ;
#36501 = DIRECTION ( 'NONE',  ( 1.000000000000000000, 3.773278334444166432E-23, 8.201307841325785021E-29 ) ) ;
#36502 = EDGE_CURVE ( 'NONE', #23842, #73137, #87643, .T. ) ;
#36503 = CARTESIAN_POINT ( 'NONE',  ( -84.52287095715007581, -24.66019654487199730, 8.947790411086122830 ) ) ;
#36504 = CARTESIAN_POINT ( 'NONE',  ( -8.160000000000000142, -10.65233964170348635, -1.621096496867198589 ) ) ;
#36505 = CARTESIAN_POINT ( 'NONE',  ( 20.10346781357453949, 10.43426432342431553, -1.500000000000002220 ) ) ;
#36506 = ORIENTED_EDGE ( 'NONE', *, *, #38073, .F. ) ;
#36507 = CARTESIAN_POINT ( 'NONE',  ( -109.6228709571500559, -23.47593901973091235, -1.443836447538999312 ) ) ;
#36508 = CARTESIAN_POINT ( 'NONE',  ( -104.5228709571500758, -24.64965694238407323, 8.947790433994194714 ) ) ;
#36509 = CARTESIAN_POINT ( 'NONE',  ( -15.99800673754971037, 11.70972097625665675, 11.49999999999999645 ) ) ;
#36510 = PLANE ( 'NONE',  #43981 ) ;
#36511 = CARTESIAN_POINT ( 'NONE',  ( 10.86264265030973952, -0.3587747205144257157, -28.64597719988137570 ) ) ;
#36512 = EDGE_LOOP ( 'NONE', ( #60658, #15119, #20214, #50694 ) ) ;
#36513 = EDGE_CURVE ( 'NONE', #41593, #62694, #23094, .T. ) ;
#36514 = CARTESIAN_POINT ( 'NONE',  ( -5.891025641025639636, -6.376774720514420736, 20.75510817307693046 ) ) ;
#36515 = CARTESIAN_POINT ( 'NONE',  ( -29.81175120719462157, -25.26027006566499011, 4.942810958528816023 ) ) ;
#36516 = LINE ( 'NONE', #98405, #48244 ) ;
#36517 = CARTESIAN_POINT ( 'NONE',  ( 5.568959250215116619, -20.88136358707659923, 11.49999999999998934 ) ) ;
#36518 = CARTESIAN_POINT ( 'NONE',  ( -26.89577987079026045, -24.79392825080098461, 7.339462090957008300 ) ) ;
#36519 = CARTESIAN_POINT ( 'NONE',  ( 17.07123823605233781, 9.195568589125342029, -1.500000000000002220 ) ) ;
#36520 = ADVANCED_FACE ( 'NONE', ( #30727 ), #25615, .T. ) ;
#36521 = CARTESIAN_POINT ( 'NONE',  ( -10.28806225508158612, -4.941275956067651798, 28.69510307482446976 ) ) ;
#36522 = CARTESIAN_POINT ( 'NONE',  ( -35.62287095715006302, -24.63287334234179227, 0.9662140553045417413 ) ) ;
#36523 = CARTESIAN_POINT ( 'NONE',  ( -19.37706247964952411, -4.161318200553020041, 11.49999999999998934 ) ) ;
#36524 = ORIENTED_EDGE ( 'NONE', *, *, #46363, .F. ) ;
#36525 = CARTESIAN_POINT ( 'NONE',  ( 20.34676669208793953, -0.1217515720461415790, 11.49999999999999645 ) ) ;
#36526 = CARTESIAN_POINT ( 'NONE',  ( -119.5228709571500616, -24.66019654487200441, 8.947790411086108620 ) ) ;
#36527 = AXIS2_PLACEMENT_3D ( 'NONE', #98437, #89844, #37052 ) ;
#36528 = VECTOR ( 'NONE', #8357, 1000.000000000000000 ) ;
#36529 = CARTESIAN_POINT ( 'NONE',  ( 6.650000000000004796, 0.000000000000000000, 19.30000000000000071 ) ) ;
#36530 = ORIENTED_EDGE ( 'NONE', *, *, #95403, .F. ) ;
#36531 = CARTESIAN_POINT ( 'NONE',  ( -102.5170194679072182, -23.96169478059713853, 10.65365249895717881 ) ) ;
#36532 = LINE ( 'NONE', #14691, #23392 ) ;
#36533 = CARTESIAN_POINT ( 'NONE',  ( -44.62287095715006302, -23.96127896941632685, -0.6493128931037885909 ) ) ;
#36534 = DIRECTION ( 'NONE',  ( 0.000000000000000000, 1.000000000000000000, 0.000000000000000000 ) ) ;
#36535 = CIRCLE ( 'NONE', #912, 6.099999999999999645 ) ;
#36536 = CARTESIAN_POINT ( 'NONE',  ( -87.22287095715006444, -23.47596703998600631, 11.44779298504227860 ) ) ;
#36537 = CARTESIAN_POINT ( 'NONE',  ( -1.290058840521481454, 20.04182742388497473, 11.49999999999998934 ) ) ;
#36538 = AXIS2_PLACEMENT_3D ( 'NONE', #67078, #67570, #59960 ) ;
#36539 = LINE ( 'NONE', #46161, #69421 ) ;
#36540 = VERTEX_POINT ( 'NONE', #15987 ) ;
#36541 = VECTOR ( 'NONE', #3245, 1000.000000000000000 ) ;
#36542 = CARTESIAN_POINT ( 'NONE',  ( -21.19308438721250099, -8.479022899233653376, 11.49999999999999645 ) ) ;
#36543 = LINE ( 'NONE', #38045, #25875 ) ;
#36544 = CARTESIAN_POINT ( 'NONE',  ( -86.62287095715005592, -24.50216790748099527, 0.6166512839513639266 ) ) ;
#36545 = DIRECTION ( 'NONE',  ( 0.6451914333552788428, 0.000000000000000000, 0.7640209514960704107 ) ) ;
#36546 = CARTESIAN_POINT ( 'NONE',  ( 5.981014360695730225, -5.876774720514425177, 21.36744920115099333 ) ) ;
#36547 = DIRECTION ( 'NONE',  ( 3.773278334444167608E-23, -1.000000000000000000, 0.000000000000000000 ) ) ;
#36548 = EDGE_CURVE ( 'NONE', #16850, #17644, #8386, .T. ) ;
#36549 = CARTESIAN_POINT ( 'NONE',  ( -19.61019785865472542, -10.87575402790796453, 11.49999999999999645 ) ) ;
#36550 = CARTESIAN_POINT ( 'NONE',  ( -98.87749449787162348, -25.03707831087709934, 7.590867751134624974 ) ) ;
#36551 = ORIENTED_EDGE ( 'NONE', *, *, #89314, .T. ) ;
#36552 = CARTESIAN_POINT ( 'NONE',  ( 20.27773211485958527, -1.686570798567030183, 11.49999999999998934 ) ) ;
#36553 = ORIENTED_EDGE ( 'NONE', *, *, #23466, .F. ) ;
#36554 = CARTESIAN_POINT ( 'NONE',  ( -11.38079350637645959, -19.95400817559217899, 11.49999999999998934 ) ) ;
#36555 = CARTESIAN_POINT ( 'NONE',  ( -37.58953762381673158, -24.65952944569304606, 1.056160979905692798 ) ) ;
#36556 = ORIENTED_EDGE ( 'NONE', *, *, #19698, .T. ) ;
#36557 = CARTESIAN_POINT ( 'NONE',  ( 13.91401389203221406, 6.376774720514426953, 27.24920385068457662 ) ) ;
#36558 = DIRECTION ( 'NONE',  ( -0.000000000000000000, 1.000000000000000000, -0.000000000000000000 ) ) ;
#36559 = LINE ( 'NONE', #74624, #1048 ) ;
#36561 = VERTEX_POINT ( 'NONE', #33730 ) ;
#36560 = CARTESIAN_POINT ( 'NONE',  ( -8.014198274750887308, -19.69740135394370384, 11.49999999999999645 ) ) ;
#36562 = VECTOR ( 'NONE', #66659, 1000.000000000000000 ) ;
#36563 = B_SPLINE_CURVE_WITH_KNOTS ( 'NONE', 3,
 ( #31412, #456, #78066, #24790, #92303, #47651 ),
 .UNSPECIFIED., .F., .F.,
 ( 4, 2, 4 ),
 ( 0.000000000000000000, 0.001381645784125716319, 0.002763291568251432639 ),
 .UNSPECIFIED. ) ;
#36564 = EDGE_LOOP ( 'NONE', ( #82614, #91530, #69532, #59074 ) ) ;
#36565 = CARTESIAN_POINT ( 'NONE',  ( -19.05511597014879044, -11.33806725510066826, 11.49999999999998934 ) ) ;
#36566 = CARTESIAN_POINT ( 'NONE',  ( -3.087264924507187924, 20.40197043678811539, -1.500000000000002220 ) ) ;
#36567 = EDGE_CURVE ( 'NONE', #8977, #66223, #119, .T. ) ;
#36568 = ORIENTED_EDGE ( 'NONE', *, *, #59411, .T. ) ;
#36569 = ORIENTED_EDGE ( 'NONE', *, *, #89257, .F. ) ;
#36570 = CARTESIAN_POINT ( 'NONE',  ( 6.403846153846157740, -6.376774720514426065, 21.48076923076922995 ) ) ;
#36571 = CARTESIAN_POINT ( 'NONE',  ( 2.708118538500707828, -5.876774720514424288, 20.94830092343283212 ) ) ;
#36572 = ORIENTED_EDGE ( 'NONE', *, *, #34205, .F. ) ;
#36573 = EDGE_CURVE ( 'NONE', #38454, #77746, #58450, .T. ) ;
#36574 = EDGE_LOOP ( 'NONE', ( #50858, #85009, #332, #4550 ) ) ;
#36575 = CARTESIAN_POINT ( 'NONE',  ( 30.57144966832858302, 5.048887879205125273, 25.33340266839140398 ) ) ;
#36576 = CARTESIAN_POINT ( 'NONE',  ( -29.49875734969025842, -5.965225279485572685, 25.61802280011862720 ) ) ;
#36577 = DIRECTION ( 'NONE',  ( 0.000000000000000000, 0.000000000000000000, -1.000000000000000000 ) ) ;
#36578 = CARTESIAN_POINT ( 'NONE',  ( -20.76960556195881225, -0.3855258213679747525, -1.500000000000002220 ) ) ;
#36579 = CARTESIAN_POINT ( 'NONE',  ( 1.329761939549756855, 21.69843865049760367, 11.49999999999999645 ) ) ;
#36580 = EDGE_LOOP ( 'NONE', ( #9631, #35102, #1625, #74228 ) ) ;
#36581 = CARTESIAN_POINT ( 'NONE',  ( -40.52227049441191298, -25.31583770613250195, 5.079412502965257481 ) ) ;
#36582 = DIRECTION ( 'NONE',  ( 0.000000000000000000, -5.204170427930421283E-15, 1.000000000000000000 ) ) ;
#36583 = CARTESIAN_POINT ( 'NONE',  ( -115.6250729497555909, -24.73486907724917927, 1.287355809206966573 ) ) ;
#36584 = CARTESIAN_POINT ( 'NONE',  ( 15.48037617655995923, 16.25473645317415361, 11.49999999999998934 ) ) ;
#36585 = ADVANCED_FACE ( 'NONE', ( #72297 ), #95628, .T. ) ;
#36586 = EDGE_CURVE ( 'NONE', #96543, #6499, #26060, .T. ) ;
#36587 = CARTESIAN_POINT ( 'NONE',  ( -51.22891850606554698, -25.26334649059542059, 4.264007109377201843 ) ) ;
#36588 = ORIENTED_EDGE ( 'NONE', *, *, #13718, .T. ) ;
#36589 = B_SPLINE_CURVE_WITH_KNOTS ( 'NONE', 3,
 ( #56733, #10533, #57236, #2433 ),
 .UNSPECIFIED., .F., .F.,
 ( 4, 4 ),
 ( 0.000000000000000000, 9.999999999998897304E-05 ),
 .UNSPECIFIED. ) ;
#36590 = CARTESIAN_POINT ( 'NONE',  ( -75.52287095715006160, -24.99132157543084176, 2.256160258750667502 ) ) ;
#36591 = DIRECTION ( 'NONE',  ( 0.000000000000000000, 0.000000000000000000, 1.000000000000000000 ) ) ;
#36592 = EDGE_CURVE ( 'NONE', #53085, #18133, #1782, .T. ) ;
#36593 = ORIENTED_EDGE ( 'NONE', *, *, #18741, .F. ) ;
#36594 = VERTEX_POINT ( 'NONE', #18001 ) ;
#36595 = DIRECTION ( 'NONE',  ( -1.000000000000000000, -3.773278334444167608E-23, -8.201307833595939069E-29 ) ) ;
#36596 = ORIENTED_EDGE ( 'NONE', *, *, #807, .F. ) ;
#36597 = CIRCLE ( 'NONE', #54494, 0.8500000000000017542 ) ;
#36598 = CARTESIAN_POINT ( 'NONE',  ( 1.434216325579209750, -21.26356369375713484, -1.500000000000002220 ) ) ;
#36599 = EDGE_LOOP ( 'NONE', ( #67562, #78182, #46068, #5421 ) ) ;
#36600 = CARTESIAN_POINT ( 'NONE',  ( -80.58953762381671027, -25.00182538069145366, 7.747789668545099317 ) ) ;
#36601 = VECTOR ( 'NONE', #39607, 1000.000000000000000 ) ;
#36602 = CARTESIAN_POINT ( 'NONE',  ( -17.33045254171255678, -11.89390297951003816, -1.500000000000002220 ) ) ;
#36603 = DIRECTION ( 'NONE',  ( -0.000000000000000000, 1.000000000000000000, -0.000000000000000000 ) ) ;
#36604 = CARTESIAN_POINT ( 'NONE',  ( 17.32531159343115945, 14.66459048539768162, 11.49999999999998934 ) ) ;
#36605 = CARTESIAN_POINT ( 'NONE',  ( -99.53443088461749255, -25.25502385701537023, 3.893674835496924391 ) ) ;
#36606 = AXIS2_PLACEMENT_3D ( 'NONE', #82319, #89440, #96054 ) ;
#36607 = FACE_OUTER_BOUND ( 'NONE', #86859, .T. ) ;
#36608 = CARTESIAN_POINT ( 'NONE',  ( -3.478157889954244464, -21.63767827151469447, -1.500000000000002220 ) ) ;
#36609 = DIRECTION ( 'NONE',  ( 0.000000000000000000, -2.173523156925980399E-06, 0.9999999999976378895 ) ) ;
#36610 = VERTEX_POINT ( 'NONE', #63193 ) ;
#36611 = CARTESIAN_POINT ( 'NONE',  ( -40.49165087243459737, -25.29352311369862605, 5.543942880681965946 ) ) ;
#36612 = EDGE_CURVE ( 'NONE', #26949, #30746, #19606, .T. ) ;
#36613 = VECTOR ( 'NONE', #29386, 1000.000000000000114 ) ;
#36614 = AXIS2_PLACEMENT_3D ( 'NONE', #32809, #64287, #70883 ) ;
#36615 = ORIENTED_EDGE ( 'NONE', *, *, #52069, .F. ) ;
#36616 = CARTESIAN_POINT ( 'NONE',  ( -120.5228709571500900, -24.82558206586149652, 1.605769216559630008 ) ) ;
#36617 = DIRECTION ( 'NONE',  ( 0.000000000000000000, -0.000000000000000000, -1.000000000000000000 ) ) ;
#36618 = CARTESIAN_POINT ( 'NONE',  ( -20.42273151058504510, -23.87832360206071769, 1.095224832288504091 ) ) ;
#36619 = CARTESIAN_POINT ( 'NONE',  ( 17.81766572339076404, -11.58780717566545526, 11.49999999999998934 ) ) ;
#36620 = CARTESIAN_POINT ( 'NONE',  ( -112.5161646695722766, -24.34968618360934656, 0.1864209137779000991 ) ) ;
#36621 = CARTESIAN_POINT ( 'NONE',  ( -26.09636659181000695, -24.97064981342374423, 4.940287549563596059 ) ) ;
#36622 = EDGE_CURVE ( 'NONE', #21715, #70027, #78906, .T. ) ;
#36623 = CARTESIAN_POINT ( 'NONE',  ( -85.63412233528902107, -24.40034930558991633, 0.3402023900116044608 ) ) ;
#36624 = CARTESIAN_POINT ( 'NONE',  ( -33.56120742164601722, -23.73766607897670866, -1.055555164236444687 ) ) ;
#36625 = ADVANCED_FACE ( 'NONE', ( #33222 ), #2292, .F. ) ;
#36626 = DIRECTION ( 'NONE',  ( -3.773278334453079618E-23, 0.9999999999976377785, 2.173523156925979975E-06 ) ) ;
#36627 = ORIENTED_EDGE ( 'NONE', *, *, #97429, .F. ) ;
#36628 = DIRECTION ( 'NONE',  ( -3.773278334444167608E-23, 1.000000000000000000, 0.000000000000000000 ) ) ;
#36629 = CARTESIAN_POINT ( 'NONE',  ( 18.19143915067776263, 7.407926943018095400, 11.49999999999999645 ) ) ;
#36630 = CARTESIAN_POINT ( 'NONE',  ( -28.98875734969026396, 3.316774720514426456, -0.08597719988137648983 ) ) ;
#36631 = CARTESIAN_POINT ( 'NONE',  ( -100.6228709571500559, -24.99156045073393173, 7.747789690856161648 ) ) ;
#36632 = VERTEX_POINT ( 'NONE', #775 ) ;
#36633 = EDGE_CURVE ( 'NONE', #66681, #2671, #53398, .T. ) ;
#36634 = CARTESIAN_POINT ( 'NONE',  ( -88.62358605409035306, -24.66019654487199730, 8.947790411086115725 ) ) ;
#36635 = CARTESIAN_POINT ( 'NONE',  ( -99.45104055277701605, -25.31439635812596478, 5.670438249640629813 ) ) ;
#36637 = EDGE_CURVE ( 'NONE', #38812, #68323, #89701, .T. ) ;
#36636 = CARTESIAN_POINT ( 'NONE',  ( -25.78296037513418781, -24.81720370909834017, 6.769897328156279315 ) ) ;
#36638 = DIRECTION ( 'NONE',  ( -4.335561085774420994E-16, -0.000000000000000000, 1.000000000000000000 ) ) ;
#36639 = CARTESIAN_POINT ( 'NONE',  ( -16.05533900033903549, 11.45903963230415101, 11.49999999999998934 ) ) ;
#36640 = EDGE_CURVE ( 'NONE', #82984, #47723, #55578, .T. ) ;
#36641 = ORIENTED_EDGE ( 'NONE', *, *, #50274, .F. ) ;
#36642 = CARTESIAN_POINT ( 'NONE',  ( 10.59058046163345423, 3.703784075859317682, -26.99573265033922453 ) ) ;
#36643 = CARTESIAN_POINT ( 'NONE',  ( -70.62287095715009855, -24.83602698348160587, 1.605859176311266845 ) ) ;
#36644 = B_SPLINE_CURVE_WITH_KNOTS ( 'NONE', 3,
 ( #63991, #72584, #62463, #16277 ),
 .UNSPECIFIED., .F., .F.,
 ( 4, 4 ),
 ( 0.000000000000000000, 0.0001000000000000098033 ),
 .UNSPECIFIED. ) ;
#36645 = B_SPLINE_CURVE_WITH_KNOTS ( 'NONE', 3,
 ( #13999, #37361, #45477, #46459, #77389, #98238, #53089, #59706 ),
 .UNSPECIFIED., .F., .F.,
 ( 4, 2, 2, 4 ),
 ( 0.000000000000000000, 0.003897507692133500394, 0.005846261538200250157, 0.007795015384267000788 ),
 .UNSPECIFIED. ) ;
#36647 = EDGE_CURVE ( 'NONE', #97579, #28117, #87008, .T. ) ;
#36646 = PERSON_AND_ORGANIZATION_ROLE ( 'creator' ) ;
#36648 = ORIENTED_EDGE ( 'NONE', *, *, #24445, .F. ) ;
#36649 = DIRECTION ( 'NONE',  ( -0.000000000000000000, 0.000000000000000000, 1.000000000000000000 ) ) ;
#36650 = CARTESIAN_POINT ( 'NONE',  ( -69.58953762381672448, -24.66019654487198665, 8.947790411086131712 ) ) ;
#36651 = CARTESIAN_POINT ( 'NONE',  ( -55.53128016475043438, -24.83618233451448987, 1.606449574219538379 ) ) ;
#36652 = DIRECTION ( 'NONE',  ( 3.773278334444166432E-23, -1.000000000000000000, 0.000000000000000000 ) ) ;
#36653 = CARTESIAN_POINT ( 'NONE',  ( -7.188523146553190912, -6.376774720514413630, 19.66116880005639800 ) ) ;
#36654 = LINE ( 'NONE', #91426, #91095 ) ;
#36655 = CARTESIAN_POINT ( 'NONE',  ( 22.81105451610979173, -2.682774720540237468, -18.46691820600746681 ) ) ;
#36656 = CARTESIAN_POINT ( 'NONE',  ( 6.038693664686949347, 19.05185810397003721, -1.500000000000002220 ) ) ;
#36657 = DIRECTION ( 'NONE',  ( -0.1736481776669261679, 0.9848077530122087975, 0.000000000000000000 ) ) ;
#36658 = CARTESIAN_POINT ( 'NONE',  ( -0.07101499051468204704, -22.13065514132824418, 9.689530304921902371 ) ) ;
#36659 = VERTEX_POINT ( 'NONE', #88519 ) ;
#36660 = CARTESIAN_POINT ( 'NONE',  ( -63.52287095715004739, -23.47593901973090169, -1.443836447538996870 ) ) ;
#36661 = LINE ( 'NONE', #90449, #47377 ) ;
#36662 = AXIS2_PLACEMENT_3D ( 'NONE', #23849, #16244, #8639 ) ;
#36663 = DIRECTION ( 'NONE',  ( 0.6599726524652352877, 0.000000000000000000, -0.7512896232465891000 ) ) ;
#36664 = CARTESIAN_POINT ( 'NONE',  ( -19.69812919673063689, 5.965225279485592225, -22.00173861453435720 ) ) ;
#36665 = CARTESIAN_POINT ( 'NONE',  ( -28.62287095715004881, -24.49608681932686949, 1.056161686216224860 ) ) ;
#36666 = CARTESIAN_POINT ( 'NONE',  ( -39.56088500995654300, -23.73766607897669800, -1.055555164236461341 ) ) ;
#36667 = CARTESIAN_POINT ( 'NONE',  ( -101.5468792378191836, -25.25287247409163527, 6.236250661346386615 ) ) ;
#36668 = CARTESIAN_POINT ( 'NONE',  ( -51.66173670239771099, -25.26279960158665006, 4.265171648276663063 ) ) ;
#36669 = AXIS2_PLACEMENT_3D ( 'NONE', #37170, #53404, #45782 ) ;
#36670 = EDGE_LOOP ( 'NONE', ( #47857, #21973, #72557, #10414 ) ) ;
#36671 = DIRECTION ( 'NONE',  ( 3.773278334444166432E-23, -1.000000000000000000, 0.000000000000000000 ) ) ;
#36673 = AXIS2_PLACEMENT_3D ( 'NONE', #52187, #76997, #76002 ) ;
#36672 = DIRECTION ( 'NONE',  ( -3.773278334453079030E-23, 0.9999999999976377785, 2.173523156925979128E-06 ) ) ;
#36674 = ORIENTED_EDGE ( 'NONE', *, *, #547, .T. ) ;
#36675 = VECTOR ( 'NONE', #88508, 1000.000000000000114 ) ;
#36676 = CARTESIAN_POINT ( 'NONE',  ( -15.67655817637044890, 12.86142704545212290, 11.49999999999998934 ) ) ;
#36677 = CARTESIAN_POINT ( 'NONE',  ( -122.5572046973127698, -23.48783264082477373, -1.443836473390087471 ) ) ;
#36678 = PLANE ( 'NONE',  #92281 ) ;
#36679 = AXIS2_PLACEMENT_3D ( 'NONE', #10458, #9962, #49042 ) ;
#36680 = PLANE ( 'NONE',  #76791 ) ;
#36681 = SHAPE_REPRESENTATION ( 'Tape Measure Hook', ( #37391 ), #14765 ) ;
#36682 = B_SPLINE_CURVE_WITH_KNOTS ( 'NONE', 3,
 ( #30165, #92066, #14936, #46899, #69739, #17441 ),
 .UNSPECIFIED., .F., .F.,
 ( 4, 2, 4 ),
 ( 0.000000000000000000, 0.001380764517854760846, 0.002761529035709521691 ),
 .UNSPECIFIED. ) ;
#36683 = ORIENTED_EDGE ( 'NONE', *, *, #69005, .T. ) ;
#36684 = CARTESIAN_POINT ( 'NONE',  ( -40.43756433397305727, -29.50248914370730091, 2.832395270851967073 ) ) ;
#36685 = CARTESIAN_POINT ( 'NONE',  ( -46.52287095715006160, -24.64965694238406613, 8.947790433994203596 ) ) ;
#36686 = CARTESIAN_POINT ( 'NONE',  ( 16.02535498940104830, 12.03463022438520191, -1.500000000000002220 ) ) ;
#36687 = CARTESIAN_POINT ( 'NONE',  ( 16.98782256641479904, -12.52229676876588371, 11.49999999999999645 ) ) ;
#36688 = CARTESIAN_POINT ( 'NONE',  ( -28.37365055580376350, -24.90401935843307157, 7.412184485816843527 ) ) ;
#36689 = DIRECTION ( 'NONE',  ( -0.000000000000000000, 1.000000000000000000, -0.000000000000000000 ) ) ;
#36690 = CARTESIAN_POINT ( 'NONE',  ( 7.254013858510784729, 20.86747967231135803, 11.49999999999998934 ) ) ;
#36691 = CARTESIAN_POINT ( 'NONE',  ( 7.908618202329199320, -18.92053725880622039, 11.49999999999998934 ) ) ;
#36692 = CARTESIAN_POINT ( 'NONE',  ( -36.62287095715005592, -29.50248528299804818, 1.056150453629031594 ) ) ;
#36693 = EDGE_CURVE ( 'NONE', #31601, #81299, #72797, .T. ) ;
#36694 = CARTESIAN_POINT ( 'NONE',  ( 31.74473449900405697, 4.976825198871215328, -4.259190951192157293 ) ) ;
#36695 = LINE ( 'NONE', #69135, #55773 ) ;
#36696 = ORIENTED_EDGE ( 'NONE', *, *, #31131, .F. ) ;
#36697 = DIRECTION ( 'NONE',  ( -0.000000000000000000, 0.000000000000000000, -1.000000000000000000 ) ) ;
#36698 = CARTESIAN_POINT ( 'NONE',  ( -67.62287095715004170, -23.95044443724991368, 10.65354141964649592 ) ) ;
#36699 = EDGE_CURVE ( 'NONE', #57603, #57780, #86093, .T. ) ;
#36700 = EDGE_LOOP ( 'NONE', ( #68101, #60067, #19069, #5507 ) ) ;
#36701 = VERTEX_POINT ( 'NONE', #59076 ) ;
#36702 = CARTESIAN_POINT ( 'NONE',  ( -54.62287095715005592, -29.50248528299804818, 1.056150453629033370 ) ) ;
#36703 = CARTESIAN_POINT ( 'NONE',  ( -127.6228709571500559, -24.64965695001469115, 8.947790433994173398 ) ) ;
#36704 = CARTESIAN_POINT ( 'NONE',  ( -62.22287095715002891, -23.47593901973090524, -1.443836447538997758 ) ) ;
#36705 = CARTESIAN_POINT ( 'NONE',  ( -18.72588118538106272, -8.511115862834014223, -1.500000000000002220 ) ) ;
#36706 = EDGE_CURVE ( 'NONE', #38639, #71522, #90012, .T. ) ;
#36707 = CARTESIAN_POINT ( 'NONE',  ( 4.075586527997184128, 21.15050231453075824, 11.49999999999999645 ) ) ;
#36708 = ORIENTED_EDGE ( 'NONE', *, *, #52048, .F. ) ;
#36709 = PLANE ( 'NONE',  #59647 ) ;
#36710 = AXIS2_PLACEMENT_3D ( 'NONE', #84622, #62304, #46572 ) ;
#36711 = PLANE ( 'NONE',  #59360 ) ;
#36712 = CARTESIAN_POINT ( 'NONE',  ( 5.437191932089902480, -21.69250089042843754, -1.500000000000002220 ) ) ;
#36713 = EDGE_CURVE ( 'NONE', #29762, #7487, #44961, .T. ) ;
#36714 = ADVANCED_FACE ( 'NONE', ( #89510 ), #41858, .T. ) ;
#36715 = DIRECTION ( 'NONE',  ( -3.773278334453079030E-23, 0.9999999999976377785, 2.173523156925979128E-06 ) ) ;
#36716 = PLANE ( 'NONE',  #15670 ) ;
#36717 = EDGE_LOOP ( 'NONE', ( #44149, #63575 ) ) ;
#36718 = CARTESIAN_POINT ( 'NONE',  ( -20.27875734969026311, -6.376774720514428729, 21.00402280011862644 ) ) ;
#36719 = FACE_OUTER_BOUND ( 'NONE', #97592, .T. ) ;
#36720 = ADVANCED_FACE ( 'NONE', ( #51454 ), #88019, .T. ) ;
#36721 = CARTESIAN_POINT ( 'NONE',  ( 20.89859092893058801, 0.06103081833375877813, -1.500000000000002220 ) ) ;
#36722 = VERTEX_POINT ( 'NONE', #65210 ) ;
#36724 = VERTEX_POINT ( 'NONE', #57582 ) ;
#36723 = CARTESIAN_POINT ( 'NONE',  ( -86.62887871871048162, -24.34968618360933945, 0.1864209137778916059 ) ) ;
#36725 = ORIENTED_EDGE ( 'NONE', *, *, #62439, .T. ) ;
#36726 = CARTESIAN_POINT ( 'NONE',  ( -32.62287095715004881, -29.50247984919015209, -1.443849546365062242 ) ) ;
#36727 = CARTESIAN_POINT ( 'NONE',  ( 5.994809752082427501, 20.21905721239408393, -1.500000000000002220 ) ) ;
#36728 = ORIENTED_EDGE ( 'NONE', *, *, #10615, .T. ) ;
#36729 = CARTESIAN_POINT ( 'NONE',  ( -117.5188432126315519, -24.15543982623907837, -0.2315651400026547124 ) ) ;
#36730 = CARTESIAN_POINT ( 'NONE',  ( 6.727764423076923350, -5.876774720514413630, 19.76442307692307665 ) ) ;
#36731 = DIRECTION ( 'NONE',  ( -3.773278334453079618E-23, 0.9999999999976377785, 2.173523156925979975E-06 ) ) ;
#36732 = CARTESIAN_POINT ( 'NONE',  ( -90.62287095715004170, -23.47596703998600631, 11.44779298504227860 ) ) ;
#36733 = CARTESIAN_POINT ( 'NONE',  ( 7.477175500793984853, -6.376774720514417183, 20.66439772633092176 ) ) ;
#36734 = CARTESIAN_POINT ( 'NONE',  ( -16.40380107638378604, 14.33077157581830008, -1.500000000000002220 ) ) ;
#36735 = CARTESIAN_POINT ( 'NONE',  ( -71.33541886227440898, -25.24674103807599934, 5.089068620786424191 ) ) ;
#36737 = ORIENTED_EDGE ( 'NONE', *, *, #8683, .T. ) ;
#36736 = CARTESIAN_POINT ( 'NONE',  ( 4.546662993595487201, 21.82331882591909178, 11.49999999999999645 ) ) ;
#36738 = CARTESIAN_POINT ( 'NONE',  ( -53.62287095715005592, -24.64965695001467694, 8.947790433994185832 ) ) ;
#36739 = CARTESIAN_POINT ( 'NONE',  ( -92.58953762381672448, -23.47596703998600631, 11.44779298504227683 ) ) ;
#36740 = ADVANCED_FACE ( 'NONE', ( #5269 ), #79768, .F. ) ;
#36741 = DIRECTION ( 'NONE',  ( 0.000000000000000000, -0.9999999999976377785, -2.173523156925979975E-06 ) ) ;
#36742 = ORIENTED_EDGE ( 'NONE', *, *, #29307, .F. ) ;
#36743 = AXIS2_PLACEMENT_3D ( 'NONE', #36388, #67351, #98269 ) ;
#36744 = EDGE_LOOP ( 'NONE', ( #30571, #29474, #40239, #11122 ) ) ;
#36745 = EDGE_CURVE ( 'NONE', #100069, #41697, #35232, .T. ) ;
#36746 = ORIENTED_EDGE ( 'NONE', *, *, #97076, .T. ) ;
#36747 = CARTESIAN_POINT ( 'NONE',  ( -100.9686692281476610, -25.15033489556367741, 7.001233543541374615 ) ) ;
#36748 = CARTESIAN_POINT ( 'NONE',  ( -7.160000000000000142, -7.572993419422048511, 8.500388862211309515 ) ) ;
#36749 = CARTESIAN_POINT ( 'NONE',  ( 29.77147767949870882, -5.356774720514427379, 26.15915692125050995 ) ) ;
#36750 = EDGE_CURVE ( 'NONE', #47172, #50535, #19994, .T. ) ;
#36751 = DIRECTION ( 'NONE',  ( -3.773278334453079618E-23, 0.9999999999976377785, 2.173523156925979975E-06 ) ) ;
#36752 = CIRCLE ( 'NONE', #80493, 0.3000000000000016542 ) ;
#36753 = CARTESIAN_POINT ( 'NONE',  ( -9.862393454161701101, 16.67994275214481092, 11.49999999999998934 ) ) ;
#36754 = LINE ( 'NONE', #66733, #29571 ) ;
#36755 = ORIENTED_EDGE ( 'NONE', *, *, #63672, .F. ) ;
#36756 = AXIS2_PLACEMENT_3D ( 'NONE', #20478, #29092, #43831 ) ;
#36757 = CARTESIAN_POINT ( 'NONE',  ( -0.1161231997828221785, -19.40653004597026410, 11.49999999999999645 ) ) ;
#36758 = CARTESIAN_POINT ( 'NONE',  ( -2.899999999999996803, 33.29999999999999716, 2.100000000000000089 ) ) ;
#36759 = AXIS2_PLACEMENT_3D ( 'NONE', #2300, #34739, #88029 ) ;
#36760 = EDGE_LOOP ( 'NONE', ( #69798, #40226, #43677, #17818 ) ) ;
#36761 = CARTESIAN_POINT ( 'NONE',  ( 3.749014282529493869, -5.876774720514404748, 18.52125941707705792 ) ) ;
#36762 = CARTESIAN_POINT ( 'NONE',  ( 3.714584954927674154, -6.376774720514402972, 18.16171433633635246 ) ) ;
#36763 = DIRECTION ( 'NONE',  ( 0.000000000000000000, 0.000000000000000000, 1.000000000000000000 ) ) ;
#36764 = AXIS2_PLACEMENT_3D ( 'NONE', #86792, #78165, #25900 ) ;
#36766 = ADVANCED_FACE ( 'NONE', ( #81900 ), #33603, .T. ) ;
#36765 = DIRECTION ( 'NONE',  ( -0.000000000000000000, -0.000000000000000000, -1.000000000000000000 ) ) ;
#36767 = CARTESIAN_POINT ( 'NONE',  ( 13.00645856128228495, 14.71372164842801844, 11.49999999999998934 ) ) ;
#36768 = DIRECTION ( 'NONE',  ( 0.000000000000000000, -0.9999999999976377785, -2.173523156925979975E-06 ) ) ;
#36769 = VERTEX_POINT ( 'NONE', #68172 ) ;
#36770 = CARTESIAN_POINT ( 'NONE',  ( -13.10987527212420645, -17.12674121770768920, 11.49999999999998934 ) ) ;
#36771 = FACE_OUTER_BOUND ( 'NONE', #174, .T. ) ;
#36772 = PLANE ( 'NONE',  #52973 ) ;
#36773 = CARTESIAN_POINT ( 'NONE',  ( -114.6228709571500559, -29.50250243563736774, 8.947779886222136270 ) ) ;
#36774 = EDGE_CURVE ( 'NONE', #16634, #46870, #44346, .T. ) ;
#36775 = LINE ( 'NONE', #67739, #9925 ) ;
#36776 = CARTESIAN_POINT ( 'NONE',  ( -21.48638390452810043, -8.140844714011898020, -1.500000000000002220 ) ) ;
#36777 = CALENDAR_DATE ( 2026, 9, 10 ) ;
#36778 = CARTESIAN_POINT ( 'NONE',  ( -89.40841769935769889, -25.27880950044345809, 5.947789066509453271 ) ) ;
#36779 = DIRECTION ( 'NONE',  ( -3.773278334453079618E-23, 0.9999999999976377785, 2.173523156925979975E-06 ) ) ;
#36780 = CARTESIAN_POINT ( 'NONE',  ( 1.109688723463823301, -20.12803150795971874, 11.49999999999999645 ) ) ;
#36781 = CARTESIAN_POINT ( 'NONE',  ( -45.62287095715005592, -23.84081130438200091, 10.88220057463249013 ) ) ;
#36782 = DIRECTION ( 'NONE',  ( 0.000000000000000000, -0.9999999999976377785, -2.173523156925979128E-06 ) ) ;
#36783 = FACE_OUTER_BOUND ( 'NONE', #37547, .T. ) ;
#36784 = CARTESIAN_POINT ( 'NONE',  ( -29.52287095715006160, -23.40102634903646717, 11.44779303447556629 ) ) ;
#36785 = CARTESIAN_POINT ( 'NONE',  ( -110.9796143976588070, -25.29779200634336078, 3.502226275253062848 ) ) ;
#36786 = EDGE_CURVE ( 'NONE', #16750, #79871, #49819, .T. ) ;
#36787 = CARTESIAN_POINT ( 'NONE',  ( -1.769646468872753120, 19.80360307839763934, -1.500000000000002220 ) ) ;
#36788 = CARTESIAN_POINT ( 'NONE',  ( -47.52287095715004739, -24.66019654487199375, 8.947790411086122830 ) ) ;
#36789 = CARTESIAN_POINT ( 'NONE',  ( -0.9724026449420489771, -19.73431249065222204, -1.500000000000002220 ) ) ;
#36790 = CIRCLE ( 'NONE', #48169, 1.020000000000000018 ) ;
#36791 = CARTESIAN_POINT ( 'NONE',  ( -42.52916115802615593, -24.65952944569304606, 1.056160979905694353 ) ) ;
#36792 = B_SPLINE_CURVE_WITH_KNOTS ( 'NONE', 3,
 ( #70946, #69438, #62335, #47610, #54725, #927 ),
 .UNSPECIFIED., .F., .F.,
 ( 4, 2, 4 ),
 ( 0.000000000000000000, 0.001380901958385389412, 0.002761803916770778824 ),
 .UNSPECIFIED. ) ;
#36793 = CARTESIAN_POINT ( 'NONE',  ( -73.52287095715007581, -23.47596703998600631, 11.44779298504228748 ) ) ;
#36794 = CARTESIAN_POINT ( 'NONE',  ( -10.34999999999997833, 27.69999999999999929, 2.100000000000000089 ) ) ;
#36795 = CARTESIAN_POINT ( 'NONE',  ( 20.27745880512110688, -4.159726151199424571, 11.49999999999999645 ) ) ;
#36796 = AXIS2_PLACEMENT_3D ( 'NONE', #28636, #50480, #28142 ) ;
#36797 = CARTESIAN_POINT ( 'NONE',  ( -111.5562042904833788, -24.64965694238575367, 8.947790433994185832 ) ) ;
#36798 = LINE ( 'NONE', #12944, #43222 ) ;
#36799 = CARTESIAN_POINT ( 'NONE',  ( -50.15966858932511485, -25.31439280820845283, 5.214258294773329361 ) ) ;
#36800 = CARTESIAN_POINT ( 'NONE',  ( 18.72737137862276313, -12.84423604280260278, 11.49999999999999645 ) ) ;
#36801 = VERTEX_POINT ( 'NONE', #29099 ) ;
#36802 = B_SPLINE_SURFACE_WITH_KNOTS ( 'NONE', 3, 3, ( 
 ( #85423, #8307, #15908, #46875 ),
 ( #77795, #39250, #70210, #31636 ),
 ( #62607, #15408, #46369, #7296 ),
 ( #78304, #93528, #8812, #77302 ),
 ( #24022, #69207, #16405, #39748 ),
 ( #70708, #32137, #94540, #7803 ),
 ( #84427, #45879, #100122, #1206 ) ),
 .UNSPECIFIED., .F., .F., .F.,
 ( 4, 3, 4 ),
 ( 4, 4 ),
 ( 0.7945040050992232539, 0.8970133687736495665, 0.9995227324480758790 ),
 ( 0.3695879146558129213, 0.3707712655177336503 ),
 .UNSPECIFIED. ) ;
#36803 = CARTESIAN_POINT ( 'NONE',  ( -0.08860454909227881426, -5.876774720514410077, 19.21747685089457036 ) ) ;
#36804 = CARTESIAN_POINT ( 'NONE',  ( 29.70397367894831930, 3.853389802531868469, 28.15179473738050220 ) ) ;
#36805 = CARTESIAN_POINT ( 'NONE',  ( -20.16912494768211417, -0.3064379698199363733, 11.49999999999998934 ) ) ;
#36806 = CARTESIAN_POINT ( 'NONE',  ( -63.54869588136745051, -24.15543982623906416, -0.2315651400026651485 ) ) ;
#36807 = DIRECTION ( 'NONE',  ( 0.000000000000000000, 0.000000000000000000, -1.000000000000000000 ) ) ;
#36808 = ORIENTED_EDGE ( 'NONE', *, *, #86089, .T. ) ;
#36809 = AXIS2_PLACEMENT_3D ( 'NONE', #40625, #2566, #48238 ) ;
#36810 = ORIENTED_EDGE ( 'NONE', *, *, #84278, .T. ) ;
#36811 = DIRECTION ( 'NONE',  ( 1.000000000000000000, -0.000000000000000000, -0.000000000000000000 ) ) ;
#36812 = CARTESIAN_POINT ( 'NONE',  ( 20.41593879258296695, -10.28030303932802880, 11.49999999999998934 ) ) ;
#36813 = CARTESIAN_POINT ( 'NONE',  ( -74.62287095715005592, -23.48783264082478794, -1.443836473390067265 ) ) ;
#36814 = B_SPLINE_CURVE_WITH_KNOTS ( 'NONE', 3,
 ( #426, #77539, #39993, #31378, #62342, #38496 ),
 .UNSPECIFIED., .F., .F.,
 ( 4, 2, 4 ),
 ( 6.391158118977072634E-06, 0.001387004593080798072, 0.002767618028042619343 ),
 .UNSPECIFIED. ) ;
#36815 = CARTESIAN_POINT ( 'NONE',  ( -10.34410514300256523, -18.92461576200269491, -1.500000000000002220 ) ) ;
#36816 = CARTESIAN_POINT ( 'NONE',  ( -123.5911763806425796, -23.73766607897670866, -1.055555164236449350 ) ) ;
#36817 = DIRECTION ( 'NONE',  ( -3.773278334444167608E-23, 1.000000000000000000, 0.000000000000000000 ) ) ;
#36818 = CARTESIAN_POINT ( 'NONE',  ( 21.27769986149581172, 7.469961712261545372, 11.49999999999999645 ) ) ;
#36819 = ORIENTED_EDGE ( 'NONE', *, *, #91036, .F. ) ;
#36820 = CARTESIAN_POINT ( 'NONE',  ( -69.87926231432713564, -25.31612431666963303, 4.903252905761131153 ) ) ;
#36821 = CARTESIAN_POINT ( 'NONE',  ( 19.14557405504459453, -10.84957060938160289, -1.500000000000002220 ) ) ;
#36822 = LINE ( 'NONE', #92584, #78665 ) ;
#36823 = CARTESIAN_POINT ( 'NONE',  ( -41.32330479122543210, -25.29087095761961379, 3.114706565199032440 ) ) ;
#36824 = ORIENTED_EDGE ( 'NONE', *, *, #31089, .T. ) ;
#36825 = CARTESIAN_POINT ( 'NONE',  ( -19.80875734969026425, 5.965225279485572685, 31.02402280011862246 ) ) ;
#36826 = ADVANCED_FACE ( 'NONE', ( #52450 ), #76705, .T. ) ;
#36827 = FACE_OUTER_BOUND ( 'NONE', #85111, .T. ) ;
#36828 = ORIENTED_EDGE ( 'NONE', *, *, #95508, .F. ) ;
#36829 = CARTESIAN_POINT ( 'NONE',  ( -77.62287095715005592, -24.50216790748097040, 0.6166512839513687005 ) ) ;
#36830 = EDGE_CURVE ( 'NONE', #63682, #17879, #30383, .T. ) ;
#36831 = ORIENTED_EDGE ( 'NONE', *, *, #77076, .T. ) ;
#36832 = CIRCLE ( 'NONE', #62780, 20.00000000000000000 ) ;
#36833 = EDGE_CURVE ( 'NONE', #33400, #11110, #58262, .T. ) ;
#36834 = B_SPLINE_CURVE_WITH_KNOTS ( 'NONE', 3,
 ( #19923, #4712, #44277, #81335 ),
 .UNSPECIFIED., .F., .F.,
 ( 4, 4 ),
 ( 0.5391559877274726409, 0.5401567347682382225 ),
 .UNSPECIFIED. ) ;
#36835 = ORIENTED_EDGE ( 'NONE', *, *, #33461, .F. ) ;
#36836 = CARTESIAN_POINT ( 'NONE',  ( -81.52287095715010423, -23.48783264083388289, -1.443836473375922580 ) ) ;
#36837 = FACE_OUTER_BOUND ( 'NONE', #86514, .T. ) ;
#36838 = CARTESIAN_POINT ( 'NONE',  ( -104.5221999606295924, -23.48786465467241413, 11.44779295918254469 ) ) ;
#36839 = CARTESIAN_POINT ( 'NONE',  ( 15.56926775127050000, -13.18612581554039132, -1.500000000000002220 ) ) ;
#36840 = EDGE_CURVE ( 'NONE', #90955, #76106, #54657, .T. ) ;
#36841 = ORIENTED_EDGE ( 'NONE', *, *, #40849, .F. ) ;
#36842 = CARTESIAN_POINT ( 'NONE',  ( -3.071531057816138333, -6.376774720514413630, 19.86545874326175110 ) ) ;
#36843 = DIRECTION ( 'NONE',  ( -0.000000000000000000, -1.000000000000000000, -0.000000000000000000 ) ) ;
#36844 = EDGE_CURVE ( 'NONE', #27379, #32345, #41364, .T. ) ;
#36845 = DIRECTION ( 'NONE',  ( 0.5543250044962501066, 0.000000000000000000, -0.8323003000060928969 ) ) ;
#36846 = DIRECTION ( 'NONE',  ( 0.000000000000000000, 0.000000000000000000, 1.000000000000000000 ) ) ;
#36847 = ORIENTED_EDGE ( 'NONE', *, *, #43126, .T. ) ;
#36848 = CARTESIAN_POINT ( 'NONE',  ( -100.2228709571500644, -23.47596703998600631, 11.44779298504227860 ) ) ;
#36849 = CARTESIAN_POINT ( 'NONE',  ( -97.52287095715003318, -24.66019654487200441, 8.947790411086119278 ) ) ;
#36850 = CARTESIAN_POINT ( 'NONE',  ( 16.81283763619640936, 12.23492182941471107, -1.500000000000002220 ) ) ;
#36851 = ORIENTED_EDGE ( 'NONE', *, *, #36612, .T. ) ;
#36853 = ORIENTED_EDGE ( 'NONE', *, *, #23039, .T. ) ;
#36852 = CARTESIAN_POINT ( 'NONE',  ( -54.62287095715005592, -24.64898659630528854, 1.056161002820821038 ) ) ;
#36854 = CARTESIAN_POINT ( 'NONE',  ( 29.73860345376319003, -5.356471260711259674, 19.84760796525321425 ) ) ;
#36855 = ORIENTED_EDGE ( 'NONE', *, *, #23308, .T. ) ;
#36856 = ORIENTED_EDGE ( 'NONE', *, *, #18741, .T. ) ;
#36857 = CARTESIAN_POINT ( 'NONE',  ( -73.62287095715005592, -29.50250243563736774, 8.947779886222143375 ) ) ;
#36858 = CARTESIAN_POINT ( 'NONE',  ( -116.4728709571500360, -25.30558663486635140, 5.000950659935019971 ) ) ;
#36859 = CARTESIAN_POINT ( 'NONE',  ( -86.52287095715006160, -23.47593901973090169, -1.443836447538996648 ) ) ;
#36860 = DIRECTION ( 'NONE',  ( -1.000000000000000000, -0.000000000000000000, -0.000000000000000000 ) ) ;
#36862 = ORIENTED_EDGE ( 'NONE', *, *, #21702, .F. ) ;
#36861 = CARTESIAN_POINT ( 'NONE',  ( 15.99899278244174639, -15.33069297701436184, 11.49999999999999645 ) ) ;
#36863 = CARTESIAN_POINT ( 'NONE',  ( -108.5519315939779830, -24.34968618360934656, 0.1864209137778971292 ) ) ;
#36864 = CARTESIAN_POINT ( 'NONE',  ( -14.08738070862771963, 17.71811851510361535, -1.500000000000002220 ) ) ;
#36865 = VECTOR ( 'NONE', #41865, 1000.000000000000114 ) ;
#36867 = ORIENTED_EDGE ( 'NONE', *, *, #55309, .T. ) ;
#36866 = PLANE ( 'NONE',  #34430 ) ;
#36868 = ORIENTED_EDGE ( 'NONE', *, *, #56423, .F. ) ;
#36869 = VECTOR ( 'NONE', #6308, 1000.000000000000000 ) ;
#36870 = CARTESIAN_POINT ( 'NONE',  ( -10.17728017005432228, -5.183720752832764234, 29.88674535377839803 ) ) ;
#36871 = CARTESIAN_POINT ( 'NONE',  ( -15.22981678846565856, -13.14137338692033907, 11.49999999999998934 ) ) ;
#36872 = CARTESIAN_POINT ( 'NONE',  ( -0.1490770655183801252, -21.12008023607309681, -1.443836447538997758 ) ) ;
#36873 = ORIENTED_EDGE ( 'NONE', *, *, #73705, .T. ) ;
#36874 = DIRECTION ( 'NONE',  ( 0.000000000000000000, 0.000000000000000000, -1.000000000000000000 ) ) ;
#36875 = CARTESIAN_POINT ( 'NONE',  ( 4.546662993595487201, 21.82331882591909178, -1.500000000000002220 ) ) ;
#36876 = ORIENTED_EDGE ( 'NONE', *, *, #73065, .F. ) ;
#36877 = CARTESIAN_POINT ( 'NONE',  ( -73.62287095715007013, -23.47596703998600276, 11.44779298504227860 ) ) ;
#36878 = PLANE ( 'NONE',  #89683 ) ;
#36879 = DIRECTION ( 'NONE',  ( 0.7071067811865515695, -0.7071067811865435759, 0.000000000000000000 ) ) ;
#36880 = B_SPLINE_CURVE_WITH_KNOTS ( 'NONE', 3,
 ( #44021, #59257, #97805, #18319, #40662, #18809, #88335, #33043 ),
 .UNSPECIFIED., .F., .F.,
 ( 4, 2, 2, 4 ),
 ( -0.001224873891641419356, -0.0002244903592271048094, 0.0007758931731872097375, 0.002776660238015834711 ),
 .UNSPECIFIED. ) ;
#36881 = FACE_OUTER_BOUND ( 'NONE', #69990, .T. ) ;
#36882 = CARTESIAN_POINT ( 'NONE',  ( 9.052818235119415746, 17.31195010612007223, -1.500000000000002220 ) ) ;
#36883 = CARTESIAN_POINT ( 'NONE',  ( -19.99255411920323056, 7.849732829375159149, 11.49999999999998934 ) ) ;
#36884 = CARTESIAN_POINT ( 'NONE',  ( -2.791950601096355733, -5.876774720514415407, 20.17732409774492552 ) ) ;
#36885 = CARTESIAN_POINT ( 'NONE',  ( -120.5228709571500616, -25.00158670708909625, 2.256160236439166411 ) ) ;
#36886 = CYLINDRICAL_SURFACE ( 'NONE', #20073, 1.500000000000001332 ) ;
#36887 = EDGE_CURVE ( 'NONE', #95068, #33918, #32094, .T. ) ;
#36888 = CARTESIAN_POINT ( 'NONE',  ( -9.359374538088376383, 20.77767741201286711, -1.500000000000002220 ) ) ;
#36889 = VECTOR ( 'NONE', #24835, 1000.000000000000000 ) ;
#36890 = EDGE_CURVE ( 'NONE', #34658, #19777, #63634, .T. ) ;
#36891 = DIRECTION ( 'NONE',  ( 0.000000000000000000, 0.000000000000000000, 1.000000000000000000 ) ) ;
#36892 = CARTESIAN_POINT ( 'NONE',  ( -96.54754425073249990, -24.51419770103159834, 9.386484678747169852 ) ) ;
#36893 = DIRECTION ( 'NONE',  ( -1.000000000000000000, -0.000000000000000000, -0.000000000000000000 ) ) ;
#36894 = CARTESIAN_POINT ( 'NONE',  ( -19.95764006394758638, 0.7380318605572177004, 11.49999999999999645 ) ) ;
#36895 = DIRECTION ( 'NONE',  ( -1.000000000000000000, -0.000000000000000000, -0.000000000000000000 ) ) ;
#36896 = VECTOR ( 'NONE', #3079, 1000.000000000000000 ) ;
#36897 = DIRECTION ( 'NONE',  ( 0.000000000000000000, 0.000000000000000000, 1.000000000000000000 ) ) ;
#36898 = CARTESIAN_POINT ( 'NONE',  ( -44.22287095715006444, -23.47593901973090169, -1.443836447538997980 ) ) ;
#36899 = ORIENTED_EDGE ( 'NONE', *, *, #94131, .T. ) ;
#36900 = CARTESIAN_POINT ( 'NONE',  ( -89.58953762381671027, -24.64898659630529210, 1.056161002820829031 ) ) ;
#36901 = CARTESIAN_POINT ( 'NONE',  ( -124.5228709571500900, -23.48783264082477373, -1.443836473390085029 ) ) ;
#36902 = CARTESIAN_POINT ( 'NONE',  ( 7.827691340095081607, 20.28360254610759839, -1.500000000000002220 ) ) ;
#36903 = CARTESIAN_POINT ( 'NONE',  ( -40.62287095715005592, -29.50247984919015209, -1.443849546365060466 ) ) ;
#36904 = CARTESIAN_POINT ( 'NONE',  ( -18.74126595726828626, 5.813943427813767606, -1.500000000000002220 ) ) ;
#36905 = DIRECTION ( 'NONE',  ( 1.000000000000000000, 3.773278334444166432E-23, 8.201307841325785021E-29 ) ) ;
#36906 = VERTEX_POINT ( 'NONE', #1160 ) ;
#36907 = ITEM_DEFINED_TRANSFORMATION ( 'NONE', 'NONE', #5080,  #37391 ) ;
#36908 = FACE_OUTER_BOUND ( 'NONE', #74484, .T. ) ;
#36909 = DIRECTION ( 'NONE',  ( -3.773278334453079030E-23, 0.9999999999976377785, 2.173523156925979128E-06 ) ) ;
#36910 = CARTESIAN_POINT ( 'NONE',  ( -9.284664653622879626, 18.31210316397345395, 11.49999999999999645 ) ) ;
#36911 = CARTESIAN_POINT ( 'NONE',  ( -50.24370449261476779, -25.30394787829096970, 5.202377319005417000 ) ) ;
#36912 = DIRECTION ( 'NONE',  ( 0.000000000000000000, 0.9999999999976377785, 2.173523156925979128E-06 ) ) ;
#36913 = B_SPLINE_CURVE_WITH_KNOTS ( 'NONE', 3,
 ( #97664, #90057, #20529, #51504 ),
 .UNSPECIFIED., .F., .F.,
 ( 4, 4 ),
 ( 0.000000000000000000, 9.999999999998897304E-05 ),
 .UNSPECIFIED. ) ;
#36914 = ORIENTED_EDGE ( 'NONE', *, *, #67890, .F. ) ;
#36915 = LINE ( 'NONE', #5961, #79962 ) ;
#36916 = LINE ( 'NONE', #98809, #76928 ) ;
#36917 = PLANE ( 'NONE',  #32245 ) ;
#36918 = DIRECTION ( 'NONE',  ( 1.000000000000000000, 0.000000000000000000, 0.000000000000000000 ) ) ;
#36919 = ORIENTED_EDGE ( 'NONE', *, *, #68012, .F. ) ;
#36920 = CARTESIAN_POINT ( 'NONE',  ( -5.891025641025639636, -5.876774720514419847, 20.75510817307693046 ) ) ;
#36921 = EDGE_CURVE ( 'NONE', #79917, #88666, #35256, .T. ) ;
#36922 = CARTESIAN_POINT ( 'NONE',  ( 4.903590608199674072, 22.46510890469962263, 11.49999999999999645 ) ) ;
#36923 = CARTESIAN_POINT ( 'NONE',  ( 0.9741843557120299923, -22.74547949729550922, 11.49999999999998934 ) ) ;
#36924 = CARTESIAN_POINT ( 'NONE',  ( 3.094204744773375815, -6.376774720514422512, 21.02053020447315745 ) ) ;
#36925 = B_SPLINE_SURFACE_WITH_KNOTS ( 'NONE', 3, 3, ( 
 ( #1991, #94824, #70497, #982 ),
 ( #62903, #93828, #24314, #16698 ),
 ( #11581, #80598, #33933, #34431 ),
 ( #25818, #20187, #73488, #56788 ),
 ( #2995, #65906, #26815, #18205 ),
 ( #64912, #64411, #58279, #50657 ),
 ( #50164, #42559, #2490, #3986 ) ),
 .UNSPECIFIED., .F., .F., .F.,
 ( 4, 3, 4 ),
 ( 4, 4 ),
 ( 0.0004766839783820627473, 0.1029713700210898447, 0.2054660560637976141 ),
 ( 0.2095473025018212698, 0.2106567117982014459 ),
 .UNSPECIFIED. ) ;
#36926 = LINE ( 'NONE', #51664, #2641 ) ;
#36927 = CARTESIAN_POINT ( 'NONE',  ( -120.5228709571500616, -24.91570333825770689, 8.075032458260345436 ) ) ;
#36928 = DIRECTION ( 'NONE',  ( -7.960204194457801640E-17, -1.000000000000000000, 0.000000000000000000 ) ) ;
#36929 = CARTESIAN_POINT ( 'NONE',  ( -8.160000000000000142, 2.939152317953647106E-16, -2.399999999999999911 ) ) ;
#36930 = CARTESIAN_POINT ( 'NONE',  ( 13.84421170697429737, -16.98027460053469895, -1.500000000000002220 ) ) ;
#36931 = CARTESIAN_POINT ( 'NONE',  ( 7.480769230769231726, -5.876774720514430506, 20.77403846153845635 ) ) ;
#36932 = CARTESIAN_POINT ( 'NONE',  ( -87.59864960828673475, -23.73791477778911840, 11.05961554403170588 ) ) ;
#36933 = CARTESIAN_POINT ( 'NONE',  ( -41.22828023510016493, -25.31356029329619517, 4.766479152052003343 ) ) ;
#36934 = DIRECTION ( 'NONE',  ( -1.000000000000000000, 0.000000000000000000, 0.000000000000000000 ) ) ;
#36935 = DIRECTION ( 'NONE',  ( 1.000000000000000000, 3.773278334444166432E-23, 8.201307841325785021E-29 ) ) ;
#36936 = DIRECTION ( 'NONE',  ( -3.773278334453080206E-23, 0.9999999999976377785, 2.173523156925979975E-06 ) ) ;
#36937 = ORIENTED_EDGE ( 'NONE', *, *, #40173, .F. ) ;
#36938 = ADVANCED_FACE ( 'NONE', ( #2173, #31093 ), #62562, .T. ) ;
#36939 = CARTESIAN_POINT ( 'NONE',  ( -2.750569593922542300, -20.27526743851804625, -1.500000000000002220 ) ) ;
#36940 = ORIENTED_EDGE ( 'NONE', *, *, #72008, .T. ) ;
#36941 = VERTEX_POINT ( 'NONE', #93487 ) ;
#36942 = ORIENTED_EDGE ( 'NONE', *, *, #89211, .F. ) ;
#36943 = ORIENTED_EDGE ( 'NONE', *, *, #862, .T. ) ;
#36944 = CARTESIAN_POINT ( 'NONE',  ( 22.92345266703080142, -2.467471440992916154, 11.49999999999998934 ) ) ;
#36945 = DIRECTION ( 'NONE',  ( -0.000000000000000000, 0.9513357669802769978, -0.3081562241202474572 ) ) ;
#36946 = CARTESIAN_POINT ( 'NONE',  ( -9.609455416251792670, -17.83980533922896683, -1.500000000000002220 ) ) ;
#36947 = EDGE_CURVE ( 'NONE', #23691, #4955, #16872, .T. ) ;
#36948 = ORIENTED_EDGE ( 'NONE', *, *, #77591, .F. ) ;
#36949 = CARTESIAN_POINT ( 'NONE',  ( -26.07746707516802331, -24.95785182683525605, 4.938174481708933250 ) ) ;
#36950 = VECTOR ( 'NONE', #66862, 1000.000000000000000 ) ;
#36951 = CARTESIAN_POINT ( 'NONE',  ( -37.62287095715005592, -29.50247984919015209, -1.443849546365060466 ) ) ;
#36952 = EDGE_CURVE ( 'NONE', #50678, #100104, #32603, .T. ) ;
#36953 = CARTESIAN_POINT ( 'NONE',  ( -25.92875734969026524, 6.376774720514426953, -0.08597719988137648983 ) ) ;
#36954 = CARTESIAN_POINT ( 'NONE',  ( -70.61332773891285797, -23.48783264082477018, -1.443836473390095021 ) ) ;
#36956 = ORIENTED_EDGE ( 'NONE', *, *, #21904, .T. ) ;
#36955 = CARTESIAN_POINT ( 'NONE',  ( -9.924231251898440576, -18.97836718215353713, 11.49999999999999645 ) ) ;
#36957 = CARTESIAN_POINT ( 'NONE',  ( -104.6228709571500559, -29.50250243563736774, 8.947779886222138046 ) ) ;
#36958 = CARTESIAN_POINT ( 'NONE',  ( -41.66425029149441173, -23.48783264082477729, -1.443836473390075925 ) ) ;
#36959 = ADVANCED_FACE ( 'NONE', ( #648 ), #85379, .F. ) ;
#36960 = ORIENTED_EDGE ( 'NONE', *, *, #27057, .T. ) ;
#36961 = EDGE_CURVE ( 'NONE', #90802, #67691, #63111, .T. ) ;
#36962 = CARTESIAN_POINT ( 'NONE',  ( -20.55201672899488585, 2.666056886502145673, 11.49999999999998934 ) ) ;
#36963 = CIRCLE ( 'NONE', #17550, 3.349999999999998757 ) ;
#36964 = ORIENTED_EDGE ( 'NONE', *, *, #94859, .T. ) ;
#36965 = FACE_OUTER_BOUND ( 'NONE', #67725, .T. ) ;
#36966 = ORIENTED_EDGE ( 'NONE', *, *, #22200, .T. ) ;
#36967 = CARTESIAN_POINT ( 'NONE',  ( -55.52287095715006160, -24.62285846331433703, 9.038163153548362416 ) ) ;
#36968 = AXIS2_PLACEMENT_3D ( 'NONE', #38321, #77870, #70781 ) ;
#36969 = ORIENTED_EDGE ( 'NONE', *, *, #68630, .F. ) ;
#36970 = CARTESIAN_POINT ( 'NONE',  ( -11.62490142266122639, -17.50836435561060256, -1.500000000000002220 ) ) ;
#36971 = EDGE_CURVE ( 'NONE', #89124, #21600, #85889, .T. ) ;
#36972 = CARTESIAN_POINT ( 'NONE',  ( 21.10488023177059347, -6.046698511884514460, 11.49999999999999645 ) ) ;
#36973 = CARTESIAN_POINT ( 'NONE',  ( -73.52211514783047619, -23.48786465467241058, 11.44779295918254824 ) ) ;
#36974 = CARTESIAN_POINT ( 'NONE',  ( 16.93931825803137414, 14.88162037096512158, -1.500000000000002220 ) ) ;
#36975 = B_SPLINE_CURVE_WITH_KNOTS ( 'NONE', 3,
 ( #3911, #81021, #82016, #88140 ),
 .UNSPECIFIED., .F., .F.,
 ( 4, 4 ),
 ( 0.000000000000000000, 1.000000000000000000 ),
 .UNSPECIFIED. ) ;
#36976 = CARTESIAN_POINT ( 'NONE',  ( -20.39251343623233836, 4.912230638944180328, 11.49999999999998934 ) ) ;
#36977 = DIRECTION ( 'NONE',  ( 1.000000000000000000, 3.773278334444166432E-23, 8.201307841325785021E-29 ) ) ;
#36978 = DIRECTION ( 'NONE',  ( 1.000000000000000000, 4.015979463811607402E-15, 0.000000000000000000 ) ) ;
#36979 = DIRECTION ( 'NONE',  ( 0.000000000000000000, 2.173523156925980399E-06, -0.9999999999976378895 ) ) ;
#36980 = VERTEX_POINT ( 'NONE', #1664 ) ;
#36981 = AXIS2_PLACEMENT_3D ( 'NONE', #83201, #4103, #43170 ) ;
#36982 = EDGE_LOOP ( 'NONE', ( #28141, #973, #19186, #74412 ) ) ;
#36983 = ORIENTED_EDGE ( 'NONE', *, *, #33976, .T. ) ;
#36984 = CARTESIAN_POINT ( 'NONE',  ( -66.52209609814681812, -23.48783264082476308, -1.443836473390097463 ) ) ;
#36985 = CARTESIAN_POINT ( 'NONE',  ( -10.32266838563235467, 18.89866041204108527, -1.500000000000002220 ) ) ;
#36986 = DIRECTION ( 'NONE',  ( 0.000000000000000000, 0.9999999999976377785, 2.173523156925979128E-06 ) ) ;
#36987 = EDGE_LOOP ( 'NONE', ( #39220, #61693, #2466, #61674 ) ) ;
#36988 = CARTESIAN_POINT ( 'NONE',  ( -20.79277273739468512, 3.736189789763188607, 11.49999999999998934 ) ) ;
#36989 = DIRECTION ( 'NONE',  ( 0.000000000000000000, -1.000000000000000000, 0.000000000000000000 ) ) ;
#36990 = FACE_OUTER_BOUND ( 'NONE', #41613, .T. ) ;
#36991 = CARTESIAN_POINT ( 'NONE',  ( -100.5228709571500758, -24.92579138211019441, 1.929029949965663127 ) ) ;
#36992 = CARTESIAN_POINT ( 'NONE',  ( 11.41483471809167405, -6.475225279485574248, -27.05170832580397189 ) ) ;
#36993 = CARTESIAN_POINT ( 'NONE',  ( -123.5562042904834072, -23.48783264082478794, -1.443836473390058384 ) ) ;
#36994 = CARTESIAN_POINT ( 'NONE',  ( -9.153499762860807465, 20.15527781828815534, -1.500000000000002220 ) ) ;
#36995 = CARTESIAN_POINT ( 'NONE',  ( -30.47287095715008576, -23.47593902499770380, -1.441415665115638456 ) ) ;
#36996 = ADVANCED_FACE ( 'NONE', ( #24981 ), #55956, .T. ) ;
#36997 = ORIENTED_EDGE ( 'NONE', *, *, #11451, .T. ) ;
#36998 = DIRECTION ( 'NONE',  ( 1.000000000000000000, -0.000000000000000000, 0.000000000000000000 ) ) ;
#36999 = CARTESIAN_POINT ( 'NONE',  ( -79.62287095715008434, -23.94994826722565762, -0.6494450866342735829 ) ) ;
#37000 = CARTESIAN_POINT ( 'NONE',  ( -41.86878170341644534, -25.27955791706579092, 4.256748853647015274 ) ) ;
#37001 = ADVANCED_FACE ( 'NONE', ( #81280 ), #95503, .F. ) ;
#37002 = CARTESIAN_POINT ( 'NONE',  ( -97.52287095715006160, -24.64965694238575011, 8.947790433994194714 ) ) ;
#37003 = B_SPLINE_CURVE_WITH_KNOTS ( 'NONE', 3,
 ( #75134, #99461, #37580, #29455 ),
 .UNSPECIFIED., .F., .F.,
 ( 4, 4 ),
 ( 0.7510362966358483661, 0.7600427279079640108 ),
 .UNSPECIFIED. ) ;
#37004 = CARTESIAN_POINT ( 'NONE',  ( -13.34961138979462270, 14.11212085816309880, -1.500000000000002220 ) ) ;
#37005 = CARTESIAN_POINT ( 'NONE',  ( 18.99370601119529312, 9.851043883551550806, 11.49999999999998934 ) ) ;
#37006 = CARTESIAN_POINT ( 'NONE',  ( -69.22054176954050320, -25.14415006753612758, 7.039201735951476024 ) ) ;
#37007 = CARTESIAN_POINT ( 'NONE',  ( -81.62287095715004170, -23.48786465467241058, 11.44779295918254647 ) ) ;
#37008 = EDGE_CURVE ( 'NONE', #64821, #52058, #94538, .T. ) ;
#37009 = CARTESIAN_POINT ( 'NONE',  ( -106.5895376238167245, -24.65952944569304961, 1.056160979905703678 ) ) ;
#37010 = CARTESIAN_POINT ( 'NONE',  ( -2.499999999999993339, 19.99999999999999645, 0.000000000000000000 ) ) ;
#37011 = CARTESIAN_POINT ( 'NONE',  ( 18.27610663105864219, 13.37729726205769154, -1.500000000000002220 ) ) ;
#37012 = B_SPLINE_SURFACE_WITH_KNOTS ( 'NONE', 3, 1, ( 
 ( #44130, #84175 ),
 ( #77056, #23266 ),
 ( #48134, #39005 ),
 ( #443, #79062 ),
 ( #32399, #9555 ),
 ( #93790, #93283 ),
 ( #31396, #78552 ),
 ( #23775, #46635 ),
 ( #54750, #24286 ),
 ( #15666, #8056 ),
 ( #86681, #1459 ),
 ( #62357, #69958 ),
 ( #15163, #16665 ),
 ( #85685, #16165 ),
 ( #47636, #69458 ) ),
 .UNSPECIFIED., .F., .F., .F.,
 ( 4, 1, 1, 1, 1, 1, 1, 1, 1, 1, 1, 1, 4 ),
 ( 2, 2 ),
 ( 0.000000000000000000, 0.1227119423657796193, 0.2396849640167788842, 0.3518158552560940455, 0.4637661328620885093, 0.5208177931608346523, 0.5794482914480051372, 0.6406041451203223769, 0.7052975118059877646, 0.7736338807131363238, 0.8446693818863779679, 0.9200565080211464686, 1.000000000000000000 ),
 ( 0.000000000000000000, 1.000000000000000000 ),
 .UNSPECIFIED. ) ;
#37013 = EDGE_LOOP ( 'NONE', ( #76283, #22332, #71558, #76502, #4639, #97761, #76338, #95747, #86464, #23502 ) ) ;
#37014 = EDGE_CURVE ( 'NONE', #76617, #9739, #86019, .T. ) ;
#37015 = CARTESIAN_POINT ( 'NONE',  ( 4.373554412633047228, -5.876774720514422512, 21.19197260575996822 ) ) ;
#37016 = DIRECTION ( 'NONE',  ( 0.000000000000000000, -0.9999999999976377785, -2.173523156925979975E-06 ) ) ;
#37017 = CARTESIAN_POINT ( 'NONE',  ( 13.37688099249405127, 14.58279310912311111, 11.49999999999999645 ) ) ;
#37019 = B_SPLINE_CURVE_WITH_KNOTS ( 'NONE', 3,
 ( #74342, #36781, #91554, #98662, #68231, #75328, #91058, #99160 ),
 .UNSPECIFIED., .F., .F.,
 ( 4, 2, 2, 4 ),
 ( 0.000000000000000000, 0.002001079623178221925, 0.003001619434767334622, 0.004002159246356447320 ),
 .UNSPECIFIED. ) ;
#37018 = FACE_OUTER_BOUND ( 'NONE', #55060, .T. ) ;
#37020 = VERTEX_POINT ( 'NONE', #73669 ) ;
#37021 = CARTESIAN_POINT ( 'NONE',  ( -86.52287095715006160, -29.50248528299804818, 1.056150453629040253 ) ) ;
#37022 = DIRECTION ( 'NONE',  ( 0.000000000000000000, 0.000000000000000000, 1.000000000000000000 ) ) ;
#37023 = CARTESIAN_POINT ( 'NONE',  ( 7.043455336710909620, -20.48365140995157674, -1.500000000000002220 ) ) ;
#37024 = CARTESIAN_POINT ( 'NONE',  ( -26.61588051278965850, -24.82222928824689134, 7.072807463452274845 ) ) ;
#37025 = VECTOR ( 'NONE', #68109, 1000.000000000000000 ) ;
#37026 = CARTESIAN_POINT ( 'NONE',  ( -12.45040968399260883, -14.89389333286084671, -1.500000000000002220 ) ) ;
#37027 = CARTESIAN_POINT ( 'NONE',  ( -129.6228709571500701, -23.48786465467241769, 11.44779295918253581 ) ) ;
#37028 = CARTESIAN_POINT ( 'NONE',  ( -82.62287095715004170, -24.35013146730203815, 9.818937971375111928 ) ) ;
#37029 = CARTESIAN_POINT ( 'NONE',  ( 4.927431051831622000, -19.18327824014073357, 11.49999999999998934 ) ) ;
#37030 = EDGE_LOOP ( 'NONE', ( #97616, #24001, #52713, #25878 ) ) ;
#37031 = CARTESIAN_POINT ( 'NONE',  ( -18.18203184671642703, 9.085611141607108365, 11.49999999999999645 ) ) ;
#37032 = DIRECTION ( 'NONE',  ( -3.773278334453079618E-23, 0.9999999999976377785, 2.173523156925979975E-06 ) ) ;
#37033 = CC_DESIGN_PERSON_AND_ORGANIZATION_ASSIGNMENT ( #39140, #22399, ( #27178 ) ) ;
#37034 = B_SPLINE_CURVE_WITH_KNOTS ( 'NONE', 3,
 ( #88526, #59083, #82398, #81412 ),
 .UNSPECIFIED., .F., .F.,
 ( 4, 4 ),
 ( 0.000000000000000000, 0.0001000000000000028644 ),
 .UNSPECIFIED. ) ;
#37035 = CARTESIAN_POINT ( 'NONE',  ( 33.13630134430571417, -3.554473796596999691, -12.85738972836020899 ) ) ;
#37036 = ORIENTED_EDGE ( 'NONE', *, *, #39279, .T. ) ;
#37037 = FACE_OUTER_BOUND ( 'NONE', #51220, .T. ) ;
#37038 = CARTESIAN_POINT ( 'NONE',  ( 6.365284455128204399, -6.376774720514413630, 19.73076923076922640 ) ) ;
#37039 = VECTOR ( 'NONE', #83078, 1000.000000000000114 ) ;
#37040 = CARTESIAN_POINT ( 'NONE',  ( -82.58953762381672448, -23.48786465467241413, 11.44779295918254647 ) ) ;
#37041 = CARTESIAN_POINT ( 'NONE',  ( -49.62287095715004170, -23.47596703998600631, 11.44779298504227505 ) ) ;
#37042 = CARTESIAN_POINT ( 'NONE',  ( -4.751880754313710042, -19.48972053015312866, 11.49999999999998934 ) ) ;
#37043 = CARTESIAN_POINT ( 'NONE',  ( 282.9764569301858046, 1.682774720514426114, 20.79159422840526616 ) ) ;
#37044 = ORIENTED_EDGE ( 'NONE', *, *, #2474, .T. ) ;
#37045 = CARTESIAN_POINT ( 'NONE',  ( -3.108974358974355923, -5.876774720514426953, 21.75000000000001066 ) ) ;
#37046 = VECTOR ( 'NONE', #79721, 1000.000000000000114 ) ;
#37047 = CARTESIAN_POINT ( 'NONE',  ( 13.81544771398824345, -18.15223324129861382, 11.49999999999999645 ) ) ;
#37048 = CARTESIAN_POINT ( 'NONE',  ( -49.76261995625480949, -25.26258836565245502, 4.511523319824253697 ) ) ;
#37049 = CARTESIAN_POINT ( 'NONE',  ( -24.55517127435777169, -5.965225279485592225, -15.44180958690142802 ) ) ;
#37050 = DIRECTION ( 'NONE',  ( -1.000000000000000000, -0.000000000000000000, -0.000000000000000000 ) ) ;
#37051 = CARTESIAN_POINT ( 'NONE',  ( -43.62287095715004881, -24.64965695001467694, 8.947790433994187609 ) ) ;
#37052 = DIRECTION ( 'NONE',  ( 0.000000000000000000, -0.000000000000000000, 1.000000000000000000 ) ) ;
#37053 = DIRECTION ( 'NONE',  ( -3.773278334453079618E-23, 0.9999999999976377785, 2.173523156925979975E-06 ) ) ;
#37054 = ORIENTED_EDGE ( 'NONE', *, *, #85983, .F. ) ;
#37055 = CARTESIAN_POINT ( 'NONE',  ( 18.17922461840205983, -9.147185827878928421, -1.500000000000002220 ) ) ;
#37056 = ORIENTED_EDGE ( 'NONE', *, *, #86200, .T. ) ;
#37057 = EDGE_CURVE ( 'NONE', #42990, #70138, #72676, .T. ) ;
#37058 = CARTESIAN_POINT ( 'NONE',  ( -1.334576548209915225, -22.92891363262047832, -1.500000000000002220 ) ) ;
#37059 = CARTESIAN_POINT ( 'NONE',  ( -53.52287095715005449, -23.96177878511308634, 10.65340807706330217 ) ) ;
#37060 = EDGE_LOOP ( 'NONE', ( #44732, #84881, #72538 ) ) ;
#37061 = DIRECTION ( 'NONE',  ( -0.9978940991575084851, 0.000000000000000000, -0.06486421869277853025 ) ) ;
#37062 = B_SPLINE_CURVE_WITH_KNOTS ( 'NONE', 3,
 ( #66360, #42518, #20151, #73955 ),
 .UNSPECIFIED., .F., .F.,
 ( 4, 4 ),
 ( 0.000000000000000000, 0.0001000000000000028644 ),
 .UNSPECIFIED. ) ;
#37063 = FACE_OUTER_BOUND ( 'NONE', #49335, .T. ) ;
#37064 = B_SPLINE_CURVE_WITH_KNOTS ( 'NONE', 3,
 ( #83682, #6566, #92789, #37513 ),
 .UNSPECIFIED., .F., .F.,
 ( 4, 4 ),
 ( 0.000000000000000000, 0.0001000000000000722533 ),
 .UNSPECIFIED. ) ;
#37065 = FACE_OUTER_BOUND ( 'NONE', #8098, .T. ) ;
#37067 = ORIENTED_EDGE ( 'NONE', *, *, #23925, .F. ) ;
#37066 = CARTESIAN_POINT ( 'NONE',  ( -15.80959461918071618, 14.24510877297761446, 11.49999999999999645 ) ) ;
#37068 = ADVANCED_FACE ( 'NONE', ( #18380 ), #66087, .F. ) ;
#37069 = EDGE_LOOP ( 'NONE', ( #60220, #86389, #64328, #36443, #7169 ) ) ;
#37070 = CARTESIAN_POINT ( 'NONE',  ( 18.11909884760711975, -12.84011383348296853, -1.500000000000002220 ) ) ;
#37071 = EDGE_CURVE ( 'NONE', #60342, #31523, #49855, .T. ) ;
#37072 = CARTESIAN_POINT ( 'NONE',  ( -0.003042231299257275486, -20.61035990087709635, -1.500000000000002220 ) ) ;
#37073 = ORIENTED_EDGE ( 'NONE', *, *, #99459, .F. ) ;
#37074 = VERTEX_POINT ( 'NONE', #97500 ) ;
#37075 = FACE_OUTER_BOUND ( 'NONE', #61574, .T. ) ;
#37076 = CARTESIAN_POINT ( 'NONE',  ( -56.62287095715007013, -23.96127896941632685, -0.6493128931037894791 ) ) ;
#37077 = ORIENTED_EDGE ( 'NONE', *, *, #13390, .F. ) ;
#37078 = CIRCLE ( 'NONE', #32228, 3.500000000000000000 ) ;
#37079 = ORIENTED_EDGE ( 'NONE', *, *, #26099, .T. ) ;
#37080 = CARTESIAN_POINT ( 'NONE',  ( -125.7765849230966211, -25.21250125880508719, 3.500947807641615839 ) ) ;
#37081 = CARTESIAN_POINT ( 'NONE',  ( -41.58697324491572545, -24.35071581493542325, 9.817618358456032368 ) ) ;
#37082 = CARTESIAN_POINT ( 'NONE',  ( -99.62287095715005592, -29.50248528299804818, 1.056150453629042030 ) ) ;
#37083 = CARTESIAN_POINT ( 'NONE',  ( 0.5783248939474509021, 20.82821387695577187, -1.500000000000002220 ) ) ;
#37084 = ADVANCED_FACE ( 'NONE', ( #26997 ), #97002, .F. ) ;
#37085 = CARTESIAN_POINT ( 'NONE',  ( -16.40380107638378604, 14.33077157581830008, 11.49999999999999645 ) ) ;
#37086 = CARTESIAN_POINT ( 'NONE',  ( -51.88024557362344069, -25.20637680390643354, 6.555349849948861163 ) ) ;
#37087 = DIRECTION ( 'NONE',  ( 0.000000000000000000, 0.000000000000000000, 1.000000000000000000 ) ) ;
#37088 = CARTESIAN_POINT ( 'NONE',  ( -8.519796113377745783, 20.75715399588506926, 11.49999999999998934 ) ) ;
#37089 = AXIS2_PLACEMENT_3D ( 'NONE', #36957, #91240, #83626 ) ;
#37090 = DIRECTION ( 'NONE',  ( -0.000000000000000000, 1.000000000000000000, -0.000000000000000000 ) ) ;
#37091 = ORIENTED_EDGE ( 'NONE', *, *, #9801, .F. ) ;
#37092 = CARTESIAN_POINT ( 'NONE',  ( -71.50913726475666010, -25.30966908743296884, 5.397536596095833694 ) ) ;
#37093 = CARTESIAN_POINT ( 'NONE',  ( -66.52287095715006160, -29.50247984919015209, -1.443849546365055359 ) ) ;
#37094 = ORIENTED_EDGE ( 'NONE', *, *, #74433, .F. ) ;
#37095 = AXIS2_PLACEMENT_3D ( 'NONE', #60029, #5722, #4234 ) ;
#37096 = VERTEX_POINT ( 'NONE', #11266 ) ;
#37097 = CARTESIAN_POINT ( 'NONE',  ( -99.70017921987172826, -25.30826663797894227, 5.426235228613150774 ) ) ;
#37098 = VERTEX_POINT ( 'NONE', #51333 ) ;
#37099 = CARTESIAN_POINT ( 'NONE',  ( 1.764508054474889009, 21.21474994468914943, -1.500000000000002220 ) ) ;
#37100 = ORIENTED_EDGE ( 'NONE', *, *, #99069, .F. ) ;
#37101 = PLANE ( 'NONE',  #47917 ) ;
#37102 = CARTESIAN_POINT ( 'NONE',  ( -0.5131542516139314669, 21.03015271272555253, 11.49999999999998934 ) ) ;
#37103 = CARTESIAN_POINT ( 'NONE',  ( -38.52287095715006160, -24.50321055353803956, 9.387540953477520489 ) ) ;
#37104 = VECTOR ( 'NONE', #82842, 1000.000000000000000 ) ;
#37105 = B_SPLINE_CURVE_WITH_KNOTS ( 'NONE', 3,
 ( #41337, #64195, #85497, #86003, #40827, #25607 ),
 .UNSPECIFIED., .F., .F.,
 ( 4, 2, 4 ),
 ( 0.000000000000000000, 0.001380764517853250986, 0.002761529035706501971 ),
 .UNSPECIFIED. ) ;
#37106 = CARTESIAN_POINT ( 'NONE',  ( 15.01415361830768447, -3.567044333682400481, -27.41917996820976811 ) ) ;
#37107 = CARTESIAN_POINT ( 'NONE',  ( 5.996070682796505125, -3.316774720514426900, -27.41631156547456882 ) ) ;
#37108 = CARTESIAN_POINT ( 'NONE',  ( 5.197331492371871420, 21.31670716312865466, -1.500000000000002220 ) ) ;
#37109 = CARTESIAN_POINT ( 'NONE',  ( -87.59165601682460078, -24.15543982623908548, -0.2315651400026449980 ) ) ;
#37110 = ORIENTED_EDGE ( 'NONE', *, *, #41684, .T. ) ;
#37111 = CARTESIAN_POINT ( 'NONE',  ( -80.71590087609354214, -25.30702814991555982, 4.545935848987151751 ) ) ;
#37112 = EDGE_CURVE ( 'NONE', #57878, #89671, #53318, .T. ) ;
#37113 = ADVANCED_FACE ( 'NONE', ( #82275 ), #12750, .T. ) ;
#37114 = CARTESIAN_POINT ( 'NONE',  ( -84.62619856286293896, -24.51419770103157347, 9.386484678747175181 ) ) ;
#37115 = CARTESIAN_POINT ( 'NONE',  ( -130.5728709571500588, -24.66459861931856778, 1.095224832288515637 ) ) ;
#37116 = CARTESIAN_POINT ( 'NONE',  ( -30.62895736903226407, -24.04695220404052591, 10.47594215909544779 ) ) ;
#37117 = CARTESIAN_POINT ( 'NONE',  ( 20.49606604269246546, -5.804284187783010474, -1.500000000000002220 ) ) ;
#37118 = CARTESIAN_POINT ( 'NONE',  ( -98.54622777176759030, -24.66019654487200086, 8.947790411086115725 ) ) ;
#37119 = CARTESIAN_POINT ( 'NONE',  ( -27.96875734969026084, 6.475225279485573360, 26.43402280011862615 ) ) ;
#37120 = ADVANCED_FACE ( 'NONE', ( #81778 ), #98557, .T. ) ;
#37121 = DIRECTION ( 'NONE',  ( -3.773278334453079030E-23, 0.9999999999976377785, 2.173523156925979128E-06 ) ) ;
#37122 = CARTESIAN_POINT ( 'NONE',  ( -70.52287095715007581, -24.62226745350440282, 0.9660975649729651726 ) ) ;
#37123 = CARTESIAN_POINT ( 'NONE',  ( 20.43785579724129420, 9.289222182981756504, -1.500000000000002220 ) ) ;
#37124 = CLOSED_SHELL ( 'NONE', ( #41482, #32798, #15506, #4284, #35005, #72990, #14045, #30366, #94782, #9629, #33654, #84405, #19204, #85392, #37113, #76372, #58368, #94444, #27264, #73499, #19572, #23562, #7367, #19784, #9315, #56964, #63321, #3909, #32271, #29181, #96836, #84196, #2832, #100211, #95521, #87357, #51717, #14384, #97446, #63787, #29166, #62383, #3963, #17526, #23241, #87832, #31616, #33059, #59003, #54024, #88952, #24337, #55071, #53702, #91477, #97019, #79669, #20921, #72916, #61133, #33097, #100031, #37001, #7291, #22048, #68369, #59539, #31135, #95583, #92890, #97435, #21823, #79926, #91857, #92963 ) ) ;
#37125 = EDGE_CURVE ( 'NONE', #39121, #77364, #81173, .T. ) ;
#37126 = CARTESIAN_POINT ( 'NONE',  ( -110.9410897254133204, -25.11552134530501590, 2.805129186380271644 ) ) ;
#37127 = VERTEX_POINT ( 'NONE', #37600 ) ;
#37128 = CARTESIAN_POINT ( 'NONE',  ( -81.52287095715006160, -23.48786465467241058, 11.44779295918254469 ) ) ;
#37129 = CARTESIAN_POINT ( 'NONE',  ( 19.59260286812380514, -1.442238090573773501, 11.49999999999999645 ) ) ;
#37130 = CARTESIAN_POINT ( 'NONE',  ( -66.62287095715007013, -24.51387760970723662, 9.387446482453425389 ) ) ;
#37131 = CARTESIAN_POINT ( 'NONE',  ( -63.52287095715006160, -23.47596703998600631, 11.44779298504228926 ) ) ;
#37132 = ORIENTED_EDGE ( 'NONE', *, *, #40918, .T. ) ;
#37133 = LINE ( 'NONE', #59989, #19827 ) ;
#37134 = CARTESIAN_POINT ( 'NONE',  ( -100.6228709571500559, -23.47593901973091235, -1.443836447539001089 ) ) ;
#37135 = CARTESIAN_POINT ( 'NONE',  ( -99.85057463794808541, -25.25095808762917571, 5.344630504190060805 ) ) ;
#37136 = CARTESIAN_POINT ( 'NONE',  ( -62.62287095715004881, -23.47596703998600276, 11.44779298504227505 ) ) ;
#37137 = CARTESIAN_POINT ( 'NONE',  ( -2.355416116969162754, -19.56741566493107598, -1.500000000000002220 ) ) ;
#37138 = B_SPLINE_CURVE_WITH_KNOTS ( 'NONE', 3,
 ( #89472, #5229, #35687, #36185 ),
 .UNSPECIFIED., .F., .F.,
 ( 4, 4 ),
 ( 0.000000000000000000, 0.0001000000000000028644 ),
 .UNSPECIFIED. ) ;
#37139 = VERTEX_POINT ( 'NONE', #90389 ) ;
#37141 = B_SPLINE_CURVE_WITH_KNOTS ( 'NONE', 3,
 ( #46892, #9822, #55510, #78320, #71733, #93046 ),
 .UNSPECIFIED., .F., .F.,
 ( 4, 2, 4 ),
 ( 1.570887131794176733E-05, 0.001396322306279759555, 0.002776935741241577573 ),
 .UNSPECIFIED. ) ;
#37140 = FACE_OUTER_BOUND ( 'NONE', #5003, .T. ) ;
#37142 = CYLINDRICAL_SURFACE ( 'NONE', #77152, 84.48086791635432746 ) ;
#37143 = ADVANCED_FACE ( 'NONE', ( #70434 ), #62842, .T. ) ;
#37144 = PERSON_AND_ORGANIZATION ( #70597, #27821 ) ;
#37145 = ORIENTED_EDGE ( 'NONE', *, *, #38540, .T. ) ;
#37146 = DIRECTION ( 'NONE',  ( -0.000000000000000000, 2.173523156925979552E-06, -0.9999999999976378895 ) ) ;
#37147 = FACE_OUTER_BOUND ( 'NONE', #74963, .T. ) ;
#37148 = CARTESIAN_POINT ( 'NONE',  ( -90.58953762381672448, -23.48786465467241058, 11.44779295918254469 ) ) ;
#37149 = PLANE ( 'NONE',  #93084 ) ;
#37150 = CARTESIAN_POINT ( 'NONE',  ( 5.326923076923078426, -6.376774720514420736, 20.76772836538461320 ) ) ;
#37151 = ADVANCED_FACE ( 'NONE', ( #99484 ), #24251, .F. ) ;
#37152 = VECTOR ( 'NONE', #10350, 1000.000000000000000 ) ;
#37153 = CARTESIAN_POINT ( 'NONE',  ( 31.84105487026623393, -5.152774720514427642, -11.95870468328481806 ) ) ;
#37154 = CARTESIAN_POINT ( 'NONE',  ( -122.5228709571500616, -29.50250786944525672, 11.44777988621622811 ) ) ;
#37155 = CARTESIAN_POINT ( 'NONE',  ( -19.59816365915598979, -3.832847594873297403, -1.500000000000002220 ) ) ;
#37156 = CARTESIAN_POINT ( 'NONE',  ( -4.700032041049139409, -6.144890974841530351, 8.999999999999998224 ) ) ;
#37157 = CARTESIAN_POINT ( 'NONE',  ( -51.69889270095674760, -25.27742702178395717, 4.038250842609248714 ) ) ;
#37158 = ORIENTED_EDGE ( 'NONE', *, *, #55074, .F. ) ;
#37159 = EDGE_CURVE ( 'NONE', #57446, #97929, #5303, .T. ) ;
#37160 = TOROIDAL_SURFACE ( 'NONE', #93874, 80.18232118519038920, 9.179999999999999716 ) ;
#37161 = PLANE ( 'NONE',  #29470 ) ;
#37162 = ADVANCED_FACE ( 'NONE', ( #75645 ), #44225, .T. ) ;
#37163 = B_SPLINE_CURVE_WITH_KNOTS ( 'NONE', 3,
 ( #6616, #46693, #8124, #70014, #39064, #501 ),
 .UNSPECIFIED., .F., .F.,
 ( 4, 2, 4 ),
 ( 0.000000000000000000, 0.001380901958385397869, 0.002761803916770795737 ),
 .UNSPECIFIED. ) ;
#37164 = CIRCLE ( 'NONE', #50149, 0.8160000000000007248 ) ;
#37165 = CARTESIAN_POINT ( 'NONE',  ( -119.5910507080879199, -23.96119346886881019, -0.6495511937832016969 ) ) ;
#37166 = FACE_OUTER_BOUND ( 'NONE', #50184, .T. ) ;
#37167 = FACE_OUTER_BOUND ( 'NONE', #99694, .T. ) ;
#37168 = CARTESIAN_POINT ( 'NONE',  ( -39.65632424235193554, -23.73766607897669800, -1.055555164236461341 ) ) ;
#37169 = VECTOR ( 'NONE', #61019, 1000.000000000000114 ) ;
#37170 = CARTESIAN_POINT ( 'NONE',  ( 20.60020833695035236, 0.000000000000000000, 0.000000000000000000 ) ) ;
#37171 = CARTESIAN_POINT ( 'NONE',  ( -1.394533802543915124, -6.376774720514413630, 20.19722303762275573 ) ) ;
#37172 = VECTOR ( 'NONE', #35860, 1000.000000000000000 ) ;
#37173 = CARTESIAN_POINT ( 'NONE',  ( -34.62287095715004170, -23.73907113216990439, -1.053371485793236806 ) ) ;
#37174 = LINE ( 'NONE', #43302, #50087 ) ;
#37175 = VERTEX_POINT ( 'NONE', #55225 ) ;
#37176 = CARTESIAN_POINT ( 'NONE',  ( -19.75413285895528404, 4.560271753130525241, 11.49999999999998934 ) ) ;
#37177 = ADVANCED_FACE ( 'NONE', ( #68060 ), #29979, .T. ) ;
#37178 = CARTESIAN_POINT ( 'NONE',  ( -39.62287095715005592, -24.64898659630366851, 1.056161002820819261 ) ) ;
#37179 = CARTESIAN_POINT ( 'NONE',  ( 20.65867867180746487, 4.278699498676136415, -17.77077369076281599 ) ) ;
#37180 = CARTESIAN_POINT ( 'NONE',  ( -76.62287095715007013, -24.34917612406837861, 0.1852690917426645656 ) ) ;
#37181 = VERTEX_POINT ( 'NONE', #67564 ) ;
#37182 = DIRECTION ( 'NONE',  ( 1.084136044942898696E-16, 0.000000000000000000, -1.000000000000000000 ) ) ;
#37183 = CARTESIAN_POINT ( 'NONE',  ( -82.62287095715005592, -29.50250243563736774, 8.947779886222141599 ) ) ;
#37184 = CARTESIAN_POINT ( 'NONE',  ( -7.184633862932894743, 18.80532529184710100, -1.500000000000002220 ) ) ;
#37185 = CARTESIAN_POINT ( 'NONE',  ( -2.902382693073098707, -20.91247731031871382, 11.49999999999999645 ) ) ;
#37186 = CARTESIAN_POINT ( 'NONE',  ( -94.62287095715005592, -29.50248528299804818, 1.056150453629040253 ) ) ;
#37187 = CARTESIAN_POINT ( 'NONE',  ( 14.53198226072946220, 16.64418356588832992, 11.49999999999998934 ) ) ;
#37188 = EDGE_CURVE ( 'NONE', #47988, #51587, #97984, .T. ) ;
#37189 = CARTESIAN_POINT ( 'NONE',  ( 16.23509277041898358, 12.58620111108425377, -1.500000000000002220 ) ) ;
#37190 = CARTESIAN_POINT ( 'NONE',  ( -39.44984910185593208, -25.27805931940480377, 4.278338840711595203 ) ) ;
#37191 = B_SPLINE_CURVE_WITH_KNOTS ( 'NONE', 3,
 ( #5974, #45053, #27818, #74974, #5477, #66899, #76471, #91206, #67389, #83589, #82600, #36924, #36425, #20692, #59782 ),
 .UNSPECIFIED., .F., .F.,
 ( 4, 1, 1, 1, 1, 1, 1, 1, 1, 1, 1, 1, 4 ),
 ( 0.000000000000000000, 0.1128134007444584058, 0.2253938839207300371, 0.3395948145627014636, 0.4596754102248630236, 0.5217351900879338977, 0.5839258387389175686, 0.6481741447653697197, 0.7138810381130681337, 0.7810044549073911213, 0.8514509275565554924, 0.9240506926641786078, 1.000000000000000000 ),
 .UNSPECIFIED. ) ;
#37192 = LINE ( 'NONE', #27594, #29188 ) ;
#37193 = ORIENTED_EDGE ( 'NONE', *, *, #65521, .T. ) ;
#37194 = FACE_OUTER_BOUND ( 'NONE', #99810, .T. ) ;
#37195 = ORIENTED_EDGE ( 'NONE', *, *, #45043, .T. ) ;
#37196 = ADVANCED_FACE ( 'NONE', ( #83764 ), #14247, .F. ) ;
#37197 = CARTESIAN_POINT ( 'NONE',  ( -99.13315347086529528, -25.26009968875505507, 3.839156536065280623 ) ) ;
#37198 = B_SPLINE_SURFACE_WITH_KNOTS ( 'NONE', 3, 3, ( 
 ( #7815, #53515, #38260, #38758 ),
 ( #84438, #69218, #69727, #205 ),
 ( #8821, #45891, #29655, #68228 ),
 ( #99157, #91551, #31150, #100133 ),
 ( #70221, #54497, #22024, #62119 ),
 ( #93041, #85432, #76314, #6813 ),
 ( #37771, #18430, #40271, #1214 ) ),
 .UNSPECIFIED., .F., .F., .F.,
 ( 4, 3, 4 ),
 ( 4, 4 ),
 ( 0.0004766839783819933041, 0.1029713700210895672, 0.2054660560637971423 ),
 ( 0.3695880141246808970, 0.3707712659113398534 ),
 .UNSPECIFIED. ) ;
#37199 = CARTESIAN_POINT ( 'NONE',  ( -102.5895376238167245, -23.47596703998600631, 11.44779298504227683 ) ) ;
#37200 = ORIENTED_EDGE ( 'NONE', *, *, #48468, .F. ) ;
#37201 = EDGE_LOOP ( 'NONE', ( #12524, #9863, #36627, #86731 ) ) ;
#37202 = CARTESIAN_POINT ( 'NONE',  ( 23.60872659128563811, 0.000000000000000000, 2.097483029078132777 ) ) ;
#37203 = DIRECTION ( 'NONE',  ( -0.000000000000000000, 1.000000000000000000, -0.000000000000000000 ) ) ;
#37204 = CARTESIAN_POINT ( 'NONE',  ( -76.50807368432518274, -24.15543982623907482, -0.2315651400026599582 ) ) ;
#37205 = CARTESIAN_POINT ( 'NONE',  ( 3.086129920417311823, 20.35385046113321295, -1.500000000000002220 ) ) ;
#37206 = EDGE_CURVE ( 'NONE', #4570, #51553, #32634, .T. ) ;
#37207 = CARTESIAN_POINT ( 'NONE',  ( 5.568959250215116619, -20.88136358707659923, 11.49999999999999645 ) ) ;
#37208 = ORIENTED_EDGE ( 'NONE', *, *, #83143, .F. ) ;
#37209 = DIRECTION ( 'NONE',  ( 0.000000000000000000, 1.000000000000000000, 0.000000000000000000 ) ) ;
#37210 = DIRECTION ( 'NONE',  ( -0.000000000000000000, -1.000000000000000000, -0.000000000000000000 ) ) ;
#37211 = CARTESIAN_POINT ( 'NONE',  ( -5.491053050139323766, 21.65304554001118120, -1.500000000000002220 ) ) ;
#37212 = ADVANCED_FACE ( 'NONE', ( #42002 ), #3439, .T. ) ;
#37213 = CARTESIAN_POINT ( 'NONE',  ( 31.79364159983995464, 6.475225279485573360, -11.59305536555894278 ) ) ;
#37214 = DIRECTION ( 'NONE',  ( -0.000000000000000000, -1.000000000000000000, -0.000000000000000000 ) ) ;
#37215 = VERTEX_POINT ( 'NONE', #64855 ) ;
#37216 = ADVANCED_FACE ( 'NONE', ( #63847 ), #39978, .T. ) ;
#37217 = CARTESIAN_POINT ( 'NONE',  ( -27.83739072329610664, -5.965225279485592225, -8.084349702057698650 ) ) ;
#37218 = CARTESIAN_POINT ( 'NONE',  ( -35.52468542394368001, -24.83644354573578639, 8.397322867130093016 ) ) ;
#37219 = CARTESIAN_POINT ( 'NONE',  ( 12.60132613692001691, 16.66296579206088069, -1.500000000000002220 ) ) ;
#37220 = ORIENTED_EDGE ( 'NONE', *, *, #49978, .T. ) ;
#37222 = ORIENTED_EDGE ( 'NONE', *, *, #76201, .F. ) ;
#37221 = CARTESIAN_POINT ( 'NONE',  ( -67.53677154461657040, -24.66019654487199730, 8.947790411086115725 ) ) ;
#37223 = ORIENTED_EDGE ( 'NONE', *, *, #55005, .T. ) ;
#37224 = B_SPLINE_CURVE_WITH_KNOTS ( 'NONE', 3,
 ( #40711, #57457, #66579, #65080 ),
 .UNSPECIFIED., .F., .F.,
 ( 4, 4 ),
 ( 0.6202288146924654910, 0.6292352459645811358 ),
 .UNSPECIFIED. ) ;
#37225 = DIRECTION ( 'NONE',  ( -3.773278334453079030E-23, 0.9999999999976377785, 2.173523156925979128E-06 ) ) ;
#37226 = CARTESIAN_POINT ( 'NONE',  ( -4.502559807402421121, -20.62786074129878955, -1.500000000000002220 ) ) ;
#37227 = ORIENTED_EDGE ( 'NONE', *, *, #65268, .F. ) ;
#37228 = CARTESIAN_POINT ( 'NONE',  ( -117.5209660606645627, -23.73766607897671221, -1.055555164236445576 ) ) ;
#37229 = CARTESIAN_POINT ( 'NONE',  ( -100.4426124108961176, -25.12215675263029624, 7.101635560846706774 ) ) ;
#37230 = CARTESIAN_POINT ( 'NONE',  ( -21.05831370385527990, 5.553659732266172711, 11.49999999999998934 ) ) ;
#37231 = CARTESIAN_POINT ( 'NONE',  ( 9.950000000000006395, 0.000000000000000000, 19.30000000000000071 ) ) ;
#37232 = AXIS2_PLACEMENT_3D ( 'NONE', #47941, #79374, #47439 ) ;
#37233 = CARTESIAN_POINT ( 'NONE',  ( 32.73857899460458754, -5.965225279485572685, -13.20677013500358399 ) ) ;
#37234 = CARTESIAN_POINT ( 'NONE',  ( -79.34687923781922336, -25.27781941911278807, 5.960409260969139922 ) ) ;
#37235 = CARTESIAN_POINT ( 'NONE',  ( 16.02445091669267185, 14.69945503153335764, -1.500000000000002220 ) ) ;
#37236 = CARTESIAN_POINT ( 'NONE',  ( -71.20541289166536103, -25.31639469619771177, 4.885889946353112023 ) ) ;
#37238 = VERTEX_POINT ( 'NONE', #94760 ) ;
#37237 = CARTESIAN_POINT ( 'NONE',  ( 20.12748746789148413, 9.599020362109589755, 11.49999999999999645 ) ) ;
#37239 = CARTESIAN_POINT ( 'NONE',  ( -57.52287095715004028, -24.51387760970724372, 9.387446482453414731 ) ) ;
#37240 = CARTESIAN_POINT ( 'NONE',  ( -70.52287095715007581, -23.47596703998600631, 11.44779298504228748 ) ) ;
#37241 = PLANE ( 'NONE',  #13199 ) ;
#37242 = EDGE_LOOP ( 'NONE', ( #63843, #71280, #63116, #33750 ) ) ;
#37243 = VECTOR ( 'NONE', #62205, 1000.000000000000000 ) ;
#37244 = ORIENTED_EDGE ( 'NONE', *, *, #24448, .T. ) ;
#37245 = VECTOR ( 'NONE', #12118, 1000.000000000000114 ) ;
#37246 = ORIENTED_EDGE ( 'NONE', *, *, #17913, .F. ) ;
#37247 = AXIS2_PLACEMENT_3D ( 'NONE', #5098, #45667, #75102 ) ;
#37248 = DIRECTION ( 'NONE',  ( -1.000000000000000000, -0.000000000000000000, -0.000000000000000000 ) ) ;
#37249 = CARTESIAN_POINT ( 'NONE',  ( 21.17954554857512761, 0.9134790845329443520, -1.500000000000002220 ) ) ;
#37250 = LINE ( 'NONE', #83408, #95209 ) ;
#37251 = CARTESIAN_POINT ( 'NONE',  ( -80.51244414166535535, -25.27791972951919774, 7.563173683831821315 ) ) ;
#37252 = DIRECTION ( 'NONE',  ( 0.000000000000000000, 0.000000000000000000, 1.000000000000000000 ) ) ;
#37253 = B_SPLINE_CURVE_WITH_KNOTS ( 'NONE', 3,
 ( #19980, #91481, #97604, #5257 ),
 .UNSPECIFIED., .F., .F.,
 ( 4, 4 ),
 ( 0.000000000000000000, 9.999999999996816991E-05 ),
 .UNSPECIFIED. ) ;
#37254 = FACE_OUTER_BOUND ( 'NONE', #49626, .T. ) ;
#37255 = AXIS2_PLACEMENT_3D ( 'NONE', #64109, #57492, #26526 ) ;
#37256 = CARTESIAN_POINT ( 'NONE',  ( -16.26263985875334228, -10.51264992557365829, 11.49999999999998934 ) ) ;
#37257 = CARTESIAN_POINT ( 'NONE',  ( -38.52287095715008292, -23.72747288104469732, -1.053458166803227680 ) ) ;
#37258 = ORIENTED_EDGE ( 'NONE', *, *, #62915, .F. ) ;
#37259 = CARTESIAN_POINT ( 'NONE',  ( -15.63568348323273227, -11.59263941501104966, 11.49999999999999645 ) ) ;
#37260 = CARTESIAN_POINT ( 'NONE',  ( -115.5228709571500190, -24.63345952396256067, 9.038047939301504741 ) ) ;
#37261 = ORIENTED_EDGE ( 'NONE', *, *, #73888, .F. ) ;
#37262 = CARTESIAN_POINT ( 'NONE',  ( 2.920210193027767076, -5.876774720514413630, 19.64065332113010243 ) ) ;
#37263 = LINE ( 'NONE', #99140, #18258 ) ;
#37264 = LINE ( 'NONE', #28156, #74104 ) ;
#37265 = FACE_OUTER_BOUND ( 'NONE', #6752, .T. ) ;
#37266 = CARTESIAN_POINT ( 'NONE',  ( -10.75157073690095721, 16.42123490324765811, -1.500000000000002220 ) ) ;
#37267 = LINE ( 'NONE', #68218, #44486 ) ;
#37268 = ORIENTED_EDGE ( 'NONE', *, *, #75741, .T. ) ;
#37269 = CARTESIAN_POINT ( 'NONE',  ( 21.29926025483437257, -3.289820829717503337, 11.49999999999998934 ) ) ;
#37270 = CARTESIAN_POINT ( 'NONE',  ( -33.63538797308950734, -24.35071581493542325, 9.817618358456039473 ) ) ;
#37271 = CARTESIAN_POINT ( 'NONE',  ( 13.91401389203221406, -5.965225279485572685, 27.75920385068456042 ) ) ;
#37272 = CARTESIAN_POINT ( 'NONE',  ( -115.5228709571500616, -24.99132157543084531, 2.256160258750667502 ) ) ;
#37273 = DIRECTION ( 'NONE',  ( -2.352173255807796549E-16, 3.728519047445511252E-18, 1.000000000000000000 ) ) ;
#37274 = CARTESIAN_POINT ( 'NONE',  ( 0.1381291366035634904, -23.06709338131901532, -1.500000000000002220 ) ) ;
#37275 = ADVANCED_FACE ( 'NONE', ( #96271 ), #79538, .T. ) ;
#37276 = SHAPE_DEFINITION_REPRESENTATION ( #95185, #91803 ) ;
#37277 = CARTESIAN_POINT ( 'NONE',  ( -101.6228709571500559, -29.50250786944525672, 11.44777988621623166 ) ) ;
#37278 = CARTESIAN_POINT ( 'NONE',  ( -50.10132759428470450, -25.25249061358302782, 3.767456410489268936 ) ) ;
#37279 = CARTESIAN_POINT ( 'NONE',  ( -8.609638109768802394, 18.19638482192696216, 11.49999999999999645 ) ) ;
#37280 = CARTESIAN_POINT ( 'NONE',  ( -84.62287095715007013, -24.50321055353803601, 9.387540953477522265 ) ) ;
#37281 = CARTESIAN_POINT ( 'NONE',  ( -24.90875734969025501, 5.356774720514425603, 27.45402280011862572 ) ) ;
#37282 = CARTESIAN_POINT ( 'NONE',  ( -4.147110899021980934, -5.876774720514418959, 20.45311193189268906 ) ) ;
#37283 = FACE_OUTER_BOUND ( 'NONE', #531, .T. ) ;
#37284 = CARTESIAN_POINT ( 'NONE',  ( -63.62287095715004881, -29.50250243563736774, 8.947779886222145151 ) ) ;
#37285 = CARTESIAN_POINT ( 'NONE',  ( 11.60740158406642664, -16.16820694497113564, -1.500000000000002220 ) ) ;
#37287 = ADVANCED_FACE ( 'NONE', ( #9529 ), #18632, .T. ) ;
#37286 = CARTESIAN_POINT ( 'NONE',  ( -69.22287095715007865, -23.47593901973090169, -1.443836447538997536 ) ) ;
#37288 = CARTESIAN_POINT ( 'NONE',  ( -17.60924879254659459, 8.996216891746938060, -1.500000000000002220 ) ) ;
#37289 = EDGE_CURVE ( 'NONE', #63916, #59325, #80540, .T. ) ;
#37290 = CARTESIAN_POINT ( 'NONE',  ( -42.62371182274537773, -24.65952944569304606, 1.056160979905694353 ) ) ;
#37291 = SHAPE_REPRESENTATION ( 'Measuring Tape_Varsay\X2\0131\X0\lan', ( #218 ), #69909 ) ;
#37292 = EDGE_CURVE ( 'NONE', #1762, #70610, #31555, .T. ) ;
#37293 = B_SPLINE_CURVE_WITH_KNOTS ( 'NONE', 3,
 ( #37778, #74834, #68733, #44907 ),
 .UNSPECIFIED., .F., .F.,
 ( 4, 4 ),
 ( 0.9912077972255933789, 0.9999675692521627912 ),
 .UNSPECIFIED. ) ;
#37294 = ADVANCED_FACE ( 'NONE', ( #9029 ), #40988, .T. ) ;
#37295 = LINE ( 'NONE', #59140, #100227 ) ;
#37296 = CARTESIAN_POINT ( 'NONE',  ( -1.733151984336291695, -6.376774720514408301, 19.29154511076646017 ) ) ;
#37297 = CARTESIAN_POINT ( 'NONE',  ( -16.33875328525262560, 12.67428768300982256, 11.49999999999999645 ) ) ;
#37298 = CARTESIAN_POINT ( 'NONE',  ( -66.62287095715005592, -23.47593901973091235, -1.443836447539006196 ) ) ;
#37299 = CIRCLE ( 'NONE', #8175, 0.2500000000000011102 ) ;
#37300 = CARTESIAN_POINT ( 'NONE',  ( -97.62287095715005592, -24.64965695001468404, 8.947790433994178727 ) ) ;
#37301 = DIRECTION ( 'NONE',  ( 0.000000000000000000, -0.9999999999976377785, -2.173523156925979128E-06 ) ) ;
#37302 = CARTESIAN_POINT ( 'NONE',  ( -9.076218414377828836, -20.82814578352222767, 11.49999999999999645 ) ) ;
#37303 = EDGE_LOOP ( 'NONE', ( #30524, #96117, #5681, #9803 ) ) ;
#37304 = CARTESIAN_POINT ( 'NONE',  ( -46.62287095715003460, -23.73934037231756733, 11.05740245334329153 ) ) ;
#37305 = CARTESIAN_POINT ( 'NONE',  ( 29.72852606603716552, 4.950008708102185295, 27.41398129243886217 ) ) ;
#37306 = VECTOR ( 'NONE', #78240, 1000.000000000000000 ) ;
#37307 = CARTESIAN_POINT ( 'NONE',  ( 3.569899647507075890, 19.86734082857295647, -1.500000000000002220 ) ) ;
#37308 = EDGE_CURVE ( 'NONE', #94609, #52065, #64349, .T. ) ;
#37309 = CARTESIAN_POINT ( 'NONE',  ( 8.940588884021780203, 1.067603002178827815E-16, -3.692441190372577342 ) ) ;
#37310 = CARTESIAN_POINT ( 'NONE',  ( -41.46611000704998418, -25.27828342519987359, 4.188173683033348915 ) ) ;
#37311 = EDGE_LOOP ( 'NONE', ( #14552, #8391, #58801, #75527 ) ) ;
#37312 = VERTEX_POINT ( 'NONE', #49114 ) ;
#37313 = EDGE_CURVE ( 'NONE', #25230, #28727, #40017, .T. ) ;
#37314 = DIRECTION ( 'NONE',  ( 0.000000000000000000, 0.000000000000000000, 1.000000000000000000 ) ) ;
#37315 = CARTESIAN_POINT ( 'NONE',  ( -19.55383134093860420, 11.88776249338449986, -1.500000000000002220 ) ) ;
#37316 = DIRECTION ( 'NONE',  ( -0.000000000000000000, 2.173523156925979552E-06, -0.9999999999976378895 ) ) ;
#37317 = AXIS2_PLACEMENT_3D ( 'NONE', #12510, #98234, #21111 ) ;
#37318 = CARTESIAN_POINT ( 'NONE',  ( -19.46174652491427182, -9.421329337880418819, -1.500000000000002220 ) ) ;
#37319 = CARTESIAN_POINT ( 'NONE',  ( -123.6238847173920732, -24.51314013834316796, 0.6176544820404235026 ) ) ;
#37320 = CARTESIAN_POINT ( 'NONE',  ( -34.48367125095467145, -24.51314013834315375, 0.6176544820404091807 ) ) ;
#37321 = CARTESIAN_POINT ( 'NONE',  ( -17.14161228048114438, 11.91956482804130601, 11.49999999999999645 ) ) ;
#37322 = EDGE_LOOP ( 'NONE', ( #82045, #52333, #15836, #33080 ) ) ;
#37323 = VECTOR ( 'NONE', #88985, 1000.000000000000000 ) ;
#37324 = DIRECTION ( 'NONE',  ( 0.000000000000000000, -0.9999999999976377785, -2.173523156925979975E-06 ) ) ;
#37325 = CARTESIAN_POINT ( 'NONE',  ( -4.682628417673765142, 21.48327871026360114, -1.500000000000002220 ) ) ;
#37326 = EDGE_CURVE ( 'NONE', #17897, #44273, #83014, .T. ) ;
#37328 = CARTESIAN_POINT ( 'NONE',  ( -105.5543609335628901, -24.15602025860896163, 10.28564288303535967 ) ) ;
#37327 = VECTOR ( 'NONE', #38008, 1000.000000000000000 ) ;
#37329 = CARTESIAN_POINT ( 'NONE',  ( -40.81364289383298427, -25.29087043510296340, 2.874305797121810446 ) ) ;
#37330 = ORIENTED_EDGE ( 'NONE', *, *, #53893, .F. ) ;
#37331 = CARTESIAN_POINT ( 'NONE',  ( -25.53098197642538736, -24.91566218739149363, 4.942811707542018596 ) ) ;
#37332 = CARTESIAN_POINT ( 'NONE',  ( -90.62618068010999650, -24.83644354573578994, 8.397322867130100121 ) ) ;
#37333 = ORIENTED_EDGE ( 'NONE', *, *, #6213, .T. ) ;
#37334 = CARTESIAN_POINT ( 'NONE',  ( -72.58793278032496232, -24.35071581493543036, 9.817618358456032368 ) ) ;
#37335 = ORIENTED_EDGE ( 'NONE', *, *, #24334, .T. ) ;
#37336 = B_SPLINE_CURVE_WITH_KNOTS ( 'NONE', 3,
 ( #18216, #80111, #33436, #41059 ),
 .UNSPECIFIED., .F., .F.,
 ( 4, 4 ),
 ( 0.000000000000000000, 9.999999999997510880E-05 ),
 .UNSPECIFIED. ) ;
#37337 = VERTEX_POINT ( 'NONE', #95765 ) ;
#37338 = CARTESIAN_POINT ( 'NONE',  ( -71.62697017891946416, -24.51419770103159124, 9.386484678747166299 ) ) ;
#37339 = CARTESIAN_POINT ( 'NONE',  ( -106.6228709571500559, -29.50247984919015209, -1.443849546365048253 ) ) ;
#37340 = CARTESIAN_POINT ( 'NONE',  ( -103.2228709571500787, -23.47593901973090169, -1.443836447538996648 ) ) ;
#37341 = CARTESIAN_POINT ( 'NONE',  ( -20.33632446988539400, 1.880062042347348195, -1.500000000000002220 ) ) ;
#37342 = EDGE_CURVE ( 'NONE', #79371, #20842, #17139, .T. ) ;
#37343 = EDGE_LOOP ( 'NONE', ( #5233, #3912, #27521, #79026 ) ) ;
#37344 = CARTESIAN_POINT ( 'NONE',  ( -3.108787716482549701, -5.876774720514416295, 20.32624910079993086 ) ) ;
#37345 = CARTESIAN_POINT ( 'NONE',  ( -30.60464735295150263, -24.58764167366260622, 9.439037205594624780 ) ) ;
#37346 = EDGE_CURVE ( 'NONE', #84649, #33464, #72442, .T. ) ;
#37347 = CARTESIAN_POINT ( 'NONE',  ( -80.13654269935770458, -25.20074414427590170, 3.409327697718777195 ) ) ;
#37348 = DIRECTION ( 'NONE',  ( 0.000000000000000000, -0.9999999999976377785, -2.173523156925979128E-06 ) ) ;
#37349 = ORIENTED_EDGE ( 'NONE', *, *, #56908, .T. ) ;
#37350 = B_SPLINE_CURVE_WITH_KNOTS ( 'NONE', 3,
 ( #51151, #18690, #73003, #96821 ),
 .UNSPECIFIED., .F., .F.,
 ( 4, 4 ),
 ( 0.3289991091667107126, 0.3299998562074764052 ),
 .UNSPECIFIED. ) ;
#37351 = FACE_OUTER_BOUND ( 'NONE', #18837, .T. ) ;
#37352 = CARTESIAN_POINT ( 'NONE',  ( -29.81002072791678614, -25.26247421725459930, 5.237831151396452611 ) ) ;
#37353 = CARTESIAN_POINT ( 'NONE',  ( 15.20108283357335921, -14.20388156210760577, 11.49999999999998934 ) ) ;
#37354 = B_SPLINE_CURVE_WITH_KNOTS ( 'NONE', 3,
 ( #13787, #83808, #51876, #66622 ),
 .UNSPECIFIED., .F., .F.,
 ( 4, 4 ),
 ( 0.000000000000000000, 1.000000000000000000 ),
 .UNSPECIFIED. ) ;
#37355 = ORIENTED_EDGE ( 'NONE', *, *, #89778, .T. ) ;
#37357 = ORIENTED_EDGE ( 'NONE', *, *, #79461, .T. ) ;
#37356 = LINE ( 'NONE', #14496, #68144 ) ;
#37358 = DIRECTION ( 'NONE',  ( 0.000000000000000000, 0.000000000000000000, -1.000000000000000000 ) ) ;
#37359 = ORIENTED_EDGE ( 'NONE', *, *, #35012, .F. ) ;
#37360 = ORIENTED_EDGE ( 'NONE', *, *, #31225, .T. ) ;
#37361 = CARTESIAN_POINT ( 'NONE',  ( 30.54636625424942764, -6.376774720514426065, 1.976438700016742045 ) ) ;
#37362 = CARTESIAN_POINT ( 'NONE',  ( -128.6228709571500417, -24.64898659630529565, 1.056161002820834804 ) ) ;
#37363 = CARTESIAN_POINT ( 'NONE',  ( -118.8949125657484274, -25.24693556693654273, 3.801660433955579954 ) ) ;
#37364 = CARTESIAN_POINT ( 'NONE',  ( -40.62287095715005592, -24.83620972994591725, 8.398175272781363887 ) ) ;
#37365 = CARTESIAN_POINT ( 'NONE',  ( -92.62813586326385007, -24.35071581493543391, 9.817618358456025263 ) ) ;
#37366 = CARTESIAN_POINT ( 'NONE',  ( -100.5562042904833930, -25.00182538069145366, 7.747789668545099317 ) ) ;
#37368 = ORIENTED_EDGE ( 'NONE', *, *, #80963, .F. ) ;
#37367 = CARTESIAN_POINT ( 'NONE',  ( 21.88104185797606505, 3.448541436957560880, 11.49999999999999645 ) ) ;
#37369 = CARTESIAN_POINT ( 'NONE',  ( -108.5864066755810029, -24.65952944569305316, 1.056160979905706121 ) ) ;
#37370 = CARTESIAN_POINT ( 'NONE',  ( -22.62345309801473547, -0.4825844212548152656, 11.49999999999998934 ) ) ;
#37372 = VERTEX_POINT ( 'NONE', #26258 ) ;
#37371 = CARTESIAN_POINT ( 'NONE',  ( -111.5228709571500332, -24.51387760970725083, 9.387446482453398744 ) ) ;
#37373 = VERTEX_POINT ( 'NONE', #57231 ) ;
#37374 = CARTESIAN_POINT ( 'NONE',  ( -81.26427307513701237, -25.31500402857158605, 5.136443472453636083 ) ) ;
#37375 = VECTOR ( 'NONE', #42368, 1000.000000000000000 ) ;
#37376 = CARTESIAN_POINT ( 'NONE',  ( 0.3675393366473880818, 20.13074986235200470, -1.500000000000002220 ) ) ;
#37377 = CARTESIAN_POINT ( 'NONE',  ( -65.62287095715005592, -23.47593901973091235, -1.443836447539006196 ) ) ;
#37378 = ORIENTED_EDGE ( 'NONE', *, *, #52760, .T. ) ;
#37379 = CARTESIAN_POINT ( 'NONE',  ( -53.62287095715005592, -23.47593901973091235, -1.443836447539009749 ) ) ;
#37380 = CARTESIAN_POINT ( 'NONE',  ( -2.938769918389303459, -22.12206158279486345, -1.500000000000002220 ) ) ;
#37381 = EDGE_LOOP ( 'NONE', ( #1867, #29977, #73328, #72496 ) ) ;
#37382 = ORIENTED_EDGE ( 'NONE', *, *, #72382, .F. ) ;
#37383 = CARTESIAN_POINT ( 'NONE',  ( -101.3987937098823409, -25.16257383815580440, 6.605699142167675397 ) ) ;
#37384 = DIRECTION ( 'NONE',  ( 0.000000000000000000, 1.000000000000000000, 0.000000000000000000 ) ) ;
#37385 = DIRECTION ( 'NONE',  ( -3.773278334444166432E-23, 1.000000000000000000, 0.000000000000000000 ) ) ;
#37386 = CARTESIAN_POINT ( 'NONE',  ( 22.02124265030973760, 5.356774720514425603, 16.20402280011862217 ) ) ;
#37387 = FACE_OUTER_BOUND ( 'NONE', #37876, .T. ) ;
#37388 = VECTOR ( 'NONE', #6302, 1000.000000000000000 ) ;
#37389 = CARTESIAN_POINT ( 'NONE',  ( -4.042178566331402045, 19.10766070095605684, 11.49999999999998934 ) ) ;
#37390 = PLANE ( 'NONE',  #57137 ) ;
#37391 = AXIS2_PLACEMENT_3D ( 'NONE', #1533, #63447, #24854 ) ;
#37392 = CARTESIAN_POINT ( 'NONE',  ( -8.943896628894790979, 19.53434260886740503, 11.49999999999998934 ) ) ;
#37393 = CARTESIAN_POINT ( 'NONE',  ( -2.762050907158362989, -6.376774720514415407, 19.89644244529369033 ) ) ;
#37394 = LINE ( 'NONE', #68342, #4305 ) ;
#37395 = CARTESIAN_POINT ( 'NONE',  ( -120.5228709571500616, -24.99156044556120904, 7.747789690856173195 ) ) ;
#37396 = CARTESIAN_POINT ( 'NONE',  ( -17.76840699843883442, -14.40508365592194195, -1.500000000000002220 ) ) ;
#37397 = CIRCLE ( 'NONE', #53399, 91.74549126261076992 ) ;
#37398 = PERSON_AND_ORGANIZATION ( #70597, #27821 ) ;
#37399 = CARTESIAN_POINT ( 'NONE',  ( -106.5908009524538471, -24.15620529776629510, 10.23563542870659582 ) ) ;
#37400 = CARTESIAN_POINT ( 'NONE',  ( -127.5228709571500616, -23.47593901973090524, -1.443836447538996204 ) ) ;
#37401 = CARTESIAN_POINT ( 'NONE',  ( -14.87316555497233495, -13.31901947624662519, 11.49999999999999645 ) ) ;
#37402 = FACE_OUTER_BOUND ( 'NONE', #84241, .T. ) ;
#37403 = EDGE_CURVE ( 'NONE', #11321, #55957, #66838, .T. ) ;
#37404 = EDGE_CURVE ( 'NONE', #6142, #56961, #25450, .T. ) ;
#37405 = CARTESIAN_POINT ( 'NONE',  ( -74.54988272486899348, -24.15620529776628800, 10.23563542870659937 ) ) ;
#37406 = DIRECTION ( 'NONE',  ( 0.000000000000000000, 0.000000000000000000, -1.000000000000000000 ) ) ;
#37407 = ORIENTED_EDGE ( 'NONE', *, *, #99037, .T. ) ;
#37408 = CARTESIAN_POINT ( 'NONE',  ( -48.62287095715004881, -29.50248528299804818, 1.056150453629033370 ) ) ;
#37409 = DIRECTION ( 'NONE',  ( 1.000000000000000000, -0.000000000000000000, 0.000000000000000000 ) ) ;
#37410 = ADVANCED_FACE ( 'NONE', ( #52093 ), #36866, .F. ) ;
#37411 = CARTESIAN_POINT ( 'NONE',  ( 18.95625057990686813, 10.65820999021175730, -1.500000000000002220 ) ) ;
#37412 = CARTESIAN_POINT ( 'NONE',  ( -4.620655831143558601, -6.376774720514410077, 19.21747685089457036 ) ) ;
#37413 = CARTESIAN_POINT ( 'NONE',  ( -15.21066300689680872, 12.40131300380995860, -1.500000000000002220 ) ) ;
#37414 = EDGE_CURVE ( 'NONE', #45193, #1888, #12150, .T. ) ;
#37415 = CARTESIAN_POINT ( 'NONE',  ( -34.52287095715006160, -23.96127896942118696, -0.6493128930941864940 ) ) ;
#37416 = ORIENTED_EDGE ( 'NONE', *, *, #39916, .T. ) ;
#37417 = PERSON_AND_ORGANIZATION ( #24574, #57256 ) ;
#37418 = PLANE ( 'NONE',  #85620 ) ;
#37419 = CARTESIAN_POINT ( 'NONE',  ( 3.113719597313231002, -6.376774720514426065, 21.58936759753562029 ) ) ;
#37420 = CARTESIAN_POINT ( 'NONE',  ( 20.49162120248849561, -0.4999214236376636200, 11.49999999999999645 ) ) ;
#37421 = DIRECTION ( 'NONE',  ( 1.000000000000000000, 0.000000000000000000, -2.168404344971008868E-16 ) ) ;
#37422 = CARTESIAN_POINT ( 'NONE',  ( 29.73860345376319003, -1.682774720514426114, -1.272392034746785860 ) ) ;
#37423 = ORIENTED_EDGE ( 'NONE', *, *, #35066, .T. ) ;
#37424 = CARTESIAN_POINT ( 'NONE',  ( -109.3610823860251031, -25.28402660629545196, 4.275462642134054470 ) ) ;
#37425 = CARTESIAN_POINT ( 'NONE',  ( -40.45829750704998418, -25.28892422092284065, 3.293942890672450829 ) ) ;
#37426 = CARTESIAN_POINT ( 'NONE',  ( -116.5208648445381243, -23.73791477778912551, 11.05961554403170055 ) ) ;
#37427 = CARTESIAN_POINT ( 'NONE',  ( -85.52287095715004739, -25.00158670708909625, 2.256160236439166411 ) ) ;
#37428 = CARTESIAN_POINT ( 'NONE',  ( -124.6228709571500559, -23.48786465467241769, 11.44779295918253759 ) ) ;
#37429 = ADVANCED_FACE ( 'NONE', ( #5910 ), #67831, .T. ) ;
#37430 = CARTESIAN_POINT ( 'NONE',  ( -0.07435467474217070938, 23.09247799282200475, 11.49999999999999645 ) ) ;
#37431 = CARTESIAN_POINT ( 'NONE',  ( 15.15630024635751383, 17.02982414992789018, -1.500000000000002220 ) ) ;
#37432 = CARTESIAN_POINT ( 'NONE',  ( -110.6281927241458476, -24.40133493613049964, 9.663955038902800609 ) ) ;
#37433 = CARTESIAN_POINT ( 'NONE',  ( -5.755030174389611730, -6.376774720514410077, 19.56655654527324728 ) ) ;
#37434 = FACE_OUTER_BOUND ( 'NONE', #22006, .T. ) ;
#37435 = CARTESIAN_POINT ( 'NONE',  ( 2.903846153846159517, -5.876774720514415407, 19.99999999999999289 ) ) ;
#37436 = CARTESIAN_POINT ( 'NONE',  ( -110.5527842940492889, -24.40034930558991633, 0.3402023900116072364 ) ) ;
#37437 = VECTOR ( 'NONE', #30255, 1000.000000000000114 ) ;
#37438 = CARTESIAN_POINT ( 'NONE',  ( 11.09338859787202480, -18.89396691112096605, -1.500000000000002220 ) ) ;
#37439 = CARTESIAN_POINT ( 'NONE',  ( -129.6228709571500417, -24.66019654487200086, 8.947790411086117501 ) ) ;
#37440 = CARTESIAN_POINT ( 'NONE',  ( -41.32836283488544638, 4.132774720514426292, 39.26872235229541985 ) ) ;
#37441 = CARTESIAN_POINT ( 'NONE',  ( -77.62287095715005592, -23.73907113216990794, -1.053371485793230145 ) ) ;
#37442 = CARTESIAN_POINT ( 'NONE',  ( -78.62656218994159474, -24.51314013834315375, 0.6176544820404143987 ) ) ;
#37443 = CARTESIAN_POINT ( 'NONE',  ( -94.62287095715001328, -23.96177878511308634, 10.65340807706329507 ) ) ;
#37444 = CARTESIAN_POINT ( 'NONE',  ( -107.6228709571500701, -24.50321055353805377, 9.387540953477529371 ) ) ;
#37445 = EDGE_LOOP ( 'NONE', ( #10870, #5959, #10886, #84812 ) ) ;
#37446 = CARTESIAN_POINT ( 'NONE',  ( 13.31029742451639386, -15.53102932315203510, 11.49999999999998934 ) ) ;
#37447 = ORIENTED_EDGE ( 'NONE', *, *, #21145, .T. ) ;
#37448 = VERTEX_POINT ( 'NONE', #19632 ) ;
#37449 = ORIENTED_EDGE ( 'NONE', *, *, #100404, .F. ) ;
#37450 = VERTEX_POINT ( 'NONE', #43492 ) ;
#37451 = CARTESIAN_POINT ( 'NONE',  ( 19.24196208499951055, 12.69117723712289703, -1.500000000000002220 ) ) ;
#37452 = CARTESIAN_POINT ( 'NONE',  ( -61.63195469153195916, -24.34968618360933945, 0.1864209137778810865 ) ) ;
#37453 = CARTESIAN_POINT ( 'NONE',  ( 2.532258636284850706, -20.04889675553949147, -1.500000000000002220 ) ) ;
#37454 = ORIENTED_EDGE ( 'NONE', *, *, #29307, .T. ) ;
#37455 = CARTESIAN_POINT ( 'NONE',  ( -26.08243833712738180, -24.84481096472645234, 3.118813907533751983 ) ) ;
#37456 = DIRECTION ( 'NONE',  ( 0.000000000000000000, 0.000000000000000000, 1.000000000000000000 ) ) ;
#37457 = ADVANCED_FACE ( 'NONE', ( #74428 ), #26326, .T. ) ;
#37458 = B_SPLINE_CURVE_WITH_KNOTS ( 'NONE', 3,
 ( #46652, #69973, #8582, #55268, #100397, #25297 ),
 .UNSPECIFIED., .F., .F.,
 ( 4, 2, 4 ),
 ( 0.000000000000000000, 0.001380901958385382256, 0.002761803916770764512 ),
 .UNSPECIFIED. ) ;
#37460 = DIRECTION ( 'NONE',  ( 1.000000000000000000, 3.773278334444167608E-23, 8.201307833595939069E-29 ) ) ;
#37459 = VECTOR ( 'NONE', #10188, 1000.000000000000114 ) ;
#37461 = LINE ( 'NONE', #23213, #4316 ) ;
#37463 = ORIENTED_EDGE ( 'NONE', *, *, #48385, .F. ) ;
#37462 = CARTESIAN_POINT ( 'NONE',  ( -16.30254408640404051, -13.89340296626662230, 11.49999999999999645 ) ) ;
#37464 = DIRECTION ( 'NONE',  ( -0.000000000000000000, 1.000000000000000000, -0.000000000000000000 ) ) ;
#37465 = CARTESIAN_POINT ( 'NONE',  ( -61.53494130710347321, -24.66019654487199375, 8.947790411086119278 ) ) ;
#37466 = VERTEX_POINT ( 'NONE', #69811 ) ;
#37467 = CARTESIAN_POINT ( 'NONE',  ( -19.90621922972506397, 5.769413876575915978, 11.49999999999998934 ) ) ;
#37468 = ADVANCED_FACE ( 'NONE', ( #31241 ), #7903, .F. ) ;
#37470 = EDGE_LOOP ( 'NONE', ( #75877, #12376, #58925, #45428 ) ) ;
#37469 = CARTESIAN_POINT ( 'NONE',  ( -71.20541289166536103, -25.31502801509702749, 4.885889949323629189 ) ) ;
#37471 = CARTESIAN_POINT ( 'NONE',  ( -28.58650821181200286, -24.19308601498208233, 0.1864216068622559508 ) ) ;
#37472 = VERTEX_POINT ( 'NONE', #76403 ) ;
#37473 = CARTESIAN_POINT ( 'NONE',  ( 4.821763668436347849, -5.876774720514404748, 18.93074869776452829 ) ) ;
#37474 = ORIENTED_EDGE ( 'NONE', *, *, #49711, .T. ) ;
#37475 = CARTESIAN_POINT ( 'NONE',  ( -1.948345350117603125, -21.87844622001750139, 11.49999999999999645 ) ) ;
#37476 = CARTESIAN_POINT ( 'NONE',  ( -37.49780277816692120, -24.15620529776627379, 10.23563542870660825 ) ) ;
#37477 = CARTESIAN_POINT ( 'NONE',  ( 11.36372850657041589, -19.49111573544105624, -1.500000000000002220 ) ) ;
#37478 = CARTESIAN_POINT ( 'NONE',  ( 4.154569570224219355, 20.57273982587956240, -1.500000000000002220 ) ) ;
#37479 = DIRECTION ( 'NONE',  ( 1.000000000000000000, 3.773278334444166432E-23, 8.201307841325785021E-29 ) ) ;
#37480 = CARTESIAN_POINT ( 'NONE',  ( 5.641653616409716854, -6.376774720514420736, 20.81030773351227481 ) ) ;
#37481 = VERTEX_POINT ( 'NONE', #93132 ) ;
#37482 = ORIENTED_EDGE ( 'NONE', *, *, #15234, .T. ) ;
#37483 = ORIENTED_EDGE ( 'NONE', *, *, #72761, .F. ) ;
#37484 = CARTESIAN_POINT ( 'NONE',  ( -66.50060275550248434, -24.34968618360933235, 0.1864209137778773950 ) ) ;
#37485 = CARTESIAN_POINT ( 'NONE',  ( 15.50980990363467882, 14.95361599516425244, -1.500000000000002220 ) ) ;
#37486 = B_SPLINE_CURVE_WITH_KNOTS ( 'NONE', 3,
 ( #63381, #24782, #86190, #55760 ),
 .UNSPECIFIED., .F., .F.,
 ( 4, 4 ),
 ( 3.505114892038065263E-09, 0.001051774434365497024 ),
 .UNSPECIFIED. ) ;
#37487 = CARTESIAN_POINT ( 'NONE',  ( -86.62287095714999907, -24.51387760970724372, 9.387446482453416507 ) ) ;
#37488 = ORIENTED_EDGE ( 'NONE', *, *, #91063, .T. ) ;
#37489 = CARTESIAN_POINT ( 'NONE',  ( -16.61111445048470614, -13.04167290785011701, -1.500000000000002220 ) ) ;
#37490 = CARTESIAN_POINT ( 'NONE',  ( -52.62287095715007013, -24.50321055353805022, 9.387540953477543582 ) ) ;
#37491 = CARTESIAN_POINT ( 'NONE',  ( -64.55379694261088730, -23.96119346886879597, -0.6495511937832134652 ) ) ;
#37492 = CARTESIAN_POINT ( 'NONE',  ( -83.58262595889972602, -24.66019654487199375, 8.947790411086124607 ) ) ;
#37493 = CARTESIAN_POINT ( 'NONE',  ( -61.52287095715006160, -29.50250243563736774, 8.947779886222145151 ) ) ;
#37494 = CARTESIAN_POINT ( 'NONE',  ( -100.4381051993576506, -25.11033443737754212, 2.832404817301930056 ) ) ;
#37495 = CARTESIAN_POINT ( 'NONE',  ( 2.577866586777615154, 22.04066829813923789, -1.500000000000002220 ) ) ;
#37496 = B_SPLINE_CURVE_WITH_KNOTS ( 'NONE', 3,
 ( #58566, #89506, #81897, #67186, #98101, #49968 ),
 .UNSPECIFIED., .F., .F.,
 ( 4, 2, 4 ),
 ( 0.002936590050694640099, 0.005175337996430707382, 0.007414085942166775967 ),
 .UNSPECIFIED. ) ;
#37497 = CARTESIAN_POINT ( 'NONE',  ( -71.58081732933524677, -24.65952944569304961, 1.056160979905700570 ) ) ;
#37498 = ORIENTED_EDGE ( 'NONE', *, *, #23778, .F. ) ;
#37499 = LINE ( 'NONE', #13646, #83807 ) ;
#37500 = CARTESIAN_POINT ( 'NONE',  ( 12.28518416766336507, 5.152774720514428530, -26.38359849988869144 ) ) ;
#37501 = CARTESIAN_POINT ( 'NONE',  ( -41.84702555354165554, -25.27955840369619622, 4.480638990042419501 ) ) ;
#37502 = DIRECTION ( 'NONE',  ( -0.000000000000000000, 1.000000000000000000, -0.000000000000000000 ) ) ;
#37503 = CARTESIAN_POINT ( 'NONE',  ( -14.69715086760845857, -12.76062437926726290, -1.500000000000002220 ) ) ;
#37504 = CARTESIAN_POINT ( 'NONE',  ( 6.831138157384286203, 20.27010762675863731, -1.500000000000002220 ) ) ;
#37505 = CARTESIAN_POINT ( 'NONE',  ( -38.52287095715006870, -23.73934037231757088, 11.05740245334329153 ) ) ;
#37506 = CARTESIAN_POINT ( 'NONE',  ( -74.62287095715005592, -29.50250243563736774, 8.947779886222143375 ) ) ;
#37507 = AXIS2_PLACEMENT_3D ( 'NONE', #40020, #87191, #33398 ) ;
#37508 = CARTESIAN_POINT ( 'NONE',  ( -123.5228709571500758, -24.33832256527049154, 0.1851278514138671449 ) ) ;
#37509 = CARTESIAN_POINT ( 'NONE',  ( -89.52287095715006160, -23.47593901973090169, -1.443836447538996426 ) ) ;
#37510 = CARTESIAN_POINT ( 'NONE',  ( -20.05226876979747530, -10.47825485868949613, -1.500000000000002220 ) ) ;
#37511 = ORIENTED_EDGE ( 'NONE', *, *, #54167, .T. ) ;
#37512 = DIRECTION ( 'NONE',  ( -1.000000000000000000, -0.000000000000000000, -0.000000000000000000 ) ) ;
#37513 = CARTESIAN_POINT ( 'NONE',  ( -122.5228709571500332, -23.48783264082477018, -1.443836473390084807 ) ) ;
#37514 = CARTESIAN_POINT ( 'NONE',  ( -17.60924879254659459, 8.996216891746938060, 11.49999999999999645 ) ) ;
#37515 = EDGE_CURVE ( 'NONE', #15460, #70350, #68472, .T. ) ;
#37516 =( BOUNDED_CURVE ( )  B_SPLINE_CURVE ( 3, ( #52266, #99422, #83701, #36529 ),
 .UNSPECIFIED., .F., .T. ) 
 B_SPLINE_CURVE_WITH_KNOTS ( ( 4, 4 ),
 ( 1.466983014708610034, 1.570796326794896558 ),
 .UNSPECIFIED. ) 
 CURVE ( )  GEOMETRIC_REPRESENTATION_ITEM ( )  RATIONAL_B_SPLINE_CURVE ( ( 1.000000000000000000, 0.9991021013140741758, 0.9991021013140741758, 1.000000000000000000 ) ) 
 REPRESENTATION_ITEM ( '' )  );
#37517 = B_SPLINE_CURVE_WITH_KNOTS ( 'NONE', 3,
 ( #50262, #97422, #89317, #43150, #96927, #19786, #18796, #59366 ),
 .UNSPECIFIED., .F., .F.,
 ( 4, 2, 2, 4 ),
 ( 6.391158118963017816E-06, 0.002007136338672925718, 0.003007508928949907765, 0.004007881519226890246 ),
 .UNSPECIFIED. ) ;
#37518 = DIRECTION ( 'NONE',  ( 0.000000000000000000, -2.173523156925979552E-06, 0.9999999999976378895 ) ) ;
#37519 = ORIENTED_EDGE ( 'NONE', *, *, #78139, .T. ) ;
#37520 = CARTESIAN_POINT ( 'NONE',  ( 15.27524774227295978, -2.682774720514427003, -27.18982104163420388 ) ) ;
#37521 = EDGE_CURVE ( 'NONE', #10751, #64821, #17003, .T. ) ;
#37522 = CARTESIAN_POINT ( 'NONE',  ( 13.37813176289109407, 2.682774720514426559, -27.17274205579463242 ) ) ;
#37523 = CARTESIAN_POINT ( 'NONE',  ( 15.40532884848888884, -15.22192433072940609, 11.49999999999998934 ) ) ;
#37524 = CARTESIAN_POINT ( 'NONE',  ( -26.36181591332271168, -24.87490845783449700, 6.596758700703877487 ) ) ;
#37525 = CARTESIAN_POINT ( 'NONE',  ( 19.33761327413411024, 2.027444641817329973, -1.500000000000002220 ) ) ;
#37526 = EDGE_CURVE ( 'NONE', #25971, #32461, #67883, .T. ) ;
#37527 = SPHERICAL_SURFACE ( 'NONE', #86999, 1.000000000000000000 ) ;
#37528 = CARTESIAN_POINT ( 'NONE',  ( -82.62287095715004170, -23.73934037231757799, 11.05740245334328975 ) ) ;
#37529 = CARTESIAN_POINT ( 'NONE',  ( 18.78060722631472501, -6.265068672152646734, 11.49999999999998934 ) ) ;
#37530 = AXIS2_PLACEMENT_3D ( 'NONE', #32421, #63393, #1983 ) ;
#37531 = EDGE_LOOP ( 'NONE', ( #3898, #83648, #94530, #96734 ) ) ;
#37532 = EDGE_CURVE ( 'NONE', #66424, #19969, #79902, .T. ) ;
#37533 = CC_DESIGN_APPROVAL ( #82954, ( #48909 ) ) ;
#37534 = CARTESIAN_POINT ( 'NONE',  ( 12.41260344771940360, 16.11316662856288318, 11.49999999999999645 ) ) ;
#37535 = LINE ( 'NONE', #84697, #81274 ) ;
#37536 = EDGE_CURVE ( 'NONE', #99338, #39688, #33906, .T. ) ;
#37537 = CARTESIAN_POINT ( 'NONE',  ( -19.37210865224160017, -0.3587747205143967943, -21.60955166348796297 ) ) ;
#37538 = EDGE_LOOP ( 'NONE', ( #20724, #34558, #95889, #69155 ) ) ;
#37539 = CARTESIAN_POINT ( 'NONE',  ( -0.03754507760218557533, -22.56394946599023044, 1.600845668900849672 ) ) ;
#37540 = CARTESIAN_POINT ( 'NONE',  ( -95.52287095715001897, -24.62285846331437256, 9.038163153548218531 ) ) ;
#37541 = CARTESIAN_POINT ( 'NONE',  ( 30.56047832681638354, -2.297196155479634516, 24.67598410064775649 ) ) ;
#37542 = CARTESIAN_POINT ( 'NONE',  ( -47.52287095715007581, -23.47593901973090169, -1.443836447538997092 ) ) ;
#37543 = CARTESIAN_POINT ( 'NONE',  ( -50.93834974540679639, -25.13772890204246124, 7.016048202706616443 ) ) ;
#37544 = CARTESIAN_POINT ( 'NONE',  ( -10.42242239376218116, -17.14354752861867937, 11.49999999999998934 ) ) ;
#37545 = EDGE_CURVE ( 'NONE', #23928, #7917, #49074, .T. ) ;
#37546 = CARTESIAN_POINT ( 'NONE',  ( -32.07722060962682775, -24.86441978397624553, 8.247789967200544581 ) ) ;
#37547 = EDGE_LOOP ( 'NONE', ( #6992, #27992, #56561, #96238 ) ) ;
#37548 = CARTESIAN_POINT ( 'NONE',  ( -63.95380932530888884, -23.56000036390796737, -1.497999999999530818 ) ) ;
#37549 = CARTESIAN_POINT ( 'NONE',  ( 22.67525425759127344, 3.225002893152739247, 11.49999999999999645 ) ) ;
#37550 = PLANE ( 'NONE',  #9721 ) ;
#37551 = CARTESIAN_POINT ( 'NONE',  ( -28.52287095715005449, -23.79850909263262082, -0.6494981837137335789 ) ) ;
#37552 = CARTESIAN_POINT ( 'NONE',  ( -59.62287095715004881, -23.47593901973091235, -1.443836447539007972 ) ) ;
#37553 = DIRECTION ( 'NONE',  ( 0.000000000000000000, 3.056206645085457922E-15, -1.000000000000000000 ) ) ;
#37554 = CARTESIAN_POINT ( 'NONE',  ( -113.6228709571500559, -23.48786465467241769, 11.44779295918254114 ) ) ;
#37555 = VECTOR ( 'NONE', #36482, 1000.000000000000000 ) ;
#37556 = CARTESIAN_POINT ( 'NONE',  ( -5.576923076923074873, -5.876774720514426953, 21.75000000000000711 ) ) ;
#37557 = VERTEX_POINT ( 'NONE', #84029 ) ;
#37558 = CARTESIAN_POINT ( 'NONE',  ( -20.32544160278596834, -1.370942541838689799, -1.500000000000002220 ) ) ;
#37559 = VERTEX_POINT ( 'NONE', #60716 ) ;
#37560 = B_SPLINE_CURVE_WITH_KNOTS ( 'NONE', 3,
 ( #82800, #44257, #75186, #68092 ),
 .UNSPECIFIED., .F., .F.,
 ( 4, 4 ),
 ( 4.163336342344337027E-17, 0.001341346153846206812 ),
 .UNSPECIFIED. ) ;
#37561 = EDGE_CURVE ( 'NONE', #2264, #57603, #88355, .T. ) ;
#37562 = CARTESIAN_POINT ( 'NONE',  ( -1.334576548209915225, -22.92891363262047832, 11.49999999999998934 ) ) ;
#37563 = CARTESIAN_POINT ( 'NONE',  ( 1.751198251822017937, 22.56127314141087581, 2.100000000000000089 ) ) ;
#37564 = ORIENTED_EDGE ( 'NONE', *, *, #4902, .F. ) ;
#37565 = CARTESIAN_POINT ( 'NONE',  ( -108.6235313111936449, -24.66019654487200441, 8.947790411086108620 ) ) ;
#37567 = EDGE_CURVE ( 'NONE', #76180, #6118, #18020, .T. ) ;
#37566 = CARTESIAN_POINT ( 'NONE',  ( -77.62661404843181856, -24.51419770103158768, 9.386484678747166299 ) ) ;
#37568 = CARTESIAN_POINT ( 'NONE',  ( -96.62287095715002749, -23.72747288104441665, -1.053458166803660889 ) ) ;
#37570 = ORIENTED_EDGE ( 'NONE', *, *, #60657, .F. ) ;
#37569 = CARTESIAN_POINT ( 'NONE',  ( 10.86157628581156764, 18.25448884030880592, 11.49999999999999645 ) ) ;
#37571 = B_SPLINE_CURVE_WITH_KNOTS ( 'NONE', 3,
 ( #99150, #6316, #98150, #29650 ),
 .UNSPECIFIED., .F., .F.,
 ( 4, 4 ),
 ( 0.000000000000000000, 0.0001000000000000167422 ),
 .UNSPECIFIED. ) ;
#37572 = ORIENTED_EDGE ( 'NONE', *, *, #96714, .T. ) ;
#37573 = CARTESIAN_POINT ( 'NONE',  ( 2.577866586777615154, 22.04066829813923789, 11.49999999999998934 ) ) ;
#37574 = AXIS2_PLACEMENT_3D ( 'NONE', #97925, #28419, #59385 ) ;
#37575 = CARTESIAN_POINT ( 'NONE',  ( -4.647353109605855792, 20.10343637636090719, 11.49999999999998934 ) ) ;
#37576 = ORIENTED_EDGE ( 'NONE', *, *, #82237, .F. ) ;
#37577 = ORIENTED_EDGE ( 'NONE', *, *, #90154, .T. ) ;
#37578 = CARTESIAN_POINT ( 'NONE',  ( -4.537657931416015700, -6.376774720514410077, 19.25713806424188235 ) ) ;
#37579 = EDGE_CURVE ( 'NONE', #35568, #85754, #10915, .T. ) ;
#37580 = CARTESIAN_POINT ( 'NONE',  ( -54.92287095715006018, -23.47596703998600631, 11.44779298504227683 ) ) ;
#37581 = ORIENTED_EDGE ( 'NONE', *, *, #94468, .F. ) ;
#37582 = ORIENTED_EDGE ( 'NONE', *, *, #43418, .T. ) ;
#37583 = CARTESIAN_POINT ( 'NONE',  ( -121.5228709571500616, -23.47596703998600631, 11.44779298504227860 ) ) ;
#37584 = CARTESIAN_POINT ( 'NONE',  ( 19.72776355195876263, -0.3587747205144265483, 28.39950002376595606 ) ) ;
#37585 = CARTESIAN_POINT ( 'NONE',  ( -1.025521031027718299, 20.81036885881322362, -1.500000000000002220 ) ) ;
#37587 = EDGE_CURVE ( 'NONE', #84975, #70943, #16506, .T. ) ;
#37586 = CARTESIAN_POINT ( 'NONE',  ( -3.204121956075930200, -21.57847171274271858, 11.49999999999999645 ) ) ;
#37588 = CARTESIAN_POINT ( 'NONE',  ( -40.72474911149932097, -25.31583763591767067, 5.047107887422168204 ) ) ;
#37589 = SECURITY_CLASSIFICATION ( '', '', #2864 ) ;
#37590 = CARTESIAN_POINT ( 'NONE',  ( -78.64224600554152289, -23.73791477778911840, 11.05961554403170588 ) ) ;
#37591 = CARTESIAN_POINT ( 'NONE',  ( -1.649324495273077451, -22.40575143947253167, -1.500000000000002220 ) ) ;
#37592 = CARTESIAN_POINT ( 'NONE',  ( -51.14398700470657388, -25.31296689817077805, 4.389973502500959412 ) ) ;
#37593 = VERTEX_POINT ( 'NONE', #78909 ) ;
#37594 = DIRECTION ( 'NONE',  ( 0.000000000000000000, -1.000000000000000000, 0.000000000000000000 ) ) ;
#37595 = AXIS2_PLACEMENT_3D ( 'NONE', #49755, #25896, #34515 ) ;
#37596 = FACE_OUTER_BOUND ( 'NONE', #77982, .T. ) ;
#37597 = CC_DESIGN_APPROVAL ( #82276, ( #11661 ) ) ;
#37598 = ORIENTED_EDGE ( 'NONE', *, *, #65023, .F. ) ;
#37599 = ORIENTED_EDGE ( 'NONE', *, *, #74274, .T. ) ;
#37600 = CARTESIAN_POINT ( 'NONE',  ( -92.62287095715005592, -24.66019654487199730, 8.947790411086124607 ) ) ;
#37601 = CC_DESIGN_DATE_AND_TIME_ASSIGNMENT ( #26182, #96202, ( #96129 ) ) ;
#37602 = ORIENTED_EDGE ( 'NONE', *, *, #87958, .F. ) ;
#37603 = CARTESIAN_POINT ( 'NONE',  ( -21.20786952941880443, -2.223526401999901925, -1.500000000000002220 ) ) ;
#37604 = ORIENTED_EDGE ( 'NONE', *, *, #62267, .T. ) ;
#37605 = CARTESIAN_POINT ( 'NONE',  ( -50.62287095715005592, -25.00182538069145011, 7.747789668545097541 ) ) ;
#37606 = CARTESIAN_POINT ( 'NONE',  ( -14.15979099334852798, -15.53166555317341135, 11.49999999999998934 ) ) ;
#37607 = CARTESIAN_POINT ( 'NONE',  ( -30.49975201380029333, -24.26950064823562059, 0.04395666736089841320 ) ) ;
#37608 = FACE_OUTER_BOUND ( 'NONE', #18374, .T. ) ;
#37609 = CARTESIAN_POINT ( 'NONE',  ( -64.52287095715006160, -29.50247984919015209, -1.443849546365056913 ) ) ;
#37610 = CARTESIAN_POINT ( 'NONE',  ( 0.1985894851802381678, 21.93841921393417849, -1.500000000000002220 ) ) ;
#37611 = CARTESIAN_POINT ( 'NONE',  ( -87.52215351861700299, -23.48783264082478794, -1.443836473390063935 ) ) ;
#37612 = EDGE_LOOP ( 'NONE', ( #52290, #66589, #39041, #43494 ) ) ;
#37613 = CARTESIAN_POINT ( 'NONE',  ( 29.74616903497430442, -6.356993644837154456, 26.56043482791313082 ) ) ;
#37614 = CARTESIAN_POINT ( 'NONE',  ( -84.60374780145698992, -23.48786465467241413, 11.44779295918254469 ) ) ;
#37615 = CARTESIAN_POINT ( 'NONE',  ( -4.686006777320704586, -0.3587747205144265483, 29.60911411231907309 ) ) ;
#37616 = CARTESIAN_POINT ( 'NONE',  ( -20.46793573446543490, -22.99545800618565750, 10.97511746239722186 ) ) ;
#37617 = CARTESIAN_POINT ( 'NONE',  ( 19.98943718749924159, -7.363913660680385220, -1.500000000000002220 ) ) ;
#37618 = CARTESIAN_POINT ( 'NONE',  ( -55.62287095715006302, -23.48786465467240703, 11.44779295918255180 ) ) ;
#37619 = CARTESIAN_POINT ( 'NONE',  ( -107.5179555912922922, -23.96169478059713853, 10.65365249895717348 ) ) ;
#37620 = CARTESIAN_POINT ( 'NONE',  ( 14.46675407819882331, -3.972730170967898378, -28.29579275198952359 ) ) ;
#37621 = CARTESIAN_POINT ( 'NONE',  ( -85.62287095715005592, -24.14406661707769075, 10.28769366152060627 ) ) ;
#37622 = CARTESIAN_POINT ( 'NONE',  ( -12.88509029660790617, -18.40938060607246740, -1.500000000000002220 ) ) ;
#37623 = B_SPLINE_SURFACE_WITH_KNOTS ( 'NONE', 3, 1, ( 
 ( #18609, #4403 ),
 ( #20606, #11500 ),
 ( #49583, #74402 ),
 ( #3416, #59187 ),
 ( #96741, #35354 ),
 ( #96249, #57207 ),
 ( #73905, #34848 ),
 ( #42479, #66315 ),
 ( #27238, #89135 ),
 ( #80517, #19608 ),
 ( #50571, #28227 ),
 ( #41976, #81526 ),
 ( #51074, #12000 ),
 ( #72918, #12500 ),
 ( #43465, #4896 ) ),
 .UNSPECIFIED., .F., .F., .F.,
 ( 4, 1, 1, 1, 1, 1, 1, 1, 1, 1, 1, 1, 4 ),
 ( 2, 2 ),
 ( 0.000000000000000000, 0.08433472199262467828, 0.1670523184160704888, 0.2495660772409616646, 0.3327404818018447341, 0.4159148863627272763, 0.4978280095399966187, 0.5803725886080506324, 0.6646001210565021244, 0.7494666931126173770, 0.8325102339401406759, 0.9156392816681737656, 1.000000000000000000 ),
 ( 0.000000000000000000, 1.000000000000000000 ),
 .UNSPECIFIED. ) ;
#37624 = CARTESIAN_POINT ( 'NONE',  ( -129.5228709571500474, -24.66019654487199730, 8.947790411086115725 ) ) ;
#37625 = ORIENTED_EDGE ( 'NONE', *, *, #3527, .T. ) ;
#37626 = DIRECTION ( 'NONE',  ( 0.000000000000000000, -2.173523156925979552E-06, 0.9999999999976378895 ) ) ;
#37627 = CARTESIAN_POINT ( 'NONE',  ( 13.16580039582533423, -14.52177825760336205, 11.49999999999999645 ) ) ;
#37628 = PLANE ( 'NONE',  #85975 ) ;
#37629 = LINE ( 'NONE', #90421, #2656 ) ;
#37630 = ORIENTED_EDGE ( 'NONE', *, *, #65153, .F. ) ;
#37631 = CARTESIAN_POINT ( 'NONE',  ( -69.67892052170711281, -25.30561282914882071, 4.980651892393407998 ) ) ;
#37632 = CARTESIAN_POINT ( 'NONE',  ( -124.4728709571500360, -25.40558663563427189, 5.000950442582704270 ) ) ;
#37633 = CARTESIAN_POINT ( 'NONE',  ( -100.5515626640960960, -25.25095778426572224, 5.205058283467153046 ) ) ;
#37634 = DIRECTION ( 'NONE',  ( -1.000000000000000000, 0.000000000000000000, 0.000000000000000000 ) ) ;
#37635 = CARTESIAN_POINT ( 'NONE',  ( -13.19171355488933983, -14.64934158388261665, -1.500000000000002220 ) ) ;
#37636 = B_SPLINE_CURVE_WITH_KNOTS ( 'NONE', 3,
 ( #69071, #36132, #37621, #52852, #14772, #98009, #44252, #99995 ),
 .UNSPECIFIED., .F., .F.,
 ( 4, 2, 2, 4 ),
 ( 0.000000000000000000, 0.002001079623178217588, 0.003001619434767328117, 0.004002159246356438646 ),
 .UNSPECIFIED. ) ;
#37637 = ORIENTED_EDGE ( 'NONE', *, *, #65166, .T. ) ;
#37638 = VECTOR ( 'NONE', #59133, 1000.000000000000000 ) ;
#37639 = EDGE_CURVE ( 'NONE', #90018, #76914, #14473, .T. ) ;
#37640 = CIRCLE ( 'NONE', #50620, 1.049999999999998934 ) ;
#37641 = CARTESIAN_POINT ( 'NONE',  ( -110.3346797185884327, -25.19502912051678933, 3.293943094755625633 ) ) ;
#37642 = CARTESIAN_POINT ( 'NONE',  ( 0.000000000000000000, -2.056774720514426669, 0.000000000000000000 ) ) ;
#37643 = EDGE_CURVE ( 'NONE', #79116, #82889, #10166, .T. ) ;
#37644 = CALENDAR_DATE ( 2026, 9, 10 ) ;
#37645 = ORIENTED_EDGE ( 'NONE', *, *, #55894, .F. ) ;
#37646 = CARTESIAN_POINT ( 'NONE',  ( -46.22287095715007155, -23.47593901973090880, -1.443836447538998424 ) ) ;
#37647 = LINE ( 'NONE', #20406, #44244 ) ;
#37648 = CARTESIAN_POINT ( 'NONE',  ( -55.59260180617345526, -24.40034930558990922, 0.3402023900116022959 ) ) ;
#37649 = CARTESIAN_POINT ( 'NONE',  ( -99.33721417192995773, -25.26638451439988842, 7.148560506356232302 ) ) ;
#37650 = DIRECTION ( 'NONE',  ( -1.000000000000000000, -3.773278334444166432E-23, -8.201307841325785021E-29 ) ) ;
#37651 = FACE_OUTER_BOUND ( 'NONE', #59004, .T. ) ;
#37652 = CARTESIAN_POINT ( 'NONE',  ( -107.5517470719624527, -24.34968618360934656, 0.1864209137778970737 ) ) ;
#37653 = CARTESIAN_POINT ( 'NONE',  ( -7.473237707827510512, 18.53023608995856009, 11.49999999999998934 ) ) ;
#37654 = EDGE_CURVE ( 'NONE', #49798, #20665, #8907, .T. ) ;
#37655 = CARTESIAN_POINT ( 'NONE',  ( -107.6228709571500701, -29.50250243563736774, 8.947779886222136270 ) ) ;
#37656 = CARTESIAN_POINT ( 'NONE',  ( -45.60106363764529647, -24.15602025860896163, 10.28564288303535434 ) ) ;
#37657 = ORIENTED_EDGE ( 'NONE', *, *, #9439, .T. ) ;
#37658 = AXIS2_PLACEMENT_3D ( 'NONE', #41263, #2211, #2707 ) ;
#37660 = CARTESIAN_POINT ( 'NONE',  ( -119.5880683731135719, -24.65952944569305316, 1.056160979905713226 ) ) ;
#37659 = CC_DESIGN_APPROVAL ( #47590, ( #63621 ) ) ;
#37661 = CARTESIAN_POINT ( 'NONE',  ( -112.5228709571500616, -23.47593901973090524, -1.443836447538996426 ) ) ;
#37662 = CARTESIAN_POINT ( 'NONE',  ( 30.93860345374796594, -6.475225279485573360, 29.23160796525321814 ) ) ;
#37663 = CARTESIAN_POINT ( 'NONE',  ( -39.48050984162963317, -24.65952944569304250, 1.056160979905697017 ) ) ;
#37664 = DIRECTION ( 'NONE',  ( -0.06283980576413537855, -0.000000000000000000, -0.9980236263794188822 ) ) ;
#37665 = CARTESIAN_POINT ( 'NONE',  ( -51.61156992512332664, -25.31574345023019035, 4.398685571975743613 ) ) ;
#37666 = DIRECTION ( 'NONE',  ( -9.779078418496698369E-14, 0.000000000000000000, -1.000000000000000000 ) ) ;
#37667 = FACE_OUTER_BOUND ( 'NONE', #18597, .T. ) ;
#37668 = ORIENTED_EDGE ( 'NONE', *, *, #96759, .F. ) ;
#37669 = CARTESIAN_POINT ( 'NONE',  ( -3.898967980886277829, 19.90457959416237088, -1.500000000000002220 ) ) ;
#37670 = AXIS2_PLACEMENT_3D ( 'NONE', #83524, #29748, #795 ) ;
#37671 = CARTESIAN_POINT ( 'NONE',  ( -54.52287095715005449, -23.47593901973090169, -1.443836447538997092 ) ) ;
#37672 = CARTESIAN_POINT ( 'NONE',  ( 20.59899778430702710, 4.215349365190572684, -17.99869025002255896 ) ) ;
#37673 = CARTESIAN_POINT ( 'NONE',  ( -71.62287095715005592, -24.64965695001468404, 8.947790433994184056 ) ) ;
#37674 = ORIENTED_EDGE ( 'NONE', *, *, #81505, .T. ) ;
#37676 = EDGE_CURVE ( 'NONE', #62214, #46809, #86029, .T. ) ;
#37675 = CARTESIAN_POINT ( 'NONE',  ( -77.52287095715006160, -23.47596703998600631, 11.44779298504228571 ) ) ;
#37677 = CARTESIAN_POINT ( 'NONE',  ( -1.304987980769231948, -5.876774720514412742, 19.76512419871795245 ) ) ;
#37678 = CARTESIAN_POINT ( 'NONE',  ( -11.28321777122536140, 16.66956161807075887, -1.500000000000002220 ) ) ;
#37679 = CARTESIAN_POINT ( 'NONE',  ( -16.00611555608923098, 13.71732778110762219, 11.49999999999999645 ) ) ;
#37680 = DIRECTION ( 'NONE',  ( -3.773278334453079030E-23, 0.9999999999976377785, 2.173523156925979128E-06 ) ) ;
#37681 = CARTESIAN_POINT ( 'NONE',  ( -2.366842300981895519, -21.98859952056468714, -1.500000000000002220 ) ) ;
#37682 = EDGE_CURVE ( 'NONE', #87638, #64400, #73793, .T. ) ;
#37683 = CARTESIAN_POINT ( 'NONE',  ( 15.21836549854886123, 13.79734045396011943, -1.500000000000002220 ) ) ;
#37684 = CARTESIAN_POINT ( 'NONE',  ( -46.62287095715004881, -23.47596703998600276, 11.44779298504227505 ) ) ;
#37685 = AXIS2_PLACEMENT_3D ( 'NONE', #18783, #63999, #78172 ) ;
#37686 = CARTESIAN_POINT ( 'NONE',  ( 16.15056352287344410, 5.152774720514413431, -27.77856273171768109 ) ) ;
#37687 = ORIENTED_EDGE ( 'NONE', *, *, #78652, .T. ) ;
#37688 = DIRECTION ( 'NONE',  ( 0.8788171126619707119, -0.4771587602595986910, 0.000000000000000000 ) ) ;
#37689 = VERTEX_POINT ( 'NONE', #2814 ) ;
#37690 = CARTESIAN_POINT ( 'NONE',  ( -100.1132281341688639, -25.12645423365821529, 2.865483173913088599 ) ) ;
#37691 = CARTESIAN_POINT ( 'NONE',  ( -94.62287095715005592, -29.50250786944525672, 11.44777988621623344 ) ) ;
#37692 = ORIENTED_EDGE ( 'NONE', *, *, #86923, .T. ) ;
#37693 = ORIENTED_EDGE ( 'NONE', *, *, #19138, .T. ) ;
#37694 = ORIENTED_EDGE ( 'NONE', *, *, #67491, .T. ) ;
#37695 = CARTESIAN_POINT ( 'NONE',  ( -58.62287095715004881, -29.50250243563736774, 8.947779886222145151 ) ) ;
#37696 = CARTESIAN_POINT ( 'NONE',  ( -71.62287095715005592, -24.64965695001468404, 8.947790433994184056 ) ) ;
#37697 = CARTESIAN_POINT ( 'NONE',  ( -107.6228709571500701, -29.50247984919015209, -1.443849546365048253 ) ) ;
#37698 = CARTESIAN_POINT ( 'NONE',  ( 19.88596897151998633, -5.565664080715476913, -1.500000000000002220 ) ) ;
#37699 = CARTESIAN_POINT ( 'NONE',  ( -21.01067979154616694, 5.129389437380057259, 11.49999999999999645 ) ) ;
#37700 = VERTEX_POINT ( 'NONE', #32241 ) ;
#37701 = CARTESIAN_POINT ( 'NONE',  ( -83.52287095715006160, -29.50250243563736774, 8.947779886222141599 ) ) ;
#37702 = CARTESIAN_POINT ( 'NONE',  ( -20.27875734969026311, 3.456774720514426136, 24.00402280011862288 ) ) ;
#37703 = CARTESIAN_POINT ( 'NONE',  ( -22.19192207843486386, -2.872123673023632584, -1.500000000000002220 ) ) ;
#37704 = CARTESIAN_POINT ( 'NONE',  ( -34.52287095715006870, -23.96177878511308634, 10.65340807706330573 ) ) ;
#37705 = CARTESIAN_POINT ( 'NONE',  ( -84.51365791126548288, -23.96119346886880663, -0.6495511937832096905 ) ) ;
#37706 = EDGE_LOOP ( 'NONE', ( #45138, #42060, #33848, #34730 ) ) ;
#37707 = CARTESIAN_POINT ( 'NONE',  ( -119.1719706626307413, -25.37174747607477698, 5.923220291595613141 ) ) ;
#37708 = CARTESIAN_POINT ( 'NONE',  ( 6.365284455128204399, -6.376774720514413630, 19.73076923076922640 ) ) ;
#37709 = VECTOR ( 'NONE', #12926, 1000.000000000000114 ) ;
#37710 = CARTESIAN_POINT ( 'NONE',  ( 19.40856703110355852, -7.758221025823637262, 11.49999999999998934 ) ) ;
#37711 = ORIENTED_EDGE ( 'NONE', *, *, #30062, .F. ) ;
#37712 = EDGE_CURVE ( 'NONE', #38912, #42203, #86352, .T. ) ;
#37714 = ORIENTED_EDGE ( 'NONE', *, *, #41919, .F. ) ;
#37713 = CARTESIAN_POINT ( 'NONE',  ( -67.64073919962002890, -23.96169478059713853, 10.65365249895717881 ) ) ;
#37715 = VERTEX_POINT ( 'NONE', #47980 ) ;
#37716 = DIRECTION ( 'NONE',  ( -1.000000000000000000, -3.773278334444166432E-23, -8.201307841325785021E-29 ) ) ;
#37717 = CARTESIAN_POINT ( 'NONE',  ( -1.424071398598787397, -21.11453822904667277, -1.500000000000002220 ) ) ;
#37718 = ORIENTED_EDGE ( 'NONE', *, *, #71035, .F. ) ;
#37719 = CARTESIAN_POINT ( 'NONE',  ( -117.5178561819711405, -24.34968618360934656, 0.1864209137778901071 ) ) ;
#37720 = PLANE ( 'NONE',  #54763 ) ;
#37721 = CARTESIAN_POINT ( 'NONE',  ( 21.67628855941699939, -2.339797445609365756, -1.500000000000002220 ) ) ;
#37722 = CARTESIAN_POINT ( 'NONE',  ( -38.22287095715006444, -23.47596703998600276, 11.44779298504227683 ) ) ;
#37723 = DIRECTION ( 'NONE',  ( -1.000000000000000000, 0.000000000000000000, 0.000000000000000000 ) ) ;
#37724 = CARTESIAN_POINT ( 'NONE',  ( -51.70072539166533687, -29.50249165357793046, 3.987142867003085733 ) ) ;
#37725 = CARTESIAN_POINT ( 'NONE',  ( -15.31764660673900558, 15.41647822393392175, -1.500000000000002220 ) ) ;
#37726 = CARTESIAN_POINT ( 'NONE',  ( -79.23861220474265110, -25.15702039326336248, 6.966313354365812671 ) ) ;
#37728 = ORIENTED_EDGE ( 'NONE', *, *, #54196, .T. ) ;
#37727 = CARTESIAN_POINT ( 'NONE',  ( -7.907391756136429528, -20.87048397725295956, 11.49999999999999645 ) ) ;
#37729 = CARTESIAN_POINT ( 'NONE',  ( -45.62287095715005592, -23.85196035786901447, -0.8779234886475056898 ) ) ;
#37730 = CARTESIAN_POINT ( 'NONE',  ( -85.58227397182980667, -24.92592662359561473, 8.075495903018000021 ) ) ;
#37731 = CARTESIAN_POINT ( 'NONE',  ( 32.80655795465876423, -4.354682733740601108, -4.311478614910781992 ) ) ;
#37732 = EDGE_LOOP ( 'NONE', ( #95844, #78560, #42260, #38570 ) ) ;
#37733 = ADVANCED_FACE ( 'NONE', ( #71319 ), #71822, .F. ) ;
#37734 = ORIENTED_EDGE ( 'NONE', *, *, #23633, .T. ) ;
#37735 = VECTOR ( 'NONE', #42040, 1000.000000000000114 ) ;
#37736 = EDGE_LOOP ( 'NONE', ( #43724, #3583, #92716, #22196 ) ) ;
#37737 = CC_DESIGN_SECURITY_CLASSIFICATION ( #96129, ( #100431 ) ) ;
#37738 = CARTESIAN_POINT ( 'NONE',  ( -44.62287095715006302, -24.50216790748206108, 0.6166512839542489521 ) ) ;
#37739 = CARTESIAN_POINT ( 'NONE',  ( 15.74494995282791088, 14.18698661492608615, 11.49999999999998934 ) ) ;
#37740 = CARTESIAN_POINT ( 'NONE',  ( -42.62287095715004881, -24.64898659630367561, 1.056161002820819261 ) ) ;
#37741 = CARTESIAN_POINT ( 'NONE',  ( -79.79245360944284471, -25.03138266959759406, 7.413205403593926768 ) ) ;
#37742 = LINE ( 'NONE', #68702, #38911 ) ;
#37743 = LINE ( 'NONE', #68704, #8638 ) ;
#37745 = CARTESIAN_POINT ( 'NONE',  ( -37.62287095715005592, -23.48786465467240347, 11.44779295918255180 ) ) ;
#37744 = VECTOR ( 'NONE', #57399, 1000.000000000000114 ) ;
#37746 = CARTESIAN_POINT ( 'NONE',  ( -51.76059860518384426, -25.30455739459534215, 5.531002304556869476 ) ) ;
#37747 = ORIENTED_EDGE ( 'NONE', *, *, #47248, .F. ) ;
#37748 = CARTESIAN_POINT ( 'NONE',  ( -19.27395093635484713, 2.380100695660296140, 11.49999999999999645 ) ) ;
#37749 = CARTESIAN_POINT ( 'NONE',  ( 0.8126045299064811323, -1.450440077808301975, 8.999999999999998224 ) ) ;
#37750 = VECTOR ( 'NONE', #54207, 1000.000000000000000 ) ;
#37751 = EDGE_CURVE ( 'NONE', #11757, #25493, #98040, .T. ) ;
#37752 = EDGE_CURVE ( 'NONE', #91151, #84743, #10407, .T. ) ;
#37753 = ORIENTED_EDGE ( 'NONE', *, *, #72315, .T. ) ;
#37754 = CARTESIAN_POINT ( 'NONE',  ( 3.116263380642223968, -6.376774720514401196, 18.40799819116699609 ) ) ;
#37755 = CARTESIAN_POINT ( 'NONE',  ( -24.90875734969025501, 5.965225279485572685, 26.43402280011862615 ) ) ;
#37756 = B_SPLINE_CURVE_WITH_KNOTS ( 'NONE', 3,
 ( #86073, #16547, #47523, #336, #31282, #46026, #93175, #23662 ),
 .UNSPECIFIED., .F., .F.,
 ( 4, 2, 2, 4 ),
 ( 6.391158118953789392E-06, 0.002007136338672918345, 0.003007508928949900826, 0.004007881519226882440 ),
 .UNSPECIFIED. ) ;
#37757 = DIRECTION ( 'NONE',  ( -0.000000000000000000, 1.000000000000000000, -0.000000000000000000 ) ) ;
#37758 = CARTESIAN_POINT ( 'NONE',  ( -10.75157073690095721, 16.42123490324765811, 11.49999999999998934 ) ) ;
#37759 = B_SPLINE_SURFACE_WITH_KNOTS ( 'NONE', 3, 3, ( 
 ( #73088, #27897, #58852, #66980 ),
 ( #51744, #44128, #57872, #88810 ),
 ( #19276, #50248, #14156, #61859 ),
 ( #67973, #68957, #68462, #60860 ) ),
 .UNSPECIFIED., .F., .F., .F.,
 ( 4, 4 ),
 ( 4, 4 ),
 ( 0.4256160872305289611, 0.5688882139226333345 ),
 ( 0.3941186795217973549, 0.4076941526734072507 ),
 .UNSPECIFIED. ) ;
#37760 = CARTESIAN_POINT ( 'NONE',  ( -117.6228709571501128, -23.96177878511309345, 10.65340807706329507 ) ) ;
#37761 = ORIENTED_EDGE ( 'NONE', *, *, #38769, .T. ) ;
#37762 = B_SPLINE_CURVE_WITH_KNOTS ( 'NONE', 3,
 ( #86794, #25400, #56375, #17286, #1577, #32010 ),
 .UNSPECIFIED., .F., .F.,
 ( 4, 2, 4 ),
 ( 6.391158118969316353E-06, 0.001387004593080788748, 0.002767618028042608501 ),
 .UNSPECIFIED. ) ;
#37763 = CARTESIAN_POINT ( 'NONE',  ( -19.35566633068252074, -9.524217769563914970, 11.49999999999998934 ) ) ;
#37764 = CARTESIAN_POINT ( 'NONE',  ( -33.53189478466186557, -24.51419770103157347, 9.386484678747185839 ) ) ;
#37765 = CARTESIAN_POINT ( 'NONE',  ( -40.48180610888380926, -24.63355581998386512, 0.9682620441943814438 ) ) ;
#37766 = CARTESIAN_POINT ( 'NONE',  ( -99.52818128268205555, -25.18439484051665644, 3.976272486753747781 ) ) ;
#37767 = CARTESIAN_POINT ( 'NONE',  ( 14.79121776280621425, -17.69394282334246427, -1.500000000000002220 ) ) ;
#37768 = EDGE_CURVE ( 'NONE', #72199, #81001, #24186, .T. ) ;
#37769 = EDGE_CURVE ( 'NONE', #52694, #65117, #93194, .T. ) ;
#37770 = PERSON_AND_ORGANIZATION ( #70597, #27821 ) ;
#37771 = CARTESIAN_POINT ( 'NONE',  ( -93.62357230945337960, -24.65952944569305316, 1.056160979905701458 ) ) ;
#37772 = CARTESIAN_POINT ( 'NONE',  ( -89.52287095715006160, -23.47596703998600631, 11.44779298504228393 ) ) ;
#37773 = CARTESIAN_POINT ( 'NONE',  ( -15.79248070760165490, 12.47733877207048181, 11.49999999999999645 ) ) ;
#37774 = DIRECTION ( 'NONE',  ( -1.000000000000000000, 0.000000000000000000, -0.000000000000000000 ) ) ;
#37775 = LINE ( 'NONE', #76318, #43657 ) ;
#37776 = LINE ( 'NONE', #7312, #29519 ) ;
#37777 = CARTESIAN_POINT ( 'NONE',  ( 23.07151214508650128, 3.625915217019311583E-15, -1.699999999999999956 ) ) ;
#37778 = CARTESIAN_POINT ( 'NONE',  ( -31.52287095715006160, -23.47596703998600631, 11.44779298504229459 ) ) ;
#37779 = CARTESIAN_POINT ( 'NONE',  ( 12.47747183659840786, 15.48776231947736015, -1.500000000000002220 ) ) ;
#37780 = EDGE_CURVE ( 'NONE', #81663, #41697, #34751, .T. ) ;
#37781 = AXIS2_PLACEMENT_3D ( 'NONE', #50834, #43227, #81774 ) ;
#37782 = CARTESIAN_POINT ( 'NONE',  ( -118.6228709571500701, -23.48786465467241769, 11.44779295918253759 ) ) ;
#37783 = CARTESIAN_POINT ( 'NONE',  ( 19.51516567812286596, -3.327523070855789911, -1.500000000000002220 ) ) ;
#37784 = CARTESIAN_POINT ( 'NONE',  ( -56.63816017806102820, -24.15543982623907127, -0.2315651400026670359 ) ) ;
#37785 = EDGE_CURVE ( 'NONE', #71428, #35259, #26722, .T. ) ;
#37786 = CIRCLE ( 'NONE', #96100, 0.8160000000000008358 ) ;
#37787 = UNCERTAINTY_MEASURE_WITH_UNIT (LENGTH_MEASURE( 1.000000000000000082E-05 ), #19934, 'distance_accuracy_value', 'NONE');
#37788 = CARTESIAN_POINT ( 'NONE',  ( -39.04979701406145409, -25.10925853515279016, 4.033764255176815361 ) ) ;
#37789 = CARTESIAN_POINT ( 'NONE',  ( -1.595974963000059477, -6.376774720514408301, 19.39236848396478408 ) ) ;
#37790 = CARTESIAN_POINT ( 'NONE',  ( -14.43086120294938368, -14.79396848081076854, 11.49999999999999645 ) ) ;
#37791 = CARTESIAN_POINT ( 'NONE',  ( -56.52287095715005449, -23.47593901973090169, -1.443836447538996870 ) ) ;
#37792 = CARTESIAN_POINT ( 'NONE',  ( -49.86018645952977835, -25.31439301394160779, 5.308912529311577977 ) ) ;
#37793 = CARTESIAN_POINT ( 'NONE',  ( 22.03932947713327906, 5.445304565557160359, 11.49999999999999645 ) ) ;
#37794 = B_SPLINE_CURVE_WITH_KNOTS ( 'NONE', 3,
 ( #42235, #64074, #88385, #33596, #73167, #47823, #79257, #56951, #64576, #25980, #86380, #9247, #40709, #72666, #10763, #40208, #94989, #71163 ),
 .UNSPECIFIED., .F., .F.,
 ( 4, 2, 2, 2, 2, 2, 2, 2, 4 ),
 ( 8.673617379884035472E-19, 0.0002908379182062560990, 0.0005816758364125113306, 0.0008725137546187665622, 0.001163351672825021794, 0.001454189591031277134, 0.001745027509237532257, 0.002035865427443787380, 0.002326703345650042720 ),
 .UNSPECIFIED. ) ;
#37795 = ORIENTED_EDGE ( 'NONE', *, *, #100, .F. ) ;
#37796 = CARTESIAN_POINT ( 'NONE',  ( -2.794871794871791604, -5.876774720514426953, 21.75000000000001066 ) ) ;
#37797 = CARTESIAN_POINT ( 'NONE',  ( -69.84645531399800689, -25.14135604393685952, 6.994270796255325884 ) ) ;
#37798 = B_SPLINE_CURVE_WITH_KNOTS ( 'NONE', 3,
 ( #97547, #35662, #29028, #20405 ),
 .UNSPECIFIED., .F., .F.,
 ( 4, 4 ),
 ( 0.000000000000000000, 9.999999999998900014E-05 ),
 .UNSPECIFIED. ) ;
#37799 = CARTESIAN_POINT ( 'NONE',  ( -20.16912494768211417, -0.3064379698199363733, -1.500000000000002220 ) ) ;
#37800 = CARTESIAN_POINT ( 'NONE',  ( -63.60362512743664354, -23.73766607897669090, -1.055555164236456900 ) ) ;
#37801 = PLANE ( 'NONE',  #20444 ) ;
#37802 = VERTEX_POINT ( 'NONE', #35754 ) ;
#37803 = VERTEX_POINT ( 'NONE', #58588 ) ;
#37804 = CARTESIAN_POINT ( 'NONE',  ( 0.2428503871269292180, -6.376774720514413630, 19.85590024959437017 ) ) ;
#37805 = CARTESIAN_POINT ( 'NONE',  ( 21.75204538223844963, -7.182240389990739438, 11.49999999999998934 ) ) ;
#37806 = FACE_OUTER_BOUND ( 'NONE', #10023, .T. ) ;
#37807 = CARTESIAN_POINT ( 'NONE',  ( -16.54959454218438708, 13.92943311328891554, -1.500000000000002220 ) ) ;
#37808 = DIRECTION ( 'NONE',  ( 0.000000000000000000, 0.9999999999976377785, 2.173523156925979975E-06 ) ) ;
#37809 = CARTESIAN_POINT ( 'NONE',  ( -43.62287095715004881, -29.50250243563736774, 8.947779886222148704 ) ) ;
#37810 = CARTESIAN_POINT ( 'NONE',  ( -20.92377055399060737, -0.003182555231893603818, 11.49999999999999645 ) ) ;
#37811 = VERTEX_POINT ( 'NONE', #66724 ) ;
#37812 = CARTESIAN_POINT ( 'NONE',  ( -124.5557939318219667, -23.96119346886880663, -0.6495511937832024740 ) ) ;
#37813 = CARTESIAN_POINT ( 'NONE',  ( -19.13726171168348245, 10.91495894028074432, 11.49999999999998934 ) ) ;
#37814 = CARTESIAN_POINT ( 'NONE',  ( -105.5894839524365239, -24.52399227489126687, 9.353111116836517525 ) ) ;
#37815 = CARTESIAN_POINT ( 'NONE',  ( -28.88518304243395818, -24.79700160504788542, 6.883447026959963466 ) ) ;
#37817 = ORIENTED_EDGE ( 'NONE', *, *, #66132, .T. ) ;
#37816 = ADVANCED_FACE ( 'NONE', ( #49993 ), #34257, .T. ) ;
#37818 = LINE ( 'NONE', #14969, #47586 ) ;
#37819 = CARTESIAN_POINT ( 'NONE',  ( -68.52287095715006160, -24.66019654487199730, 8.947790411086124607 ) ) ;
#37820 = ORIENTED_EDGE ( 'NONE', *, *, #49507, .F. ) ;
#37821 = CARTESIAN_POINT ( 'NONE',  ( -72.62362984840773095, -24.66019654487199730, 8.947790411086121054 ) ) ;
#37822 = VERTEX_POINT ( 'NONE', #57602 ) ;
#37823 = CIRCLE ( 'NONE', #16738, 0.8159999999999469900 ) ;
#37824 = VERTEX_POINT ( 'NONE', #50477 ) ;
#37825 = CARTESIAN_POINT ( 'NONE',  ( -71.58415216203414388, -24.51419770103159124, 9.386484678747166299 ) ) ;
#37826 = CARTESIAN_POINT ( 'NONE',  ( -117.5562042904833504, -24.64965694238575011, 8.947790433994191162 ) ) ;
#37827 = FACE_OUTER_BOUND ( 'NONE', #88202, .T. ) ;
#37828 = CARTESIAN_POINT ( 'NONE',  ( -4.979992623568794130, 19.86841884474198494, -1.500000000000002220 ) ) ;
#37829 = EDGE_LOOP ( 'NONE', ( #9486, #8134, #8771, #50419 ) ) ;
#37830 = CARTESIAN_POINT ( 'NONE',  ( -3.103301570662693187, -6.376774720514418959, 20.14409848895067512 ) ) ;
#37831 = CARTESIAN_POINT ( 'NONE',  ( 6.573941812937369455, 1.185825954564562440E-17, -0.2639660507643281639 ) ) ;
#37832 = DIRECTION ( 'NONE',  ( 0.000000000000000000, -0.000000000000000000, -1.000000000000000000 ) ) ;
#37833 = CARTESIAN_POINT ( 'NONE',  ( 16.16129659511371131, 15.28805624652528472, -1.500000000000002220 ) ) ;
#37834 = CARTESIAN_POINT ( 'NONE',  ( -27.96875734969026084, 6.143225279485574397, 24.50402280011861933 ) ) ;
#37835 = DIRECTION ( 'NONE',  ( -3.773278334453079618E-23, 0.9999999999976377785, 2.173523156925979975E-06 ) ) ;
#37836 = EDGE_LOOP ( 'NONE', ( #48345, #40641, #91128, #41084 ) ) ;
#37837 = LINE ( 'NONE', #60194, #46794 ) ;
#37838 = CARTESIAN_POINT ( 'NONE',  ( -64.52287095715006160, -23.48786465467241769, 11.44779295918254824 ) ) ;
#37839 = CARTESIAN_POINT ( 'NONE',  ( 19.92439739378097840, -5.974006126113303949, -1.500000000000002220 ) ) ;
#37840 = ORIENTED_EDGE ( 'NONE', *, *, #73316, .F. ) ;
#37842 = VERTEX_POINT ( 'NONE', #4306 ) ;
#37841 = CARTESIAN_POINT ( 'NONE',  ( -42.52287095715005449, -24.66019654487199020, 8.947790411086133489 ) ) ;
#37843 = EDGE_CURVE ( 'NONE', #37096, #36594, #66224, .T. ) ;
#37844 = B_SPLINE_SURFACE_WITH_KNOTS ( 'NONE', 3, 1, ( 
 ( #79786, #55467 ),
 ( #2188, #71189 ),
 ( #2684, #47850 ),
 ( #10284, #41240 ),
 ( #26005, #78772 ),
 ( #9272, #40237 ),
 ( #74184, #81794 ),
 ( #66102, #49869 ),
 ( #35628, #89906 ),
 ( #34130, #57978 ),
 ( #88917, #3683 ) ),
 .UNSPECIFIED., .F., .F., .F.,
 ( 4, 1, 1, 1, 1, 1, 1, 1, 4 ),
 ( 2, 2 ),
 ( 0.000000000000000000, 0.1281581855276738569, 0.2536731361531681661, 0.3773253059734874015, 0.4993845547646074690, 0.6229183680423439062, 0.7458393931045753655, 0.8713952850140305184, 1.000000000000000000 ),
 ( 0.000000000000000000, 1.000000000000000000 ),
 .UNSPECIFIED. ) ;
#37845 = CARTESIAN_POINT ( 'NONE',  ( -31.58953762381672092, -24.65952944569304606, 1.056160979905695907 ) ) ;
#37846 = ORIENTED_EDGE ( 'NONE', *, *, #17308, .F. ) ;
#37847 = ORIENTED_EDGE ( 'NONE', *, *, #12411, .F. ) ;
#37848 = CARTESIAN_POINT ( 'NONE',  ( 7.160000000000000142, 10.80195425911416507, -0.9450485415980990345 ) ) ;
#37849 = DIRECTION ( 'NONE',  ( 0.000000000000000000, 0.000000000000000000, 1.000000000000000000 ) ) ;
#37850 = CARTESIAN_POINT ( 'NONE',  ( -116.4728709571500360, -25.30558663486635140, 5.000950659935019971 ) ) ;
#37851 = EDGE_CURVE ( 'NONE', #7232, #49833, #83489, .T. ) ;
#37852 = CARTESIAN_POINT ( 'NONE',  ( -115.5228709571500616, -29.50250243563736774, 8.947779886222134493 ) ) ;
#37853 = CARTESIAN_POINT ( 'NONE',  ( -108.9545715455114987, -25.28708312187852414, 4.170144817753115518 ) ) ;
#37854 = CARTESIAN_POINT ( 'NONE',  ( -95.58953762381672448, -23.47596703998600631, 11.44779298504227683 ) ) ;
#37856 = ORIENTED_EDGE ( 'NONE', *, *, #92509, .T. ) ;
#37855 = CARTESIAN_POINT ( 'NONE',  ( 22.15222936869060177, 0.07132910108538677296, 11.49999999999999645 ) ) ;
#37857 = CARTESIAN_POINT ( 'NONE',  ( -91.94687923781920347, -25.22391124735684187, 6.409327647371628522 ) ) ;
#37858 = CARTESIAN_POINT ( 'NONE',  ( -1.322449806865925614, 22.60218017400935864, -1.500000000000002220 ) ) ;
#37859 = EDGE_CURVE ( 'NONE', #76045, #79539, #8571, .T. ) ;
#37860 = EDGE_CURVE ( 'NONE', #1763, #24851, #60440, .T. ) ;
#37861 = ADVANCED_FACE ( 'NONE', ( #68913 ), #84631, .F. ) ;
#37863 = VERTEX_POINT ( 'NONE', #77508 ) ;
#37862 = CARTESIAN_POINT ( 'NONE',  ( -87.62287095715004170, -23.47593901973091235, -1.443836447539002865 ) ) ;
#37864 = AXIS2_PLACEMENT_3D ( 'NONE', #21259, #52233, #75544 ) ;
#37865 = EDGE_LOOP ( 'NONE', ( #34580, #77113, #89237, #72482, #13759, #66104, #12871, #72593, #88000, #99628, #49544, #84903, #45343, #97960, #9865 ) ) ;
#37866 = EDGE_CURVE ( 'NONE', #11694, #18999, #23729, .T. ) ;
#37867 = CARTESIAN_POINT ( 'NONE',  ( -113.5228709571500616, -23.47596703998600631, 11.44779298504228038 ) ) ;
#37868 = CARTESIAN_POINT ( 'NONE',  ( -19.68739882612603864, 4.164723872966736629, -1.500000000000002220 ) ) ;
#37869 = CARTESIAN_POINT ( 'NONE',  ( -99.62287095715005592, -23.47596703998600631, 11.44779298504227860 ) ) ;
#37870 = ORIENTED_EDGE ( 'NONE', *, *, #74880, .F. ) ;
#37871 = CARTESIAN_POINT ( 'NONE',  ( -6.499999999999992895, -1.301042606982604926E-15, 4.499999999999999112 ) ) ;
#37872 = CARTESIAN_POINT ( 'NONE',  ( -10.28394192611005842, 19.82837715243953625, -1.500000000000002220 ) ) ;
#37873 = EDGE_CURVE ( 'NONE', #97847, #38686, #65612, .T. ) ;
#37874 = ADVANCED_FACE ( 'NONE', ( #14114 ), #84130, .F. ) ;
#37875 = ORIENTED_EDGE ( 'NONE', *, *, #65861, .T. ) ;
#37876 = EDGE_LOOP ( 'NONE', ( #61491, #15411, #47408, #22841 ) ) ;
#37877 = LINE ( 'NONE', #22131, #20645 ) ;
#37878 = CARTESIAN_POINT ( 'NONE',  ( -119.5562042904834072, -23.48786465467241769, 11.44779295918253759 ) ) ;
#37879 = CARTESIAN_POINT ( 'NONE',  ( -80.53842267555941703, -25.29579208320836869, 4.514328772014316371 ) ) ;
#37880 = DIRECTION ( 'NONE',  ( 1.000000000000000000, 3.773278334444166432E-23, 8.201307841325785021E-29 ) ) ;
#37881 = DIRECTION ( 'NONE',  ( 0.8219392559241307517, 0.5637660281018075370, -0.08114015731558690825 ) ) ;
#37882 = CARTESIAN_POINT ( 'NONE',  ( 17.37147561666312257, 8.948746033654231269, 11.49999999999998934 ) ) ;
#37883 = FACE_OUTER_BOUND ( 'NONE', #70910, .T. ) ;
#37884 = CARTESIAN_POINT ( 'NONE',  ( -5.860608850286626925, 20.67097946995454905, 11.49999999999998934 ) ) ;
#37885 = CARTESIAN_POINT ( 'NONE',  ( -25.89225704477708589, -24.57999767617803855, 2.873802903271038822 ) ) ;
#37886 = DIRECTION ( 'NONE',  ( -3.773278334444166432E-23, 1.000000000000000000, 0.000000000000000000 ) ) ;
#37887 = CARTESIAN_POINT ( 'NONE',  ( -64.62287095715007013, -23.47596703998600631, 11.44779298504227683 ) ) ;
#37888 = CARTESIAN_POINT ( 'NONE',  ( -16.32851894532483783, 16.03542138455653898, -1.500000000000002220 ) ) ;
#37889 = EDGE_CURVE ( 'NONE', #95525, #31584, #31301, .T. ) ;
#37890 = VECTOR ( 'NONE', #35895, 1000.000000000000000 ) ;
#37891 = APPROVAL_STATUS ( 'not_yet_approved' ) ;
#37892 = CARTESIAN_POINT ( 'NONE',  ( -45.62287095715004881, -29.50248528299804818, 1.056150453629033370 ) ) ;
#37893 = FACE_OUTER_BOUND ( 'NONE', #20743, .T. ) ;
#37894 = CARTESIAN_POINT ( 'NONE',  ( 18.25133680241413359, 8.160682379734268466, 11.49999999999999645 ) ) ;
#37895 = DIRECTION ( 'NONE',  ( 0.000000000000000000, -0.9999999999976377785, -2.173523156925979128E-06 ) ) ;
#37896 = AXIS2_PLACEMENT_3D ( 'NONE', #47000, #15535, #93659 ) ;
#37897 = CARTESIAN_POINT ( 'NONE',  ( -74.52211788372726176, -23.48786465467241058, 11.44779295918254824 ) ) ;
#37898 = DIRECTION ( 'NONE',  ( -1.000000000000000000, -3.773278334444167020E-23, -8.201307838832447938E-29 ) ) ;
#37899 = VERTEX_POINT ( 'NONE', #14620 ) ;
#37900 = CARTESIAN_POINT ( 'NONE',  ( -83.52287095715007581, -23.96177878511310055, 10.65340807706330217 ) ) ;
#37901 = EDGE_CURVE ( 'NONE', #15617, #81766, #31350, .T. ) ;
#37902 = CARTESIAN_POINT ( 'NONE',  ( 18.07971092720299922, 12.08445254275838465, 11.49999999999998934 ) ) ;
#37903 = CARTESIAN_POINT ( 'NONE',  ( -56.62287095715005592, -23.73934037231757443, 11.05740245334328797 ) ) ;
#37904 = CARTESIAN_POINT ( 'NONE',  ( 2.036066721924049805, 19.47704226162102614, -1.500000000000002220 ) ) ;
#37905 = FACE_OUTER_BOUND ( 'NONE', #54821, .T. ) ;
#37906 = EDGE_CURVE ( 'NONE', #12577, #64113, #6517, .T. ) ;
#37907 = EDGE_CURVE ( 'NONE', #93232, #26341, #92242, .T. ) ;
#37908 = ITEM_DEFINED_TRANSFORMATION ( 'NONE', 'NONE', #76329,  #37391 ) ;
#37909 = CARTESIAN_POINT ( 'NONE',  ( -104.6228709571500559, -23.47593901973091235, -1.443836447539001089 ) ) ;
#37910 = DIRECTION ( 'NONE',  ( 1.000000000000000000, 4.218088402344531063E-15, 0.000000000000000000 ) ) ;
#37911 = CARTESIAN_POINT ( 'NONE',  ( 3.385237411341575964, -20.22741857368478335, 11.49999999999999645 ) ) ;
#37912 = DIRECTION ( 'NONE',  ( -1.000000000000000000, 0.000000000000000000, -0.000000000000000000 ) ) ;
#37913 = B_SPLINE_CURVE_WITH_KNOTS ( 'NONE', 3,
 ( #40631, #63484, #2570, #33511 ),
 .UNSPECIFIED., .F., .F.,
 ( 4, 4 ),
 ( 0.000000000000000000, 9.999999999999592548E-05 ),
 .UNSPECIFIED. ) ;
#37914 = CARTESIAN_POINT ( 'NONE',  ( 29.73860345376319003, -5.356774720514425603, -4.021180035027960287 ) ) ;
#37915 = EDGE_CURVE ( 'NONE', #90366, #77603, #39467, .T. ) ;
#37916 = ORIENTED_EDGE ( 'NONE', *, *, #1565, .T. ) ;
#37917 = CARTESIAN_POINT ( 'NONE',  ( -30.47287095715007510, -23.47596703474403768, 11.44538124590455830 ) ) ;
#37918 = DIRECTION ( 'NONE',  ( 0.000000000000000000, -0.000000000000000000, 1.000000000000000000 ) ) ;
#37919 = CARTESIAN_POINT ( 'NONE',  ( -125.5899142108936672, -24.40133493613050675, 9.663955038902798833 ) ) ;
#37920 = FACE_OUTER_BOUND ( 'NONE', #32128, .T. ) ;
#37921 = LINE ( 'NONE', #60276, #43563 ) ;
#37922 = CARTESIAN_POINT ( 'NONE',  ( -42.62287095715006302, -23.47596703998600276, 11.44779298504227505 ) ) ;
#37923 = CARTESIAN_POINT ( 'NONE',  ( 6.753845092018655016, 22.03294598498517232, 11.49999999999999645 ) ) ;
#37924 = CARTESIAN_POINT ( 'NONE',  ( -7.756741253720922380, -21.46081514045699024, 11.49999999999998934 ) ) ;
#37925 = CARTESIAN_POINT ( 'NONE',  ( -29.52287095715007581, -24.57618165405973087, 1.056161296257514870 ) ) ;
#37926 = AXIS2_PLACEMENT_3D ( 'NONE', #3272, #43813, #12350 ) ;
#37927 = CARTESIAN_POINT ( 'NONE',  ( -5.530932042872791499, -6.376774720514408301, 19.30497968945844534 ) ) ;
#37928 = CARTESIAN_POINT ( 'NONE',  ( -57.52287095715005449, -24.50216790748204687, 0.6166512839542507285 ) ) ;
#37929 = CARTESIAN_POINT ( 'NONE',  ( -40.52287095715007581, -24.63345952396255356, 9.038047939301511846 ) ) ;
#37930 = CARTESIAN_POINT ( 'NONE',  ( -110.5501846981437239, -24.73486907724917572, 1.287355809206965240 ) ) ;
#37931 = CARTESIAN_POINT ( 'NONE',  ( 21.14253370195585546, 5.708146584608840612, 11.49999999999998934 ) ) ;
#37932 = CARTESIAN_POINT ( 'NONE',  ( -38.52287095715006870, -24.66019654487199730, 8.947790411086121054 ) ) ;
#37933 = CARTESIAN_POINT ( 'NONE',  ( -87.56249327518180792, -23.48786465467240703, 11.44779295918254647 ) ) ;
#37934 = CARTESIAN_POINT ( 'NONE',  ( 9.940598223437573822, -5.876774720514426953, 18.21871304725684837 ) ) ;
#37935 = CARTESIAN_POINT ( 'NONE',  ( -36.52287095715006870, -29.50250786944525672, 11.44777988621624232 ) ) ;
#37936 = CARTESIAN_POINT ( 'NONE',  ( -115.5228709571500616, -29.50247984919015209, -1.443849546365046699 ) ) ;
#37937 = ORIENTED_EDGE ( 'NONE', *, *, #34815, .T. ) ;
#37938 = CARTESIAN_POINT ( 'NONE',  ( 5.749347661499963458, 19.61174949527739386, 11.49999999999998934 ) ) ;
#37939 = ORIENTED_EDGE ( 'NONE', *, *, #70538, .F. ) ;
#37940 = VERTEX_POINT ( 'NONE', #61816 ) ;
#37941 = EDGE_LOOP ( 'NONE', ( #48731, #9658, #90618, #49326 ) ) ;
#37942 = ORIENTED_EDGE ( 'NONE', *, *, #32636, .F. ) ;
#37943 = CARTESIAN_POINT ( 'NONE',  ( 11.92049557817732364, -19.74369927386287671, 11.49999999999998934 ) ) ;
#37944 = CARTESIAN_POINT ( 'NONE',  ( -61.54325905924635265, -24.34968618360933945, 0.1864209137778810865 ) ) ;
#37945 = CARTESIAN_POINT ( 'NONE',  ( -0.5548696950099620828, -20.20177982057877841, -1.500000000000002220 ) ) ;
#37946 = ORIENTED_EDGE ( 'NONE', *, *, #82767, .F. ) ;
#37947 = CARTESIAN_POINT ( 'NONE',  ( -27.14406549058544726, -24.94612812924882661, 6.759032221908315208 ) ) ;
#37948 = CARTESIAN_POINT ( 'NONE',  ( -29.49875734969025842, 5.965225279485572685, 23.37402280011862743 ) ) ;
#37949 = B_SPLINE_CURVE_WITH_KNOTS ( 'NONE', 3,
 ( #61048, #132, #85361, #91980, #52433, #37696 ),
 .UNSPECIFIED., .F., .F.,
 ( 4, 2, 4 ),
 ( 0.000000000000000000, 0.001380901958385383124, 0.002761803916770766247 ),
 .UNSPECIFIED. ) ;
#37950 = FACE_OUTER_BOUND ( 'NONE', #46448, .T. ) ;
#37951 = CARTESIAN_POINT ( 'NONE',  ( -70.63481881909494575, -24.52300882791528380, 0.6510814631126248253 ) ) ;
#37953 = ORIENTED_EDGE ( 'NONE', *, *, #78761, .T. ) ;
#37952 = CARTESIAN_POINT ( 'NONE',  ( 1.049947104896167049, -21.43676768134831434, 11.49999999999999645 ) ) ;
#37954 = CARTESIAN_POINT ( 'NONE',  ( -113.6228709571500275, -24.33832256526968862, 0.1851278514119947260 ) ) ;
#37955 = CARTESIAN_POINT ( 'NONE',  ( -111.2228709571500502, -23.47593901973090524, -1.443836447538996426 ) ) ;
#37956 = B_SPLINE_CURVE_WITH_KNOTS ( 'NONE', 3,
 ( #67219, #5796, #74316, #59599 ),
 .UNSPECIFIED., .F., .F.,
 ( 4, 4 ),
 ( 0.000000000000000000, 9.999999999997510880E-05 ),
 .UNSPECIFIED. ) ;
#37957 = ORIENTED_EDGE ( 'NONE', *, *, #51660, .T. ) ;
#37958 = CARTESIAN_POINT ( 'NONE',  ( 18.07348078632662691, -10.09602009226539288, 11.49999999999998934 ) ) ;
#37959 = ORIENTED_EDGE ( 'NONE', *, *, #98468, .F. ) ;
#37961 = ORIENTED_EDGE ( 'NONE', *, *, #56811, .T. ) ;
#37960 = CARTESIAN_POINT ( 'NONE',  ( -123.6228709571500559, -24.65952944569304961, 1.056160979905703234 ) ) ;
#37962 = EDGE_CURVE ( 'NONE', #22769, #22324, #83631, .T. ) ;
#37963 = CARTESIAN_POINT ( 'NONE',  ( 15.30859874843628354, -3.492299066144916697, -27.16052374892713317 ) ) ;
#37964 = ORIENTED_EDGE ( 'NONE', *, *, #35921, .F. ) ;
#37965 = ADVANCED_FACE ( 'NONE', ( #7013 ), #29346, .T. ) ;
#37966 = CARTESIAN_POINT ( 'NONE',  ( 4.334227700317904386, -6.376774720514402972, 18.30971318885719157 ) ) ;
#37967 = EDGE_CURVE ( 'NONE', #9703, #93197, #70439, .T. ) ;
#37968 = CARTESIAN_POINT ( 'NONE',  ( -65.57896445802249730, -24.92564183028979130, 1.928384488918254869 ) ) ;
#37969 = CARTESIAN_POINT ( 'NONE',  ( 5.346615758220810477, 21.33151429383102382, 11.49999999999999645 ) ) ;
#37970 = EDGE_CURVE ( 'NONE', #37842, #22614, #23222, .T. ) ;
#37971 = PLANE ( 'NONE',  #5825 ) ;
#37972 = CARTESIAN_POINT ( 'NONE',  ( 17.82461400791848405, -13.82690402418615960, 11.49999999999998934 ) ) ;
#37973 = EDGE_CURVE ( 'NONE', #64840, #26207, #22219, .T. ) ;
#37974 = CARTESIAN_POINT ( 'NONE',  ( -18.73635099073748833, 9.434554061794083069, -1.500000000000002220 ) ) ;
#37975 = CARTESIAN_POINT ( 'NONE',  ( -109.8650237084402619, -25.29042187987247914, 5.784623108531866897 ) ) ;
#37976 = EDGE_CURVE ( 'NONE', #76909, #79516, #19567, .T. ) ;
#37977 = LINE ( 'NONE', #52210, #11922 ) ;
#37978 = ORIENTED_EDGE ( 'NONE', *, *, #80306, .F. ) ;
#37979 = ORIENTED_EDGE ( 'NONE', *, *, #83260, .F. ) ;
#37980 = ADVANCED_FACE ( 'NONE', ( #69415 ), #92736, .F. ) ;
#37981 = VERTEX_POINT ( 'NONE', #26243 ) ;
#37982 = CARTESIAN_POINT ( 'NONE',  ( -88.52287095715006160, -23.47596703998600631, 11.44779298504228393 ) ) ;
#37983 = VECTOR ( 'NONE', #42302, 999.9999999999998863 ) ;
#37984 = CARTESIAN_POINT ( 'NONE',  ( -21.46803524902295024, 1.580295693706654347, -1.500000000000002220 ) ) ;
#37985 = B_SPLINE_CURVE_WITH_KNOTS ( 'NONE', 3,
 ( #97114, #38193, #16357, #31080, #84872, #99580, #92977, #38695 ),
 .UNSPECIFIED., .F., .F.,
 ( 4, 2, 2, 4 ),
 ( 0.000000000000000000, 0.002001098010032681049, 0.003001647015049021573, 0.004002196020065362098 ),
 .UNSPECIFIED. ) ;
#37986 = DIRECTION ( 'NONE',  ( -0.9951627101165076983, 0.000000000000000000, 0.09824042138329588947 ) ) ;
#37987 = ORIENTED_EDGE ( 'NONE', *, *, #39273, .T. ) ;
#37988 = CARTESIAN_POINT ( 'NONE',  ( -15.95541298346445735, 13.85296639876547076, -1.500000000000002220 ) ) ;
#37989 = DIRECTION ( 'NONE',  ( -0.000000000000000000, 1.000000000000000000, -0.000000000000000000 ) ) ;
#37990 = CARTESIAN_POINT ( 'NONE',  ( -64.53586813036071135, -24.65952944569304250, 1.056160979905695685 ) ) ;
#37991 = CARTESIAN_POINT ( 'NONE',  ( -50.28147435909711049, -25.30259094565539257, 4.732480668705053795 ) ) ;
#37992 = PLANE ( 'NONE',  #15151 ) ;
#37993 = CARTESIAN_POINT ( 'NONE',  ( -1.174900045708346497, -5.876774720514411854, 19.48569229636960998 ) ) ;
#37994 = CARTESIAN_POINT ( 'NONE',  ( -2.513997614918375589, -22.02279109229760223, -1.500000000000002220 ) ) ;
#37995 = CARTESIAN_POINT ( 'NONE',  ( -114.6307832717401851, -23.48783264082478794, -1.443836473390062380 ) ) ;
#37996 = EDGE_CURVE ( 'NONE', #50697, #22271, #33853, .T. ) ;
#37997 = AXIS2_PLACEMENT_3D ( 'NONE', #24834, #48190, #94848 ) ;
#37998 = VERTEX_POINT ( 'NONE', #93740 ) ;
#37999 = CARTESIAN_POINT ( 'NONE',  ( -51.15602047325173629, -25.31633097224522189, 4.998862860385179907 ) ) ;
#38000 = CARTESIAN_POINT ( 'NONE',  ( 0.000000000000000000, -0.3849999999999936806, -1.530000000000001359 ) ) ;
#38001 = CARTESIAN_POINT ( 'NONE',  ( -83.62287095715005592, -23.47593901973091235, -1.443836447539004642 ) ) ;
#38002 = FACE_OUTER_BOUND ( 'NONE', #59508, .T. ) ;
#38003 = ADVANCED_FACE ( 'NONE', ( #2922 ), #2835, .T. ) ;
#38004 = CARTESIAN_POINT ( 'NONE',  ( 12.19879910451502703, -15.15100395215988449, -1.500000000000002220 ) ) ;
#38005 = CARTESIAN_POINT ( 'NONE',  ( -17.20161093224466953, -12.68000408521323408, 11.49999999999998934 ) ) ;
#38006 = CYLINDRICAL_SURFACE ( 'NONE', #17478, 91.74549126261076992 ) ;
#38007 = CARTESIAN_POINT ( 'NONE',  ( -124.5228709571500616, -24.64965694238575722, 8.947790433994191162 ) ) ;
#38008 = DIRECTION ( 'NONE',  ( 0.000000000000000000, -1.000000000000000000, 1.571307496355802463E-16 ) ) ;
#38009 = DIRECTION ( 'NONE',  ( -0.000000000000000000, -1.000000000000000000, -0.000000000000000000 ) ) ;
#38010 = CARTESIAN_POINT ( 'NONE',  ( -4.086358941109507370, -22.34742993483353146, -1.500000000000002220 ) ) ;
#38011 = EDGE_LOOP ( 'NONE', ( #69673, #3326, #43578, #70918 ) ) ;
#38012 = CARTESIAN_POINT ( 'NONE',  ( -58.52287095715006160, -24.64965694238407323, 8.947790433994201820 ) ) ;
#38013 = CARTESIAN_POINT ( 'NONE',  ( -57.62287095715001328, -24.35013146730203459, 9.818937971375111928 ) ) ;
#38014 = CARTESIAN_POINT ( 'NONE',  ( -10.52764212615999639, 16.74383705166681580, 11.49999999999999645 ) ) ;
#38015 = CARTESIAN_POINT ( 'NONE',  ( -117.5228709571500758, -29.50248528299804818, 1.056150453629045360 ) ) ;
#38016 = EDGE_LOOP ( 'NONE', ( #89741, #15947, #89625, #70532 ) ) ;
#38017 = CARTESIAN_POINT ( 'NONE',  ( -48.62287095715004881, -23.48783264082478439, -1.443836473390070596 ) ) ;
#38018 = CARTESIAN_POINT ( 'NONE',  ( -87.52287095715006160, -23.47596703998600631, 11.44779298504228393 ) ) ;
#38019 = CARTESIAN_POINT ( 'NONE',  ( 19.51036611237648088, 9.378288983258578071, -1.500000000000002220 ) ) ;
#38020 = CARTESIAN_POINT ( 'NONE',  ( -45.52287095715004739, -23.48783264082477018, -1.443836473390097019 ) ) ;
#38021 = CARTESIAN_POINT ( 'NONE',  ( 15.36829964806744364, -11.83880051060199712, -1.500000000000002220 ) ) ;
#38022 = CARTESIAN_POINT ( 'NONE',  ( -82.52287095715007581, -23.96177878511308634, 10.65340807706329862 ) ) ;
#38023 = DIRECTION ( 'NONE',  ( -1.000000000000000000, -0.000000000000000000, -0.000000000000000000 ) ) ;
#38024 = EDGE_CURVE ( 'NONE', #81873, #83477, #32348, .T. ) ;
#38025 = CARTESIAN_POINT ( 'NONE',  ( 19.71268880909926580, -1.816447362451163450, 11.49999999999998934 ) ) ;
#38026 = ORIENTED_EDGE ( 'NONE', *, *, #38290, .F. ) ;
#38027 = AXIS2_PLACEMENT_3D ( 'NONE', #40022, #25795, #86193 ) ;
#38028 = CARTESIAN_POINT ( 'NONE',  ( 9.809556900635294951, 17.81656380412256269, 11.49999999999999645 ) ) ;
#38029 = CARTESIAN_POINT ( 'NONE',  ( -118.5228709571500758, -29.50250786944525672, 11.44777988621622811 ) ) ;
#38030 = EDGE_CURVE ( 'NONE', #32620, #11368, #86637, .T. ) ;
#38031 = CARTESIAN_POINT ( 'NONE',  ( 33.69795529655567634, 5.515143950957555496, 14.99689261510125249 ) ) ;
#38032 = VERTEX_POINT ( 'NONE', #1914 ) ;
#38033 = B_SPLINE_SURFACE_WITH_KNOTS ( 'NONE', 3, 3, ( 
 ( #45454, #76859, #45948, #23073 ),
 ( #37338, #37825, #84493, #77862 ),
 ( #21585, #68778, #52557, #54064 ),
 ( #29713, #7360, #84988, #7866 ),
 ( #8369, #92595, #62675, #99696 ),
 ( #46434, #30200, #62172, #69273 ),
 ( #93095, #23578, #54548, #92104 ) ),
 .UNSPECIFIED., .F., .F., .F.,
 ( 4, 3, 4 ),
 ( 4, 4 ),
 ( 0.7945040050992235869, 0.8970133687736498995, 0.9995227324480762121 ),
 ( 0.5896438339135527951, 0.5909287771905322728 ),
 .UNSPECIFIED. ) ;
#38034 = CARTESIAN_POINT ( 'NONE',  ( -30.59800378598952264, -24.75991027412950274, 1.063373454495736947 ) ) ;
#38035 = CARTESIAN_POINT ( 'NONE',  ( -119.4728709571500502, -25.21147115889350587, 5.000950862241205996 ) ) ;
#38036 = LINE ( 'NONE', #31425, #49969 ) ;
#38037 = CARTESIAN_POINT ( 'NONE',  ( -7.160000000000000142, 7.891155995661682354, 5.788828319098143993 ) ) ;
#38038 = CARTESIAN_POINT ( 'NONE',  ( -127.6228709571500559, -24.50321055353805377, 9.387540953477520489 ) ) ;
#38039 = CARTESIAN_POINT ( 'NONE',  ( -16.07871291144651593, -12.00523380332558965, 11.49999999999998934 ) ) ;
#38040 = CARTESIAN_POINT ( 'NONE',  ( -109.6228709571500417, -23.48786465467242124, 11.44779295918253936 ) ) ;
#38041 = ORIENTED_EDGE ( 'NONE', *, *, #78084, .T. ) ;
#38042 = CYLINDRICAL_SURFACE ( 'NONE', #64165, 2.349999999999999645 ) ;
#38043 = CARTESIAN_POINT ( 'NONE',  ( -12.73177969873712279, -19.06072230859735939, 11.49999999999999645 ) ) ;
#38044 = CARTESIAN_POINT ( 'NONE',  ( -14.94938274637043207, -17.11189489004485864, 11.49999999999998934 ) ) ;
#38045 = CARTESIAN_POINT ( 'NONE',  ( 32.60294298177596062, -6.376774720514426953, -11.48871326860665043 ) ) ;
#38046 = CARTESIAN_POINT ( 'NONE',  ( -29.62287095715004881, -29.50248298729119867, -6.412432996800796609E-05 ) ) ;
#38047 = CARTESIAN_POINT ( 'NONE',  ( -38.61777322412189051, -23.48786465467240347, 11.44779295918255002 ) ) ;
#38048 = CARTESIAN_POINT ( 'NONE',  ( 8.971512145086530055, -9.528487854913503696, -4.499999999999998224 ) ) ;
#38049 = VECTOR ( 'NONE', #22416, 1000.000000000000000 ) ;
#38050 = CARTESIAN_POINT ( 'NONE',  ( -4.568292318365942073, 0.3587747205144265483, 30.06720597538392425 ) ) ;
#38051 = CARTESIAN_POINT ( 'NONE',  ( 26.73860345374794178, -1.682774720514426114, -1.272392034746785860 ) ) ;
#38052 = ORIENTED_EDGE ( 'NONE', *, *, #64244, .T. ) ;
#38053 = CARTESIAN_POINT ( 'NONE',  ( 8.194921280291850962, -18.63391395107102610, 11.49999999999998934 ) ) ;
#38054 = ORIENTED_EDGE ( 'NONE', *, *, #35140, .F. ) ;
#38055 = CARTESIAN_POINT ( 'NONE',  ( -18.50152239663938403, 13.63810111590111163, -1.500000000000002220 ) ) ;
#38056 = CARTESIAN_POINT ( 'NONE',  ( -53.52287095715004739, -24.35013146730203815, 9.818937971375104823 ) ) ;
#38057 = VECTOR ( 'NONE', #88505, 1000.000000000000000 ) ;
#38058 = VERTEX_POINT ( 'NONE', #63833 ) ;
#38059 = CARTESIAN_POINT ( 'NONE',  ( -101.6228709571500985, -23.95044443724992789, 10.65354141964649592 ) ) ;
#38060 = CARTESIAN_POINT ( 'NONE',  ( -77.50832112164282250, -24.15620529776628800, 10.23563542870659937 ) ) ;
#38061 = CARTESIAN_POINT ( 'NONE',  ( -40.62287095715004170, -24.99132157543083466, 2.256160258750667502 ) ) ;
#38063 = ORIENTED_EDGE ( 'NONE', *, *, #48818, .F. ) ;
#38062 = CARTESIAN_POINT ( 'NONE',  ( -12.14505723179402530, 17.47690347785001919, 11.49999999999999645 ) ) ;
#38064 = ORIENTED_EDGE ( 'NONE', *, *, #11411, .T. ) ;
#38065 = CARTESIAN_POINT ( 'NONE',  ( 19.86420646539740176, -9.926203236129387264, -1.500000000000002220 ) ) ;
#38066 = CARTESIAN_POINT ( 'NONE',  ( -3.146292006899429783, -20.37002610441940220, 11.49999999999998934 ) ) ;
#38067 = ORIENTED_EDGE ( 'NONE', *, *, #67253, .T. ) ;
#38068 = VERTEX_POINT ( 'NONE', #94746 ) ;
#38069 = EDGE_CURVE ( 'NONE', #90203, #94029, #267, .T. ) ;
#38070 = CARTESIAN_POINT ( 'NONE',  ( -109.0556427821970260, -25.27682694363410576, 4.716568693008002633 ) ) ;
#38071 = CARTESIAN_POINT ( 'NONE',  ( -121.6228709571500985, -24.51283580621365488, 0.6167428607019845854 ) ) ;
#38072 = ORIENTED_EDGE ( 'NONE', *, *, #83630, .T. ) ;
#38073 = EDGE_CURVE ( 'NONE', #68279, #37863, #31858, .T. ) ;
#38074 = DIRECTION ( 'NONE',  ( 0.000000000000000000, 0.000000000000000000, -1.000000000000000000 ) ) ;
#38075 = ORIENTED_EDGE ( 'NONE', *, *, #83781, .F. ) ;
#38076 = CARTESIAN_POINT ( 'NONE',  ( -39.52287095715006870, -23.47596703998600631, 11.44779298504229281 ) ) ;
#38077 = CARTESIAN_POINT ( 'NONE',  ( -35.58953762381672448, -23.48786465467240347, 11.44779295918255180 ) ) ;
#38078 = CARTESIAN_POINT ( 'NONE',  ( 20.75994597877129877, -1.272245555857973054, -1.500000000000002220 ) ) ;
#38079 = CARTESIAN_POINT ( 'NONE',  ( -5.167225684058948332, 21.16526716281445530, 11.49999999999999645 ) ) ;
#38080 = ADVANCED_FACE ( 'NONE', ( #59197 ), #20614, .F. ) ;
#38081 = CARTESIAN_POINT ( 'NONE',  ( -40.20787662131280626, -25.18822154510203148, 3.317274650640859690 ) ) ;
#38082 = CARTESIAN_POINT ( 'NONE',  ( -20.27875734969026311, -5.356774720514425603, 24.00402280011862288 ) ) ;
#38083 = CARTESIAN_POINT ( 'NONE',  ( -18.83616483605274539, -12.25834331966736102, 11.49999999999998934 ) ) ;
#38084 = ADVANCED_FACE ( 'NONE', ( #12010 ), #66824, .F. ) ;
#38085 = DIRECTION ( 'NONE',  ( -8.659560562354873694E-17, -0.7071067811865525687, -0.7071067811865425767 ) ) ;
#38086 = EDGE_LOOP ( 'NONE', ( #96112, #16299, #23420, #63737 ) ) ;
#38087 = CARTESIAN_POINT ( 'NONE',  ( -4.141025641025642301, -6.376774720514408301, 19.19230769230769695 ) ) ;
#38088 = CARTESIAN_POINT ( 'NONE',  ( -101.6814946224345704, -25.24282061761981311, 6.236250683194342059 ) ) ;
#38089 = EDGE_CURVE ( 'NONE', #89333, #63176, #5398, .T. ) ;
#38090 = VECTOR ( 'NONE', #22898, 1000.000000000000000 ) ;
#38091 = ORIENTED_EDGE ( 'NONE', *, *, #35448, .F. ) ;
#38092 = ADVANCED_FACE ( 'NONE', ( #89144 ), #19618, .T. ) ;
#38093 = ORIENTED_EDGE ( 'NONE', *, *, #55113, .T. ) ;
#38094 = ORIENTED_EDGE ( 'NONE', *, *, #10524, .T. ) ;
#38095 = CARTESIAN_POINT ( 'NONE',  ( -17.73838780825237649, 11.93509662624355450, -1.500000000000002220 ) ) ;
#38096 = ORIENTED_EDGE ( 'NONE', *, *, #79311, .T. ) ;
#38097 = CARTESIAN_POINT ( 'NONE',  ( -19.40065202112720755, 8.109199488025859992, 11.49999999999998934 ) ) ;
#38098 = CARTESIAN_POINT ( 'NONE',  ( -30.52453496278478084, -25.14632053279673585, 2.712646531854225440 ) ) ;
#38099 =( BOUNDED_CURVE ( )  B_SPLINE_CURVE ( 3, ( #30141, #14912, #6808, #74820 ),
 .UNSPECIFIED., .F., .F. ) 
 B_SPLINE_CURVE_WITH_KNOTS ( ( 4, 4 ),
 ( 1.570796326794896558, 1.674609638881183082 ),
 .UNSPECIFIED. ) 
 CURVE ( )  GEOMETRIC_REPRESENTATION_ITEM ( )  RATIONAL_B_SPLINE_CURVE ( ( 1.000000000000000000, 0.9991021013140741758, 0.9991021013140741758, 1.000000000000000000 ) ) 
 REPRESENTATION_ITEM ( '' )  );
#38100 = CARTESIAN_POINT ( 'NONE',  ( -110.3346797185884327, -25.19502912051678933, 3.293943094755625633 ) ) ;
#38101 = CARTESIAN_POINT ( 'NONE',  ( -65.52287095715009002, -23.84081130425358808, 10.88220057483157888 ) ) ;
#38102 = CARTESIAN_POINT ( 'NONE',  ( 21.52718982488130450, -4.553922534329950089, -1.500000000000002220 ) ) ;
#38103 = LINE ( 'NONE', #69057, #68986 ) ;
#38104 = ORIENTED_EDGE ( 'NONE', *, *, #66061, .F. ) ;
#38105 = CARTESIAN_POINT ( 'NONE',  ( -38.92287095715006018, -23.47593901973090524, -1.443836447538997980 ) ) ;
#38106 = FACE_OUTER_BOUND ( 'NONE', #36083, .T. ) ;
#38107 = LINE ( 'NONE', #99987, #60890 ) ;
#38108 = LINE ( 'NONE', #20882, #86202 ) ;
#38109 = CARTESIAN_POINT ( 'NONE',  ( -0.02085506613324685302, -22.78001478014107306, 7.291654623549817416 ) ) ;
#38110 = CARTESIAN_POINT ( 'NONE',  ( 19.49461108348020133, 8.573440864381753457, -1.500000000000002220 ) ) ;
#38111 = CARTESIAN_POINT ( 'NONE',  ( -98.55250113363597109, -24.15620529776628445, 10.23563542870660292 ) ) ;
#38112 = CARTESIAN_POINT ( 'NONE',  ( -107.5517401469810324, -24.35071581493543746, 9.817618358456021710 ) ) ;
#38113 = VECTOR ( 'NONE', #58779, 1000.000000000000114 ) ;
#38114 = CARTESIAN_POINT ( 'NONE',  ( 8.160000000000000142, -9.074990544709798712, -0.7360493640965781736 ) ) ;
#38115 = CARTESIAN_POINT ( 'NONE',  ( -33.58674611195124982, -24.34968618360933235, 0.1864209137778845560 ) ) ;
#38116 = CARTESIAN_POINT ( 'NONE',  ( 9.993301969596378953, 20.15287186522775542, -1.500000000000002220 ) ) ;
#38117 = CARTESIAN_POINT ( 'NONE',  ( -111.9710651877489767, -25.32390614315827193, 4.358500768180118889 ) ) ;
#38118 = VERTEX_POINT ( 'NONE', #81535 ) ;
#38119 = FACE_OUTER_BOUND ( 'NONE', #87911, .T. ) ;
#38120 = CARTESIAN_POINT ( 'NONE',  ( 10.60981200654714307, 16.52409317135366607, 11.49999999999999645 ) ) ;
#38121 = CARTESIAN_POINT ( 'NONE',  ( -125.6228709571500559, -24.92579138211019085, 1.929029949965666457 ) ) ;
#38122 = CARTESIAN_POINT ( 'NONE',  ( -82.52287095715006160, -24.65952944569304606, 1.056160979905698794 ) ) ;
#38123 = ORIENTED_EDGE ( 'NONE', *, *, #88571, .F. ) ;
#38124 = CIRCLE ( 'NONE', #94846, 8.452410033082760066 ) ;
#38125 = CARTESIAN_POINT ( 'NONE',  ( -88.51806219836213074, -23.73791477778912196, 11.05961554403170588 ) ) ;
#38126 = CARTESIAN_POINT ( 'NONE',  ( -127.2834360451832225, -25.38371582119480507, 5.756550691135934095 ) ) ;
#38127 = CARTESIAN_POINT ( 'NONE',  ( -100.4277023991755442, -25.31439536995993933, 5.215800341084221081 ) ) ;
#38128 = AXIS2_PLACEMENT_3D ( 'NONE', #2267, #34706, #41320 ) ;
#38129 = CARTESIAN_POINT ( 'NONE',  ( -10.60818629614422370, 16.63341085705455669, 11.49999999999998934 ) ) ;
#38130 = EDGE_LOOP ( 'NONE', ( #3699, #14245, #76773, #81199 ) ) ;
#38131 = CARTESIAN_POINT ( 'NONE',  ( 10.86431179149619908, 3.316774720514763075, -28.05678185015766246 ) ) ;
#38132 = DIRECTION ( 'NONE',  ( 0.000000000000000000, 0.000000000000000000, -1.000000000000000000 ) ) ;
#38133 = EDGE_CURVE ( 'NONE', #43478, #25854, #75045, .T. ) ;
#38134 = COORDINATED_UNIVERSAL_TIME_OFFSET ( 0, 0, .AHEAD. ) ;
#38135 = EDGE_CURVE ( 'NONE', #66793, #88329, #67307, .T. ) ;
#38136 = EDGE_LOOP ( 'NONE', ( #62421, #14184, #9506, #72626 ) ) ;
#38137 = CARTESIAN_POINT ( 'NONE',  ( -96.58953762381672448, -24.64898659630368272, 1.056161002820388273 ) ) ;
#38138 = PLANE ( 'NONE',  #31261 ) ;
#38139 = FACE_OUTER_BOUND ( 'NONE', #7525, .T. ) ;
#38140 = DIRECTION ( 'NONE',  ( -0.000000000000000000, -1.000000000000000000, -0.000000000000000000 ) ) ;
#38141 = CARTESIAN_POINT ( 'NONE',  ( -66.62287095715005592, -24.64965695001468404, 8.947790433994184056 ) ) ;
#38142 = CARTESIAN_POINT ( 'NONE',  ( 33.12653832968932477, -5.965225279485572685, -7.315055336576597789 ) ) ;
#38143 = CARTESIAN_POINT ( 'NONE',  ( -107.5116988131331084, -24.65952944569305316, 1.056160979905704789 ) ) ;
#38144 = CARTESIAN_POINT ( 'NONE',  ( -8.876215969300202957, 17.89991547088461488, -1.500000000000002220 ) ) ;
#38145 = CARTESIAN_POINT ( 'NONE',  ( -127.6228709571500559, -23.94994826722515668, -0.6494450866351666463 ) ) ;
#38146 = CARTESIAN_POINT ( 'NONE',  ( -45.52251258058822714, -25.00182538069146787, 7.747789668545044250 ) ) ;
#38147 = VERTEX_POINT ( 'NONE', #51083 ) ;
#38148 = CARTESIAN_POINT ( 'NONE',  ( -119.5539613361492144, -24.34968618360934656, 0.1864209137778924941 ) ) ;
#38149 = AXIS2_PLACEMENT_3D ( 'NONE', #30171, #69241, #61151 ) ;
#38150 = CARTESIAN_POINT ( 'NONE',  ( -80.54343777448522701, -24.63419186844610920, 9.035850630976922204 ) ) ;
#38151 = CARTESIAN_POINT ( 'NONE',  ( 29.73860345376316872, 5.356774720514427379, 17.30421508979850387 ) ) ;
#38152 = CARTESIAN_POINT ( 'NONE',  ( -108.5228709571500758, -23.94994826722565762, -0.6494450866342741380 ) ) ;
#38153 = CARTESIAN_POINT ( 'NONE',  ( 1.949999999999999956, 0.1925000000000007538, -0.1924999999999994493 ) ) ;
#38154 = EDGE_CURVE ( 'NONE', #92103, #91104, #28738, .T. ) ;
#38155 = CARTESIAN_POINT ( 'NONE',  ( -1.359786310227693251, -5.876774720514417183, 20.62654306927474579 ) ) ;
#38156 = CARTESIAN_POINT ( 'NONE',  ( -37.62287095715007723, -23.72773821059535493, 11.05748984161097503 ) ) ;
#38157 = CYLINDRICAL_SURFACE ( 'NONE', #30724, 2.499999999999998668 ) ;
#38158 = ORIENTED_EDGE ( 'NONE', *, *, #82355, .F. ) ;
#38159 = B_SPLINE_CURVE_WITH_KNOTS ( 'NONE', 3,
 ( #83542, #51611, #90661, #28767 ),
 .UNSPECIFIED., .F., .F.,
 ( 4, 4 ),
 ( 0.000000000000000000, 0.0001000000000000028644 ),
 .UNSPECIFIED. ) ;
#38160 = CARTESIAN_POINT ( 'NONE',  ( 0.7435384974594729801, 20.27106041150680937, -1.500000000000002220 ) ) ;
#38161 = CARTESIAN_POINT ( 'NONE',  ( -122.5195476943700186, -24.34968618360934300, 0.1864209137778895797 ) ) ;
#38162 = PLANE ( 'NONE',  #59856 ) ;
#38163 = DIRECTION ( 'NONE',  ( -3.773278334453079030E-23, 0.9999999999976377785, 2.173523156925979128E-06 ) ) ;
#38164 = VERTEX_POINT ( 'NONE', #42978 ) ;
#38165 = CARTESIAN_POINT ( 'NONE',  ( -73.62287095715005592, -29.50250786944525672, 11.44777988621623699 ) ) ;
#38166 = CARTESIAN_POINT ( 'NONE',  ( 13.10547390533899836, 15.29217475743441312, -1.500000000000002220 ) ) ;
#38167 = CARTESIAN_POINT ( 'NONE',  ( -14.29351441246084065, -15.47709782942846424, 11.49999999999999645 ) ) ;
#38168 = LINE ( 'NONE', #14331, #62846 ) ;
#38169 = CARTESIAN_POINT ( 'NONE',  ( 21.80885565983754404, 3.581153529568561478, 11.49999999999998934 ) ) ;
#38170 = CARTESIAN_POINT ( 'NONE',  ( 18.67943556539783856, 8.552475402716291697, 11.49999999999998934 ) ) ;
#38171 = CARTESIAN_POINT ( 'NONE',  ( -60.85008211737284256, -25.20813793428145289, 6.796440242136131182 ) ) ;
#38172 = VECTOR ( 'NONE', #73034, 1000.000000000000114 ) ;
#38173 = CARTESIAN_POINT ( 'NONE',  ( -60.50382013959431049, -24.15503026093916006, -0.2815557561904390993 ) ) ;
#38174 = ORIENTED_EDGE ( 'NONE', *, *, #84884, .T. ) ;
#38175 = LINE ( 'NONE', #28581, #10409 ) ;
#38176 = ORIENTED_EDGE ( 'NONE', *, *, #1587, .T. ) ;
#38177 = CARTESIAN_POINT ( 'NONE',  ( -5.970505764849975527, -6.376774720514411854, 19.55848054040323802 ) ) ;
#38178 = DIRECTION ( 'NONE',  ( -3.773278334444167608E-23, 1.000000000000000000, 0.000000000000000000 ) ) ;
#38179 = VERTEX_POINT ( 'NONE', #58201 ) ;
#38180 = VECTOR ( 'NONE', #3437, 999.9999999999998863 ) ;
#38181 = VERTEX_POINT ( 'NONE', #42489 ) ;
#38182 = VECTOR ( 'NONE', #85800, 1000.000000000000114 ) ;
#38183 = VERTEX_POINT ( 'NONE', #88648 ) ;
#38184 = FACE_OUTER_BOUND ( 'NONE', #54569, .T. ) ;
#38185 = CARTESIAN_POINT ( 'NONE',  ( -74.58953762381672448, -24.66019654487198665, 8.947790411086131712 ) ) ;
#38186 = CARTESIAN_POINT ( 'NONE',  ( -77.62287095715007013, -24.65952944569304606, 1.056160979905699016 ) ) ;
#38187 = CARTESIAN_POINT ( 'NONE',  ( -20.51892249978613236, 2.527598752449112585, -1.500000000000002220 ) ) ;
#38188 = VECTOR ( 'NONE', #37502, 1000.000000000000000 ) ;
#38189 = CARTESIAN_POINT ( 'NONE',  ( 14.26105141482337935, -16.23293960606763520, 11.49999999999999645 ) ) ;
#38190 = ORIENTED_EDGE ( 'NONE', *, *, #8865, .F. ) ;
#38191 = EDGE_CURVE ( 'NONE', #33057, #81742, #45871, .T. ) ;
#38192 = CARTESIAN_POINT ( 'NONE',  ( -81.62287095715004170, -24.66019654487199020, 8.947790411086131712 ) ) ;
#38193 = CARTESIAN_POINT ( 'NONE',  ( -60.62287095715005592, -23.84047902841601285, -0.8780736468305713194 ) ) ;
#38194 = CARTESIAN_POINT ( 'NONE',  ( -15.72835732567950195, 15.92727474065614501, 11.49999999999998934 ) ) ;
#38195 = AXIS2_PLACEMENT_3D ( 'NONE', #56328, #79633, #17237 ) ;
#38196 = ADVANCED_FACE ( 'NONE', ( #50579 ), #73912, .T. ) ;
#38197 = CARTESIAN_POINT ( 'NONE',  ( -62.52287095715006160, -23.96127896941631974, -0.6493128931038026908 ) ) ;
#38198 = DIRECTION ( 'NONE',  ( -1.000000000000000000, 0.000000000000000000, 0.000000000000000000 ) ) ;
#38199 = ORIENTED_EDGE ( 'NONE', *, *, #77398, .F. ) ;
#38200 = CARTESIAN_POINT ( 'NONE',  ( 32.85081302853786411, -5.152774720514582185, -13.10817780685225031 ) ) ;
#38201 = CARTESIAN_POINT ( 'NONE',  ( -35.46595863577746854, -25.00182538069146077, 7.747789668545035369 ) ) ;
#38202 = EDGE_CURVE ( 'NONE', #47437, #45447, #64354, .T. ) ;
#38203 = CARTESIAN_POINT ( 'NONE',  ( 32.66876533700882845, -5.965225279485572685, -12.58926540598385557 ) ) ;
#38204 = CARTESIAN_POINT ( 'NONE',  ( -18.75169668496848985, 9.291489096422434812, -1.500000000000002220 ) ) ;
#38205 = ADVANCED_FACE ( 'NONE', ( #28235 ), #84011, .T. ) ;
#38206 = VERTEX_POINT ( 'NONE', #25888 ) ;
#38208 = ORIENTED_EDGE ( 'NONE', *, *, #59194, .T. ) ;
#38207 = CARTESIAN_POINT ( 'NONE',  ( -67.54034052825554113, -24.51419770103159124, 9.386484678747168076 ) ) ;
#38209 = ORIENTED_EDGE ( 'NONE', *, *, #74673, .F. ) ;
#38210 = CARTESIAN_POINT ( 'NONE',  ( 13.91401389203221406, 6.376774720514426953, 158.0376437107427137 ) ) ;
#38211 = CARTESIAN_POINT ( 'NONE',  ( 15.93590435955092843, -13.91358336426615239, -1.500000000000002220 ) ) ;
#38212 = VERTEX_POINT ( 'NONE', #95895 ) ;
#38213 = CARTESIAN_POINT ( 'NONE',  ( -112.5228709571500332, -24.33927499327855770, 9.819080762295804732 ) ) ;
#38214 = CARTESIAN_POINT ( 'NONE',  ( -99.37409858214790859, -25.12215546412569012, 6.508817117250577766 ) ) ;
#38215 = CARTESIAN_POINT ( 'NONE',  ( -12.70408864715453667, 17.69581422525067183, 11.49999999999998934 ) ) ;
#38216 = CARTESIAN_POINT ( 'NONE',  ( -89.23534077628077910, -25.22391154813774605, 6.409327647370973935 ) ) ;
#38217 = CARTESIAN_POINT ( 'NONE',  ( -76.60618700539868087, -23.48786465467240703, 11.44779295918254647 ) ) ;
#38218 = CARTESIAN_POINT ( 'NONE',  ( 8.000000000000003553, -6.376774720514426953, 0.000000000000000000 ) ) ;
#38219 = CARTESIAN_POINT ( 'NONE',  ( 3.468383421097696928, -21.53508805063734854, -1.500000000000002220 ) ) ;
#38220 = CARTESIAN_POINT ( 'NONE',  ( -71.70841769935768184, -25.31639753719101549, 6.192981292503872304 ) ) ;
#38221 = ORIENTED_EDGE ( 'NONE', *, *, #83815, .F. ) ;
#38222 = EDGE_CURVE ( 'NONE', #31540, #2778, #94891, .T. ) ;
#38223 = DIRECTION ( 'NONE',  ( 1.000000000000000000, 3.773278334444165844E-23, 8.201307836089272790E-29 ) ) ;
#38224 = CARTESIAN_POINT ( 'NONE',  ( -72.55620429048340725, -24.65952944569304606, 1.056160979905698127 ) ) ;
#38225 = CARTESIAN_POINT ( 'NONE',  ( -43.62287095715004881, -23.47593901973091235, -1.443836447539011525 ) ) ;
#38226 = ORIENTED_EDGE ( 'NONE', *, *, #42824, .T. ) ;
#38227 = B_SPLINE_CURVE_WITH_KNOTS ( 'NONE', 3,
 ( #3294, #89503, #19987, #57076 ),
 .UNSPECIFIED., .F., .F.,
 ( 4, 4 ),
 ( 0.000000000000000000, 0.0009166666666666628549 ),
 .UNSPECIFIED. ) ;
#38228 = ORIENTED_EDGE ( 'NONE', *, *, #36586, .T. ) ;
#38229 = ORIENTED_EDGE ( 'NONE', *, *, #65772, .T. ) ;
#38230 = CARTESIAN_POINT ( 'NONE',  ( 29.70220533433691301, -6.475225279485573360, 28.20564067601639735 ) ) ;
#38231 = CARTESIAN_POINT ( 'NONE',  ( 16.91677535067316995, -12.78530099663392505, 11.49999999999998934 ) ) ;
#38232 = CARTESIAN_POINT ( 'NONE',  ( -94.62287095715007013, -23.73907113216990794, -1.053371485793227702 ) ) ;
#38233 = CARTESIAN_POINT ( 'NONE',  ( -30.63234162661936111, -23.86952536761623023, -1.017619990082605952 ) ) ;
#38234 = CARTESIAN_POINT ( 'NONE',  ( -99.55620429048339304, -24.64898659630529210, 1.056161002820829919 ) ) ;
#38235 = CARTESIAN_POINT ( 'NONE',  ( 5.326923076923078426, -5.876774720514419847, 20.76772836538461320 ) ) ;
#38236 = CARTESIAN_POINT ( 'NONE',  ( -11.15089393765527959, -15.82809448842462885, 11.49999999999998934 ) ) ;
#38237 = CARTESIAN_POINT ( 'NONE',  ( -39.02569778787134425, -25.30060000302003331, 6.009290021095885059 ) ) ;
#38238 = ORIENTED_EDGE ( 'NONE', *, *, #54819, .T. ) ;
#38239 = CARTESIAN_POINT ( 'NONE',  ( -18.83898130102433299, -4.906684326670742280, 11.49999999999999645 ) ) ;
#38240 = DIRECTION ( 'NONE',  ( -1.000000000000000000, -3.773278334444166432E-23, -8.201307841325785021E-29 ) ) ;
#38241 = CARTESIAN_POINT ( 'NONE',  ( -103.5228709571500900, -24.33927499327855415, 9.819080762295806508 ) ) ;
#38242 = ORIENTED_EDGE ( 'NONE', *, *, #66341, .F. ) ;
#38243 = DIRECTION ( 'NONE',  ( -0.000000000000000000, 2.173523156925979552E-06, -0.9999999999976378895 ) ) ;
#38244 = CARTESIAN_POINT ( 'NONE',  ( 17.51792015816173986, 5.965225279485572685, 29.01255224319336889 ) ) ;
#38245 = VECTOR ( 'NONE', #31973, 1000.000000000000114 ) ;
#38246 = PLANE ( 'NONE',  #6643 ) ;
#38247 = EDGE_CURVE ( 'NONE', #5695, #39942, #57361, .T. ) ;
#38248 = CARTESIAN_POINT ( 'NONE',  ( -55.62287095715002749, -24.92579138211018375, 1.929029949965663349 ) ) ;
#38249 = CARTESIAN_POINT ( 'NONE',  ( 19.40334540789412188, 3.064012487144803565, 11.49999999999998934 ) ) ;
#38250 = CARTESIAN_POINT ( 'NONE',  ( -40.99816688406356491, -25.31583739607578920, 4.936760826533250324 ) ) ;
#38251 = VERTEX_POINT ( 'NONE', #81171 ) ;
#38252 = CARTESIAN_POINT ( 'NONE',  ( -2.376235263977734657, 21.45616117177731041, -1.500000000000002220 ) ) ;
#38253 = DIRECTION ( 'NONE',  ( 0.6599726524652352877, -0.000000000000000000, -0.7512896232465891000 ) ) ;
#38254 = CARTESIAN_POINT ( 'NONE',  ( -40.63664402775552986, -24.63355581998383670, 0.9682620441943914358 ) ) ;
#38255 = CARTESIAN_POINT ( 'NONE',  ( 30.53060340732036337, 1.682774720514426114, -1.352392034746782823 ) ) ;
#38256 = CARTESIAN_POINT ( 'NONE',  ( 11.60186680256600233, 19.91347440808847935, -1.500000000000002220 ) ) ;
#38257 = EDGE_CURVE ( 'NONE', #23443, #11463, #81675, .T. ) ;
#38258 = AXIS2_PLACEMENT_3D ( 'NONE', #23056, #92086, #99193 ) ;
#38259 = APPROVAL_STATUS ( 'not_yet_approved' ) ;
#38260 = CARTESIAN_POINT ( 'NONE',  ( -93.56158353983492759, -23.48783264082477018, -1.443836473390090358 ) ) ;
#38261 = FACE_OUTER_BOUND ( 'NONE', #46347, .T. ) ;
#38262 = CARTESIAN_POINT ( 'NONE',  ( -18.82339984186270598, 7.397194320553815317, 11.49999999999999645 ) ) ;
#38263 = DIRECTION ( 'NONE',  ( -3.773278334453079618E-23, 0.9999999999976377785, 2.173523156925978705E-06 ) ) ;
#38264 = CARTESIAN_POINT ( 'NONE',  ( 22.81105451610979173, 1.477225279485574028, -18.46691820600746681 ) ) ;
#38265 = AXIS2_PLACEMENT_3D ( 'NONE', #89630, #26234, #20111 ) ;
#38266 = CARTESIAN_POINT ( 'NONE',  ( -110.3641915914744800, -25.29823811401694655, 2.833513268873118829 ) ) ;
#38267 = CARTESIAN_POINT ( 'NONE',  ( -34.62287095715005592, -29.50250786944525672, 11.44777988621624409 ) ) ;
#38268 = CARTESIAN_POINT ( 'NONE',  ( -122.5228709571500332, -24.51387760970725438, 9.387446482453409402 ) ) ;
#38269 = CARTESIAN_POINT ( 'NONE',  ( 12.47747183659840786, 15.48776231947736015, 11.49999999999998934 ) ) ;
#38270 = VECTOR ( 'NONE', #10303, 1000.000000000000114 ) ;
#38271 = PLANE ( 'NONE',  #79237 ) ;
#38272 = CARTESIAN_POINT ( 'NONE',  ( -15.09475962229707591, 12.77647934908296712, -1.500000000000002220 ) ) ;
#38273 = AXIS2_PLACEMENT_3D ( 'NONE', #96216, #34813, #43433 ) ;
#38274 = CARTESIAN_POINT ( 'NONE',  ( -56.54233644916853763, -24.34968618360933590, 0.1864209137778786995 ) ) ;
#38275 = FACE_OUTER_BOUND ( 'NONE', #46748, .T. ) ;
#38276 = LINE ( 'NONE', #36794, #29670 ) ;
#38277 = CARTESIAN_POINT ( 'NONE',  ( -13.38394104848841693, -15.81244124602197765, 11.49999999999999645 ) ) ;
#38278 = CARTESIAN_POINT ( 'NONE',  ( -38.52287095715006870, -29.50248528299804818, 1.056150453629031594 ) ) ;
#38279 = CC_DESIGN_PERSON_AND_ORGANIZATION_ASSIGNMENT ( #87061, #17046, ( #47237 ) ) ;
#38280 = CARTESIAN_POINT ( 'NONE',  ( -35.52287095715006870, -23.47596703998600631, 11.44779298504229281 ) ) ;
#38281 = B_SPLINE_CURVE_WITH_KNOTS ( 'NONE', 3,
 ( #47469, #78396, #8899, #39845, #94632, #32230, #63204, #2302 ),
 .UNSPECIFIED., .F., .F.,
 ( 4, 2, 2, 4 ),
 ( 0.000000000000000000, 0.002001079623178220190, 0.003001619434767332020, 0.004002159246356443850 ),
 .UNSPECIFIED. ) ;
#38282 = CARTESIAN_POINT ( 'NONE',  ( -5.793434319722853054, -21.96748078227757617, 11.49999999999999645 ) ) ;
#38283 = ORIENTED_EDGE ( 'NONE', *, *, #79295, .F. ) ;
#38284 = DIRECTION ( 'NONE',  ( 0.000000000000000000, -1.000000000000000000, 0.000000000000000000 ) ) ;
#38285 = CARTESIAN_POINT ( 'NONE',  ( 32.66876533700882845, 6.475225279485573360, -12.58926540598385557 ) ) ;
#38286 = CARTESIAN_POINT ( 'NONE',  ( -15.75104486599040321, 12.61009050114280861, -1.500000000000002220 ) ) ;
#38287 = B_SPLINE_CURVE_WITH_KNOTS ( 'NONE', 3,
 ( #584, #17311, #25928, #93931 ),
 .UNSPECIFIED., .F., .F.,
 ( 4, 4 ),
 ( 0.000000000000000000, 9.999999999998897304E-05 ),
 .UNSPECIFIED. ) ;
#38288 = DIRECTION ( 'NONE',  ( -1.000000000000000000, -0.000000000000000000, -0.000000000000000000 ) ) ;
#38289 = DIRECTION ( 'NONE',  ( -3.773278334453079618E-23, 0.9999999999976377785, 2.173523156925979975E-06 ) ) ;
#38290 = EDGE_CURVE ( 'NONE', #85635, #76224, #11160, .T. ) ;
#38291 = VECTOR ( 'NONE', #9295, 1000.000000000000000 ) ;
#38292 = ORIENTED_EDGE ( 'NONE', *, *, #5017, .F. ) ;
#38293 = ORIENTED_EDGE ( 'NONE', *, *, #10326, .F. ) ;
#38294 = FACE_OUTER_BOUND ( 'NONE', #12011, .T. ) ;
#38295 = CARTESIAN_POINT ( 'NONE',  ( 18.56524475492553705, -13.42312393814442650, 11.49999999999998934 ) ) ;
#38296 = CARTESIAN_POINT ( 'NONE',  ( 19.75748517575715368, -5.965225279485572685, 28.87153971905864580 ) ) ;
#38297 = CARTESIAN_POINT ( 'NONE',  ( -21.01067979154616694, 5.129389437380057259, -1.500000000000002220 ) ) ;
#38298 = CARTESIAN_POINT ( 'NONE',  ( -123.5209524854786167, -23.96119346886881019, -0.6495511937832023630 ) ) ;
#38299 = LINE ( 'NONE', #83979, #16066 ) ;
#38300 = CARTESIAN_POINT ( 'NONE',  ( -0.8937202392249329330, 20.86669477224961256, 11.49999999999999645 ) ) ;
#38301 = VERTEX_POINT ( 'NONE', #79665 ) ;
#38302 = CARTESIAN_POINT ( 'NONE',  ( -68.99199226862026535, -25.31612623828177888, 5.787353048591010740 ) ) ;
#38303 = CARTESIAN_POINT ( 'NONE',  ( -2.093881351098874521, -21.91542971883435698, -1.500000000000002220 ) ) ;
#38304 = CARTESIAN_POINT ( 'NONE',  ( -64.52287095715006160, -23.47593901973090169, -1.443836447538996870 ) ) ;
#38305 = CARTESIAN_POINT ( 'NONE',  ( -27.89469851781394283, -24.79700315216039996, 7.595246444988488221 ) ) ;
#38306 = ORIENTED_EDGE ( 'NONE', *, *, #24587, .T. ) ;
#38307 = CARTESIAN_POINT ( 'NONE',  ( 4.967620699791259753, -6.376774720514415407, 19.94530485585548973 ) ) ;
#38308 = DIRECTION ( 'NONE',  ( -0.000000000000000000, -1.000000000000000000, -0.000000000000000000 ) ) ;
#38309 = EDGE_LOOP ( 'NONE', ( #1286, #34909, #80987, #75646 ) ) ;
#38310 = CYLINDRICAL_SURFACE ( 'NONE', #72887, 7.652410033082760243 ) ;
#38311 = ORIENTED_EDGE ( 'NONE', *, *, #31197, .F. ) ;
#38312 = ORIENTED_EDGE ( 'NONE', *, *, #41100, .T. ) ;
#38313 = ADVANCED_FACE ( 'NONE', ( #11651 ), #67817, .T. ) ;
#38314 = CARTESIAN_POINT ( 'NONE',  ( -61.64687923781919920, -25.13069339737145214, 2.947789366383932297 ) ) ;
#38315 = CARTESIAN_POINT ( 'NONE',  ( -95.62287095714998486, -23.85229601348997264, 10.88205029486207032 ) ) ;
#38316 = CARTESIAN_POINT ( 'NONE',  ( -100.5228709571500758, -24.91570333825770689, 8.075032458260348989 ) ) ;
#38317 = CARTESIAN_POINT ( 'NONE',  ( 10.21088607376515789, 17.76353854702842483, -1.500000000000002220 ) ) ;
#38318 = ORIENTED_EDGE ( 'NONE', *, *, #63259, .T. ) ;
#38319 = CARTESIAN_POINT ( 'NONE',  ( -2.711489738547795625, -5.876774720514409189, 19.27798293355755632 ) ) ;
#38320 = DIRECTION ( 'NONE',  ( 0.06975647374412549673, 0.9975640502598241977, 0.000000000000000000 ) ) ;
#38321 = CARTESIAN_POINT ( 'NONE',  ( -13.89275734969026388, 5.965225279485572685, 31.02402280011862246 ) ) ;
#38322 = CARTESIAN_POINT ( 'NONE',  ( 13.76814385225720372, 17.53657229028232223, -1.500000000000002220 ) ) ;
#38323 = AXIS2_PLACEMENT_3D ( 'NONE', #40147, #71102, #1592 ) ;
#38324 = B_SPLINE_CURVE_WITH_KNOTS ( 'NONE', 3,
 ( #48791, #4104, #18323, #27442 ),
 .UNSPECIFIED., .F., .F.,
 ( 4, 4 ),
 ( 6.938893903907228378E-18, 9.999999999999591193E-05 ),
 .UNSPECIFIED. ) ;
#38325 = B_SPLINE_CURVE_WITH_KNOTS ( 'NONE', 3,
 ( #41382, #72838, #20034, #58602 ),
 .UNSPECIFIED., .F., .F.,
 ( 4, 4 ),
 ( 0.1398858135129756319, 0.1488922447850913322 ),
 .UNSPECIFIED. ) ;
#38326 = CARTESIAN_POINT ( 'NONE',  ( -4.152941208099351300, -6.376774720514415407, 20.35309744218305639 ) ) ;
#38327 = LINE ( 'NONE', #84504, #59354 ) ;
#38328 = ORIENTED_EDGE ( 'NONE', *, *, #40380, .F. ) ;
#38329 = CARTESIAN_POINT ( 'NONE',  ( -29.59050140619070746, -25.08417512812387784, 3.123287764124576427 ) ) ;
#38330 = CARTESIAN_POINT ( 'NONE',  ( -39.52287095715006160, -23.96177878511308634, 10.65340807706330573 ) ) ;
#38331 = ADVANCED_FACE ( 'NONE', ( #3560 ), #65478, .F. ) ;
#38332 = CARTESIAN_POINT ( 'NONE',  ( -20.21371806590929410, -4.994250807877889109, 11.49999999999998934 ) ) ;
#38333 = EDGE_CURVE ( 'NONE', #75143, #79503, #26887, .T. ) ;
#38334 = VERTEX_POINT ( 'NONE', #2562 ) ;
#38336 = ORIENTED_EDGE ( 'NONE', *, *, #38426, .T. ) ;
#38335 = CARTESIAN_POINT ( 'NONE',  ( -42.52287095715006870, -24.51387760970724372, 9.387446482453423613 ) ) ;
#38337 = CIRCLE ( 'NONE', #48055, 3.060000000000000053 ) ;
#38338 = CARTESIAN_POINT ( 'NONE',  ( -98.52287095715009002, -24.66019654487200441, 8.947790411086119278 ) ) ;
#38339 = VERTEX_POINT ( 'NONE', #33498 ) ;
#38340 = VERTEX_POINT ( 'NONE', #64484 ) ;
#38341 = VECTOR ( 'NONE', #85372, 1000.000000000000114 ) ;
#38342 = DIRECTION ( 'NONE',  ( 1.000000000000000000, 3.773278334444167608E-23, 8.201307833595939069E-29 ) ) ;
#38343 = CARTESIAN_POINT ( 'NONE',  ( -80.58953762381672448, -24.99156044556120193, 7.747789690856343725 ) ) ;
#38344 = CARTESIAN_POINT ( 'NONE',  ( -110.7941337500641765, -25.27168412048538571, 6.209429327144849076 ) ) ;
#38345 = VECTOR ( 'NONE', #59063, 1000.000000000000000 ) ;
#38346 = CARTESIAN_POINT ( 'NONE',  ( -99.12380231474227799, -25.26431306044052150, 4.001575155705512366 ) ) ;
#38347 = CARTESIAN_POINT ( 'NONE',  ( -92.50696408965231399, -24.51419770103157347, 9.386484678747171628 ) ) ;
#38348 = LINE ( 'NONE', #284, #61102 ) ;
#38350 = VERTEX_POINT ( 'NONE', #75537 ) ;
#38349 = CARTESIAN_POINT ( 'NONE',  ( -21.51168160490077952, -5.175097382202364926, 11.49999999999999645 ) ) ;
#38351 = ADVANCED_FACE ( 'NONE', ( #59846 ), #60847, .T. ) ;
#38352 = DIRECTION ( 'NONE',  ( -1.000000000000000000, -3.773278334444167608E-23, -8.201307833595939069E-29 ) ) ;
#38353 = ORIENTED_EDGE ( 'NONE', *, *, #49327, .T. ) ;
#38354 = CARTESIAN_POINT ( 'NONE',  ( 22.31954755298990278, 3.869410565987296380, -1.500000000000002220 ) ) ;
#38355 = VECTOR ( 'NONE', #28302, 1000.000000000000114 ) ;
#38357 = ORIENTED_EDGE ( 'NONE', *, *, #40541, .T. ) ;
#38356 = CARTESIAN_POINT ( 'NONE',  ( -29.10259911666015498, -25.11412234476797067, 6.379066241192269615 ) ) ;
#38358 = ORIENTED_EDGE ( 'NONE', *, *, #84868, .T. ) ;
#38359 = CARTESIAN_POINT ( 'NONE',  ( -99.58953762381672448, -24.65952944569304606, 1.056160979905699682 ) ) ;
#38360 = CARTESIAN_POINT ( 'NONE',  ( -19.81368827760683260, -3.497637702615509880, 11.49999999999998934 ) ) ;
#38361 = CARTESIAN_POINT ( 'NONE',  ( 12.92500000000000249, 1.999999999999999556, 24.00000000000000000 ) ) ;
#38362 = EDGE_LOOP ( 'NONE', ( #21102, #56609, #92260, #79016 ) ) ;
#38363 = B_SPLINE_CURVE_WITH_KNOTS ( 'NONE', 3,
 ( #60902, #60408, #82717, #5599 ),
 .UNSPECIFIED., .F., .F.,
 ( 4, 4 ),
 ( 0.7503217108452443496, 0.7593281421173597723 ),
 .UNSPECIFIED. ) ;
#38364 = CARTESIAN_POINT ( 'NONE',  ( -92.62287095715005592, -23.48786465467241413, 11.44779295918254469 ) ) ;
#38365 = CARTESIAN_POINT ( 'NONE',  ( -21.16112330106665240, 7.131417522999676351, -1.500000000000002220 ) ) ;
#38366 = EDGE_LOOP ( 'NONE', ( #4758, #85247, #59046, #64663 ) ) ;
#38367 = ORIENTED_EDGE ( 'NONE', *, *, #22103, .F. ) ;
#38368 = DIRECTION ( 'NONE',  ( 0.000000000000000000, -1.000000000000000000, 0.000000000000000000 ) ) ;
#38369 = LINE ( 'NONE', #45005, #19997 ) ;
#38370 = CARTESIAN_POINT ( 'NONE',  ( 32.98733314340959311, -5.965225279485572685, 2.074222136288530027 ) ) ;
#38371 = VECTOR ( 'NONE', #27613, 1000.000000000000114 ) ;
#38372 = FACE_OUTER_BOUND ( 'NONE', #55539, .T. ) ;
#38373 = CYLINDRICAL_SURFACE ( 'NONE', #90951, 1.249999999999997558 ) ;
#38374 = CARTESIAN_POINT ( 'NONE',  ( 17.37147561666312257, 8.948746033654231269, -1.500000000000002220 ) ) ;
#38375 = DIRECTION ( 'NONE',  ( 0.1087265912856348327, 0.000000000000000000, -0.9940716917543757081 ) ) ;
#38376 = CARTESIAN_POINT ( 'NONE',  ( 10.45947017991876926, -18.73710855793504848, 11.49999999999998934 ) ) ;
#38377 = AXIS2_PLACEMENT_3D ( 'NONE', #52476, #85403, #68196 ) ;
#38378 = CARTESIAN_POINT ( 'NONE',  ( -10.58858228176428717, -5.965225279485594001, -27.03148018517017093 ) ) ;
#38379 = FACE_OUTER_BOUND ( 'NONE', #69893, .T. ) ;
#38380 = CARTESIAN_POINT ( 'NONE',  ( -129.5228709571500758, -23.48786465467242479, 11.44779295918253581 ) ) ;
#38381 = CARTESIAN_POINT ( 'NONE',  ( -20.27875734969026311, -4.543225279485573864, 26.25402280011862288 ) ) ;
#38382 = CARTESIAN_POINT ( 'NONE',  ( 6.305670413343573699, 22.00876638805999974, -1.500000000000002220 ) ) ;
#38383 = EDGE_CURVE ( 'NONE', #29853, #5623, #29375, .T. ) ;
#38384 = DATE_TIME_ROLE ( 'creation_date' ) ;
#38385 = CARTESIAN_POINT ( 'NONE',  ( -101.5895376238167245, -23.47593901973091235, -1.443836447539001089 ) ) ;
#38386 = DIRECTION ( 'NONE',  ( -0.6599726524652352877, 0.000000000000000000, 0.7512896232465891000 ) ) ;
#38387 = CARTESIAN_POINT ( 'NONE',  ( -0.1815635828756200498, -20.05798930676971636, 11.49999999999999645 ) ) ;
#38388 = CARTESIAN_POINT ( 'NONE',  ( -79.67189865184847974, -25.26612408227589768, 4.664461613298229281 ) ) ;
#38389 = FACE_OUTER_BOUND ( 'NONE', #57684, .T. ) ;
#38390 = CARTESIAN_POINT ( 'NONE',  ( 4.886128916861816052, -5.876774720514411854, 19.14085035285361514 ) ) ;
#38391 = FACE_OUTER_BOUND ( 'NONE', #44701, .T. ) ;
#38392 = ORIENTED_EDGE ( 'NONE', *, *, #47136, .F. ) ;
#38393 = CARTESIAN_POINT ( 'NONE',  ( -109.5228709571500332, -23.94994826722564696, -0.6494450866342718065 ) ) ;
#38394 = DIRECTION ( 'NONE',  ( 0.000000000000000000, -1.000000000000000000, 0.000000000000000000 ) ) ;
#38395 = CARTESIAN_POINT ( 'NONE',  ( -12.78816955685674372, 17.57309652720472570, 11.49999999999998934 ) ) ;
#38396 = CARTESIAN_POINT ( 'NONE',  ( -39.62287095715005592, -29.50250243563736774, 8.947779886222148704 ) ) ;
#38397 = CARTESIAN_POINT ( 'NONE',  ( -12.94911239430987315, -14.73082512860577609, -1.500000000000002220 ) ) ;
#38398 = AXIS2_PLACEMENT_3D ( 'NONE', #27397, #94897, #11657 ) ;
#38399 = CARTESIAN_POINT ( 'NONE',  ( 0.000000000000000000, 0.000000000000000000, 0.000000000000000000 ) ) ;
#38400 = B_SPLINE_CURVE_WITH_KNOTS ( 'NONE', 3,
 ( #3257, #17453, #10851, #33180, #96090, #87978 ),
 .UNSPECIFIED., .F., .F.,
 ( 4, 2, 4 ),
 ( 6.391158118973930141E-06, 0.001387004593080793519, 0.002767618028042612838 ),
 .UNSPECIFIED. ) ;
#38401 = CARTESIAN_POINT ( 'NONE',  ( -109.4462232385598099, -25.27925759040196141, 4.635298292504290707 ) ) ;
#38402 = APPROVAL_DATE_TIME ( #76952, #6561 ) ;
#38403 = PLANE ( 'NONE',  #90466 ) ;
#38404 = CARTESIAN_POINT ( 'NONE',  ( 3.050049012211247579, -5.876774720514426065, 21.53019692557248632 ) ) ;
#38405 = CARTESIAN_POINT ( 'NONE',  ( -18.14515864413662172, 9.488524743509296755, 11.49999999999999645 ) ) ;
#38406 = DIRECTION ( 'NONE',  ( -3.773278334453079030E-23, 0.9999999999976377785, 2.173523156925979128E-06 ) ) ;
#38407 = AXIS2_PLACEMENT_3D ( 'NONE', #3502, #87733, #81615 ) ;
#38408 = CARTESIAN_POINT ( 'NONE',  ( -120.5169643464197975, -24.83618233451451118, 1.606449574219542598 ) ) ;
#38409 = EDGE_CURVE ( 'NONE', #26640, #51831, #6546, .T. ) ;
#38410 = ORIENTED_EDGE ( 'NONE', *, *, #70788, .T. ) ;
#38411 = CARTESIAN_POINT ( 'NONE',  ( -99.65355524409876864, -25.31296369576671523, 4.362766217231969890 ) ) ;
#38412 = CARTESIAN_POINT ( 'NONE',  ( 32.98733314340959311, 0.3587747205144265483, 2.074222136288530027 ) ) ;
#38413 = CARTESIAN_POINT ( 'NONE',  ( -125.6251146265216221, -24.15602025860897584, 10.28564288303534013 ) ) ;
#38414 = CARTESIAN_POINT ( 'NONE',  ( 15.06054736595347343, -3.522115819418385030, -27.30839264876215466 ) ) ;
#38415 = ADVANCED_FACE ( 'NONE', ( #91765 ), #64419, .F. ) ;
#38416 = AXIS2_PLACEMENT_3D ( 'NONE', #90397, #43729, #27510 ) ;
#38417 = CARTESIAN_POINT ( 'NONE',  ( -25.53444008324515124, -24.61459456346077701, 5.226875869559658661 ) ) ;
#38418 = CARTESIAN_POINT ( 'NONE',  ( 31.16918082143019220, 5.911085521256299380, -1.357342440710215481 ) ) ;
#38419 = EDGE_CURVE ( 'NONE', #15581, #76298, #76624, .T. ) ;
#38420 = EDGE_CURVE ( 'NONE', #38639, #63436, #75042, .T. ) ;
#38421 = CARTESIAN_POINT ( 'NONE',  ( 22.66633601775066253, -4.223608244049824378, 11.49999999999999645 ) ) ;
#38422 = CARTESIAN_POINT ( 'NONE',  ( 21.14626179850551324, 8.528272852130310611, 11.49999999999998934 ) ) ;
#38423 = CARTESIAN_POINT ( 'NONE',  ( -74.64912136475619775, -23.48783264082477018, -1.443836473390096353 ) ) ;
#38424 = CARTESIAN_POINT ( 'NONE',  ( -96.63903541359736948, -23.48783264082477018, -1.443836473390089914 ) ) ;
#38425 = CYLINDRICAL_SURFACE ( 'NONE', #7959, 28.45799999999999486 ) ;
#38426 = EDGE_CURVE ( 'NONE', #50071, #9886, #79903, .T. ) ;
#38427 = CARTESIAN_POINT ( 'NONE',  ( -20.38924965233672282, -9.335317855073830273, 11.49999999999999645 ) ) ;
#38428 = ORIENTED_EDGE ( 'NONE', *, *, #18417, .F. ) ;
#38429 = CARTESIAN_POINT ( 'NONE',  ( -40.52287095715007581, -25.00182538069145011, 7.747789668545104647 ) ) ;
#38430 = PLANE ( 'NONE',  #22169 ) ;
#38431 = CARTESIAN_POINT ( 'NONE',  ( -21.18249553426131015, -5.656070447573528170, 11.49999999999998934 ) ) ;
#38432 = CARTESIAN_POINT ( 'NONE',  ( -5.053929855541893446, -5.876774720514408301, 19.14848118821636547 ) ) ;
#38433 = DIRECTION ( 'NONE',  ( -0.000000000000000000, -1.000000000000000000, 0.000000000000000000 ) ) ;
#38434 = CARTESIAN_POINT ( 'NONE',  ( -77.62287095715007013, -24.65952944569304606, 1.056160979905699016 ) ) ;
#38435 = CARTESIAN_POINT ( 'NONE',  ( -125.5228709571500616, -24.99156044556120904, 7.747789690856173195 ) ) ;
#38436 = LINE ( 'NONE', #13589, #74418 ) ;
#38437 = VERTEX_POINT ( 'NONE', #68445 ) ;
#38438 = CARTESIAN_POINT ( 'NONE',  ( -4.979992623568794130, 19.86841884474198494, 11.49999999999998934 ) ) ;
#38439 = VERTEX_POINT ( 'NONE', #4561 ) ;
#38440 = ORIENTED_EDGE ( 'NONE', *, *, #74230, .F. ) ;
#38441 = ORIENTED_EDGE ( 'NONE', *, *, #62971, .T. ) ;
#38442 = ORIENTED_EDGE ( 'NONE', *, *, #46272, .T. ) ;
#38443 = EDGE_CURVE ( 'NONE', #4897, #24545, #67957, .T. ) ;
#38444 = CARTESIAN_POINT ( 'NONE',  ( -23.06710473063640165, 0.7821689226722955413, -1.500000000000002220 ) ) ;
#38445 = CARTESIAN_POINT ( 'NONE',  ( -102.5228709571501042, -24.66019654487200441, 8.947790411086119278 ) ) ;
#38446 = CARTESIAN_POINT ( 'NONE',  ( 17.43904876784772284, 10.37648870149486413, -1.500000000000002220 ) ) ;
#38447 = ORIENTED_EDGE ( 'NONE', *, *, #33885, .T. ) ;
#38448 = AXIS2_PLACEMENT_3D ( 'NONE', #10766, #19366, #49845 ) ;
#38449 = CARTESIAN_POINT ( 'NONE',  ( -29.49875734969026198, 0.3587747205144262708, 7.870022800118625206 ) ) ;
#38450 = DIRECTION ( 'NONE',  ( 1.000000000000000000, 0.000000000000000000, 0.000000000000000000 ) ) ;
#38451 = CARTESIAN_POINT ( 'NONE',  ( -73.52287095715007581, -24.64965694238407323, 8.947790433994200043 ) ) ;
#38452 = CARTESIAN_POINT ( 'NONE',  ( -70.63767667287973495, -24.40034930558990922, 0.3402023900116040167 ) ) ;
#38454 = VERTEX_POINT ( 'NONE', #60352 ) ;
#38453 = CARTESIAN_POINT ( 'NONE',  ( -10.41973078503355588, 18.78793304046337198, 11.49999999999999645 ) ) ;
#38455 = CARTESIAN_POINT ( 'NONE',  ( -125.6228709571500559, -24.99132157543083821, 2.256160258750667502 ) ) ;
#38456 = CARTESIAN_POINT ( 'NONE',  ( -34.62287095715005592, -24.64898659630367206, 1.056161002820817485 ) ) ;
#38457 = VERTEX_POINT ( 'NONE', #97397 ) ;
#38458 = AXIS2_PLACEMENT_3D ( 'NONE', #23505, #22009, #7801 ) ;
#38459 = CARTESIAN_POINT ( 'NONE',  ( -17.53982812869053731, -11.02811673548155902, 11.49999999999998934 ) ) ;
#38460 = ADVANCED_FACE ( 'NONE', ( #5538 ), #92860, .T. ) ;
#38461 = ORIENTED_EDGE ( 'NONE', *, *, #96068, .T. ) ;
#38463 = EDGE_LOOP ( 'NONE', ( #33221, #15591 ) ) ;
#38462 = CARTESIAN_POINT ( 'NONE',  ( -123.6228709571500559, -23.48783264082478794, -1.443836473390058606 ) ) ;
#38464 = B_SPLINE_SURFACE_WITH_KNOTS ( 'NONE', 3, 3, ( 
 ( #67680, #98600, #76256, #61059 ),
 ( #52444, #6751, #6256, #36220 ),
 ( #12863, #67183, #13864, #37705 ),
 ( #68665, #91989, #90993, #51945 ),
 ( #22460, #84376, #76744, #21464 ),
 ( #69154, #86383, #69664, #39700 ),
 ( #32593, #9757, #16866, #63064 ) ),
 .UNSPECIFIED., .F., .F., .F.,
 ( 4, 3, 4 ),
 ( 4, 4 ),
 ( 0.0004766839783816787229, 0.1029713700210895116, 0.2054660560637973366 ),
 ( 0.4596109144125399837, 0.4608357025999801904 ),
 .UNSPECIFIED. ) ;
#38465 = EDGE_CURVE ( 'NONE', #81283, #98585, #27883, .T. ) ;
#38466 = CARTESIAN_POINT ( 'NONE',  ( 8.000000000000003553, -5.876774720514426953, 17.50000000000000000 ) ) ;
#38467 = ORIENTED_EDGE ( 'NONE', *, *, #23539, .F. ) ;
#38468 = ORIENTED_EDGE ( 'NONE', *, *, #27378, .T. ) ;
#38469 = CARTESIAN_POINT ( 'NONE',  ( -55.52287095715007581, -23.84081130425355610, 10.88220057483161085 ) ) ;
#38470 = CARTESIAN_POINT ( 'NONE',  ( -77.62287095715009855, -23.47596703998600631, 11.44779298504227683 ) ) ;
#38471 = CARTESIAN_POINT ( 'NONE',  ( -65.49304012721087531, -24.63355581998386867, 0.9682620441943842193 ) ) ;
#38472 = CARTESIAN_POINT ( 'NONE',  ( -4.682628417673765142, 21.48327871026360114, 11.49999999999999645 ) ) ;
#38473 = EDGE_CURVE ( 'NONE', #85527, #32572, #70446, .T. ) ;
#38474 = CARTESIAN_POINT ( 'NONE',  ( -89.54841333971366168, -24.35071581493543391, 9.817618358456025263 ) ) ;
#38475 = CARTESIAN_POINT ( 'NONE',  ( -5.352388609804938469, -21.92410630658433845, -1.500000000000002220 ) ) ;
#38476 = VECTOR ( 'NONE', #64506, 1000.000000000000114 ) ;
#38477 = CARTESIAN_POINT ( 'NONE',  ( -12.59924929152775874, 16.77720732749412846, -1.500000000000002220 ) ) ;
#38478 = EDGE_CURVE ( 'NONE', #84725, #15126, #93419, .T. ) ;
#38479 = PLANE ( 'NONE',  #70723 ) ;
#38480 = DIRECTION ( 'NONE',  ( -1.000000000000000000, -3.773278334444167608E-23, -8.201307833595939069E-29 ) ) ;
#38481 = ORIENTED_EDGE ( 'NONE', *, *, #75762, .T. ) ;
#38482 = EDGE_CURVE ( 'NONE', #96355, #31349, #11128, .T. ) ;
#38483 = EDGE_LOOP ( 'NONE', ( #2932, #28331, #72317, #49732 ) ) ;
#38484 = ORIENTED_EDGE ( 'NONE', *, *, #88162, .T. ) ;
#38485 = DIRECTION ( 'NONE',  ( 0.000000000000000000, 0.000000000000000000, -1.000000000000000000 ) ) ;
#38486 = CIRCLE ( 'NONE', #62772, 0.9999999999999997780 ) ;
#38487 = CARTESIAN_POINT ( 'NONE',  ( 4.199879391047538491, -21.09745483596041282, -1.500000000000002220 ) ) ;
#38488 = CARTESIAN_POINT ( 'NONE',  ( 0.4325450954222598288, 0.000000000000000000, 0.000000000000000000 ) ) ;
#38489 = VERTEX_POINT ( 'NONE', #77538 ) ;
#38490 = CARTESIAN_POINT ( 'NONE',  ( -4.502559807402421121, -20.62786074129878955, -1.500000000000002220 ) ) ;
#38491 = CARTESIAN_POINT ( 'NONE',  ( -47.52287095715006160, -29.50250243563736774, 8.947779886222146928 ) ) ;
#38492 = CARTESIAN_POINT ( 'NONE',  ( -59.79580795642156232, -25.14083923594471059, 2.947789366366678987 ) ) ;
#38493 = CARTESIAN_POINT ( 'NONE',  ( -83.59183038314901637, -24.15620529776628089, 10.23563542870660470 ) ) ;
#38494 = VECTOR ( 'NONE', #85155, 1000.000000000000114 ) ;
#38495 = CARTESIAN_POINT ( 'NONE',  ( -56.62287095715004881, -24.66019654487199020, 8.947790411086131712 ) ) ;
#38496 = CARTESIAN_POINT ( 'NONE',  ( -127.5228709571500332, -24.66019654487200441, 8.947790411086105067 ) ) ;
#38497 = CARTESIAN_POINT ( 'NONE',  ( 18.07010470096111021, 12.80550835427630574, -1.500000000000002220 ) ) ;
#38498 = CARTESIAN_POINT ( 'NONE',  ( -81.64592523690049575, -23.48786465467241413, 11.44779295918254824 ) ) ;
#38499 = ORIENTED_EDGE ( 'NONE', *, *, #12986, .F. ) ;
#38500 = FACE_OUTER_BOUND ( 'NONE', #43658, .T. ) ;
#38501 = CARTESIAN_POINT ( 'NONE',  ( -64.52287095715006160, -23.47593901973090169, -1.443836447538996870 ) ) ;
#38502 = CARTESIAN_POINT ( 'NONE',  ( -68.62287095715005592, -24.64898659630367916, 1.056161002820824368 ) ) ;
#38503 = CARTESIAN_POINT ( 'NONE',  ( -100.6235771224457665, -25.00158670708910691, 2.256160236439218369 ) ) ;
#38504 = CARTESIAN_POINT ( 'NONE',  ( 17.17441491540288823, 9.109037055621362455, 11.49999999999998934 ) ) ;
#38505 = CARTESIAN_POINT ( 'NONE',  ( -20.23222619987061677, -6.887663580918623296, 11.49999999999998934 ) ) ;
#38506 = CARTESIAN_POINT ( 'NONE',  ( 19.75748517575715368, -0.3587747205144265483, 28.87153971905864580 ) ) ;
#38507 = DIRECTION ( 'NONE',  ( -1.000000000000000000, 0.000000000000000000, 0.000000000000000000 ) ) ;
#38508 = CARTESIAN_POINT ( 'NONE',  ( -111.9545715455114987, -25.05712135967895193, 7.447789548357302891 ) ) ;
#38509 = CARTESIAN_POINT ( 'NONE',  ( 32.98733314340959311, -0.3587747205144265483, 2.074222136288530027 ) ) ;
#38510 = CARTESIAN_POINT ( 'NONE',  ( 19.36006514395606004, 11.85157241509795512, -1.500000000000002220 ) ) ;
#38511 = CARTESIAN_POINT ( 'NONE',  ( -106.5895376238167387, -23.47593901973091235, -1.443836447538999312 ) ) ;
#38512 = CARTESIAN_POINT ( 'NONE',  ( -24.90875734969025501, 5.965225279485572685, 26.43402280011862615 ) ) ;
#38513 = CARTESIAN_POINT ( 'NONE',  ( -19.69265041987409859, 1.759638296948408787, 11.49999999999999645 ) ) ;
#38514 = CARTESIAN_POINT ( 'NONE',  ( -88.58953762381669605, -24.64898659630367916, 1.056161002820386052 ) ) ;
#38515 = VERTEX_POINT ( 'NONE', #30374 ) ;
#38516 = DIRECTION ( 'NONE',  ( 1.000000000000000000, 0.000000000000000000, -0.000000000000000000 ) ) ;
#38517 = CARTESIAN_POINT ( 'NONE',  ( -99.29687923781919778, -25.26138073939643292, 6.149712181314777482 ) ) ;
#38518 = LINE ( 'NONE', #69470, #9113 ) ;
#38519 = CARTESIAN_POINT ( 'NONE',  ( 15.40532884848888884, -15.22192433072940609, -1.500000000000002220 ) ) ;
#38520 = VECTOR ( 'NONE', #47465, 1000.000000000000000 ) ;
#38521 = DIRECTION ( 'NONE',  ( 0.000000000000000000, 0.000000000000000000, 1.000000000000000000 ) ) ;
#38522 = CARTESIAN_POINT ( 'NONE',  ( 14.64286990871793392, 12.78475832571431070, -1.500000000000002220 ) ) ;
#38523 = CARTESIAN_POINT ( 'NONE',  ( -80.52287095715004739, -25.00182538069145366, 7.747789668545104647 ) ) ;
#38524 = CARTESIAN_POINT ( 'NONE',  ( -55.49173473690001401, -24.52399227489126687, 9.353111116836526406 ) ) ;
#38525 = CARTESIAN_POINT ( 'NONE',  ( 15.56394622224390645, 12.30447529683395125, 11.49999999999998934 ) ) ;
#38526 = VERTEX_POINT ( 'NONE', #38495 ) ;
#38527 = CARTESIAN_POINT ( 'NONE',  ( -8.236308187080631171, 18.58821751820538637, 11.49999999999999645 ) ) ;
#38528 = CARTESIAN_POINT ( 'NONE',  ( -80.49584335415009662, -24.83618233451450408, 1.606449574219532384 ) ) ;
#38529 = CARTESIAN_POINT ( 'NONE',  ( 33.60454178612405229, -3.597323055450746487, -11.40641020892026170 ) ) ;
#38530 = EDGE_CURVE ( 'NONE', #6142, #44485, #933, .T. ) ;
#38531 = EDGE_LOOP ( 'NONE', ( #55602, #19613, #80905, #53104, #16217, #84918, #27436, #52674, #41977 ) ) ;
#38532 = CARTESIAN_POINT ( 'NONE',  ( -30.61048516611183601, -24.43626637953622449, 0.1835287498755956703 ) ) ;
#38533 = CARTESIAN_POINT ( 'NONE',  ( -92.52287095715006160, -24.64898659630529210, 1.056161002820827921 ) ) ;
#38534 = CARTESIAN_POINT ( 'NONE',  ( -49.13746579462012676, -25.31601915193193975, 5.391919824163067254 ) ) ;
#38535 = CARTESIAN_POINT ( 'NONE',  ( 4.621320343559262689, 12.74999999999999645, 2.100000000000000089 ) ) ;
#38536 = DIRECTION ( 'NONE',  ( 0.000000000000000000, 2.173523156925980399E-06, -0.9999999999976378895 ) ) ;
#38537 = CARTESIAN_POINT ( 'NONE',  ( 10.01938154005162218, -17.43019892170380913, -1.500000000000002220 ) ) ;
#38538 = CARTESIAN_POINT ( 'NONE',  ( -122.6228709571500417, -29.50247984919015209, -1.443849546365046699 ) ) ;
#38539 = VERTEX_POINT ( 'NONE', #7040 ) ;
#38540 = EDGE_CURVE ( 'NONE', #69591, #31747, #23755, .T. ) ;
#38541 = CARTESIAN_POINT ( 'NONE',  ( 0.000000000000000000, -16.94322527948557422, 0.000000000000000000 ) ) ;
#38542 = EDGE_CURVE ( 'NONE', #58804, #20245, #3801, .T. ) ;
#38543 = AXIS2_PLACEMENT_3D ( 'NONE', #58736, #43519, #89685 ) ;
#38544 = ADVANCED_FACE ( 'NONE', ( #32379 ), #37992, .T. ) ;
#38545 = CARTESIAN_POINT ( 'NONE',  ( -8.048360580058307789, -21.46040670285860230, 11.49999999999999645 ) ) ;
#38546 = CARTESIAN_POINT ( 'NONE',  ( -22.42851769774927817, -3.676000928666301792, -1.500000000000002220 ) ) ;
#38547 = ORIENTED_EDGE ( 'NONE', *, *, #84916, .T. ) ;
#38548 = CARTESIAN_POINT ( 'NONE',  ( -109.6228709571500701, -24.34917612406837861, 0.1852690917426676465 ) ) ;
#38549 = CARTESIAN_POINT ( 'NONE',  ( -126.5228709571500616, -23.48786465467241769, 11.44779295918253581 ) ) ;
#38550 = CARTESIAN_POINT ( 'NONE',  ( -39.50187459890584307, -25.26395632038229522, 3.881371279102487026 ) ) ;
#38551 = ADVANCED_FACE ( 'NONE', ( #62855 ), #78535, .T. ) ;
#38552 = CARTESIAN_POINT ( 'NONE',  ( -30.57287095715007297, -25.31541627316749654, 4.725453788811557310 ) ) ;
#38553 = CIRCLE ( 'NONE', #100084, 1.000000000000000000 ) ;
#38554 = CARTESIAN_POINT ( 'NONE',  ( -128.5217320095746061, -24.15620529776629510, 10.23563542870659582 ) ) ;
#38555 = FACE_OUTER_BOUND ( 'NONE', #91973, .T. ) ;
#38556 = ORIENTED_EDGE ( 'NONE', *, *, #45111, .T. ) ;
#38557 = AXIS2_PLACEMENT_3D ( 'NONE', #72705, #51859, #90410 ) ;
#38558 = CARTESIAN_POINT ( 'NONE',  ( 12.54693703879240196, 16.07252283493236433, -1.500000000000002220 ) ) ;
#38559 = B_SPLINE_CURVE_WITH_KNOTS ( 'NONE', 3,
 ( #25075, #55550, #38803, #85985 ),
 .UNSPECIFIED., .F., .F.,
 ( 4, 4 ),
 ( 0.7102931274136203843, 0.7192995586857354740 ),
 .UNSPECIFIED. ) ;
#38560 = ORIENTED_EDGE ( 'NONE', *, *, #88090, .T. ) ;
#38561 = ADVANCED_FACE ( 'NONE', ( #92270 ), #16646, .T. ) ;
#38562 = CARTESIAN_POINT ( 'NONE',  ( 16.94363762160741516, 15.55198921429254533, -1.500000000000002220 ) ) ;
#38563 = CARTESIAN_POINT ( 'NONE',  ( -45.52287095715006160, -24.99132157543083821, 2.256160258750667502 ) ) ;
#38564 = VERTEX_POINT ( 'NONE', #31377 ) ;
#38565 = CARTESIAN_POINT ( 'NONE',  ( -101.1944152955115044, -25.16311295231453826, 6.858246048749960799 ) ) ;
#38566 = DIRECTION ( 'NONE',  ( -0.000000000000000000, 1.000000000000000000, -0.000000000000000000 ) ) ;
#38567 = EDGE_CURVE ( 'NONE', #55380, #73391, #9039, .T. ) ;
#38568 = CARTESIAN_POINT ( 'NONE',  ( -51.62815728054503239, -24.51419770103156637, 9.386484678747176957 ) ) ;
#38570 = ORIENTED_EDGE ( 'NONE', *, *, #83784, .T. ) ;
#38569 = CARTESIAN_POINT ( 'NONE',  ( 19.98919582620916913, -7.218065965386815996, 11.49999999999999645 ) ) ;
#38571 = EDGE_LOOP ( 'NONE', ( #39185, #88130, #33241, #1243 ) ) ;
#38572 = CARTESIAN_POINT ( 'NONE',  ( 20.56832688555235222, -8.368550285707721414, -1.500000000000002220 ) ) ;
#38573 = CARTESIAN_POINT ( 'NONE',  ( -7.709890279958820258, -19.11728055126480186, -1.500000000000002220 ) ) ;
#38574 = ADVANCED_FACE ( 'NONE', ( #61844 ), #14648, .T. ) ;
#38575 = ORIENTED_EDGE ( 'NONE', *, *, #7045, .T. ) ;
#38576 = EDGE_LOOP ( 'NONE', ( #32450, #92018, #87557, #79353 ) ) ;
#38577 = CARTESIAN_POINT ( 'NONE',  ( -108.9979829822171951, -25.31627198676055457, 4.539662782732864166 ) ) ;
#38578 = CARTESIAN_POINT ( 'NONE',  ( -39.32411912248426944, -25.20542183771704714, 3.367115814691465481 ) ) ;
#38579 = ORIENTED_EDGE ( 'NONE', *, *, #93870, .T. ) ;
#38580 = CARTESIAN_POINT ( 'NONE',  ( -91.50657791617553016, -24.51314013834315375, 0.6176544820404143987 ) ) ;
#38581 = ORIENTED_EDGE ( 'NONE', *, *, #71100, .F. ) ;
#38582 = CARTESIAN_POINT ( 'NONE',  ( -39.52287095715009002, -24.33927499327854349, 9.819080762295822495 ) ) ;
#38583 = CARTESIAN_POINT ( 'NONE',  ( -48.52287095715007581, -23.47593901973090524, -1.443836447538997314 ) ) ;
#38584 = CARTESIAN_POINT ( 'NONE',  ( -20.82185584224439978, -0.2524610531272265534, -1.500000000000002220 ) ) ;
#38585 = CARTESIAN_POINT ( 'NONE',  ( 13.71991279636371175, 16.93377936151356877, 11.49999999999999645 ) ) ;
#38586 = CARTESIAN_POINT ( 'NONE',  ( 25.03579691670893936, -5.064143700970446638, -9.488111998929152691 ) ) ;
#38587 = CARTESIAN_POINT ( 'NONE',  ( -78.50464208480038053, -24.35071581493543391, 9.817618358456027039 ) ) ;
#38588 = CARTESIAN_POINT ( 'NONE',  ( -22.46026885398333661, -0.8929446408661095846, -1.500000000000002220 ) ) ;
#38589 = EDGE_CURVE ( 'NONE', #70398, #29553, #92166, .T. ) ;
#38590 = CARTESIAN_POINT ( 'NONE',  ( -50.38822539166533687, -25.26334751702766113, 4.736250638575107530 ) ) ;
#38591 = ORIENTED_EDGE ( 'NONE', *, *, #14674, .T. ) ;
#38592 = CARTESIAN_POINT ( 'NONE',  ( -58.52287095715006160, -23.73907113216989018, -1.053371485793251461 ) ) ;
#38593 = DIRECTION ( 'NONE',  ( -3.773278334453079030E-23, 0.9999999999976377785, 2.173523156925979128E-06 ) ) ;
#38594 = B_SPLINE_CURVE_WITH_KNOTS ( 'NONE', 3,
 ( #13305, #97556, #20415, #32789, #33285, #63772 ),
 .UNSPECIFIED., .F., .F.,
 ( 4, 2, 4 ),
 ( 0.000000000000000000, 0.001380764517854758894, 0.002761529035709517788 ),
 .UNSPECIFIED. ) ;
#38595 = B_SPLINE_SURFACE_WITH_KNOTS ( 'NONE', 3, 1, ( 
 ( #77543, #95288 ),
 ( #87172, #95783 ),
 ( #33377, #42515 ),
 ( #19151, #25772 ),
 ( #57248, #32892 ),
 ( #18650, #71461 ) ),
 .UNSPECIFIED., .F., .F., .F.,
 ( 4, 1, 1, 4 ),
 ( 2, 2 ),
 ( 0.000000000000000000, 0.1985723521474869191, 0.3687871234093659245, 0.5983641756130111400 ),
 ( 0.000000000000000000, 1.000000000000000000 ),
 .UNSPECIFIED. ) ;
#38596 = ORIENTED_EDGE ( 'NONE', *, *, #53619, .T. ) ;
#38597 = ORIENTED_EDGE ( 'NONE', *, *, #48419, .T. ) ;
#38598 = EDGE_CURVE ( 'NONE', #43572, #31857, #54620, .T. ) ;
#38599 = VERTEX_POINT ( 'NONE', #63355 ) ;
#38600 = CARTESIAN_POINT ( 'NONE',  ( 17.14628872753620215, 12.71262973326862245, -1.500000000000002220 ) ) ;
#38601 = ORIENTED_EDGE ( 'NONE', *, *, #72460, .T. ) ;
#38602 = CARTESIAN_POINT ( 'NONE',  ( -14.96386864383857329, 14.77685607883014640, 11.49999999999998934 ) ) ;
#38603 = CARTESIAN_POINT ( 'NONE',  ( -30.42285774359944028, -24.74858208471048471, 1.363670884829966123 ) ) ;
#38604 = DIRECTION ( 'NONE',  ( -3.773278334453079030E-23, 0.9999999999976377785, 2.173523156925979128E-06 ) ) ;
#38605 = CARTESIAN_POINT ( 'NONE',  ( -50.29662818668498403, -25.04370934227833700, 7.560222902623404018 ) ) ;
#38606 = CARTESIAN_POINT ( 'NONE',  ( 3.092608977599853315, -21.74436839971096802, -1.500000000000002220 ) ) ;
#38607 = CARTESIAN_POINT ( 'NONE',  ( -87.52287095715007581, -23.72747288104470087, -1.053458166803226126 ) ) ;
#38608 = ORIENTED_EDGE ( 'NONE', *, *, #31657, .F. ) ;
#38609 = DIRECTION ( 'NONE',  ( 0.000000000000000000, 0.000000000000000000, 1.000000000000000000 ) ) ;
#38610 = B_SPLINE_CURVE_WITH_KNOTS ( 'NONE', 3,
 ( #60010, #82327, #51386, #81832, #98536, #52384 ),
 .UNSPECIFIED., .F., .F.,
 ( 4, 2, 4 ),
 ( 0.000000000000000000, 0.001380901958385379220, 0.002761803916770758441 ),
 .UNSPECIFIED. ) ;
#38611 = CARTESIAN_POINT ( 'NONE',  ( -127.5228709571500616, -23.47596703998600631, 11.44779298504227683 ) ) ;
#38612 = CARTESIAN_POINT ( 'NONE',  ( 18.58881047053902691, 9.431966241625852732, 11.49999999999999645 ) ) ;
#38613 = CARTESIAN_POINT ( 'NONE',  ( 31.63187483939985256, -3.931892516571728446, 27.18445229901795557 ) ) ;
#38614 = CARTESIAN_POINT ( 'NONE',  ( -86.52287095715006160, -23.47596703998600631, 11.44779298504228393 ) ) ;
#38615 = CARTESIAN_POINT ( 'NONE',  ( -10.31630007230791968, -21.90547765859858842, 11.44779298504228038 ) ) ;
#38616 = CARTESIAN_POINT ( 'NONE',  ( 4.979423480801214552, 20.69870207611912605, 11.49999999999998934 ) ) ;
#38617 = CARTESIAN_POINT ( 'NONE',  ( -39.52287095715006870, -29.50248528299804818, 1.056150453629031594 ) ) ;
#38618 = DIRECTION ( 'NONE',  ( 0.000000000000000000, 0.000000000000000000, 1.000000000000000000 ) ) ;
#38619 = CARTESIAN_POINT ( 'NONE',  ( 15.97264542221207151, -3.406413700670978262, -27.93485542787877662 ) ) ;
#38620 = DIRECTION ( 'NONE',  ( -0.000000000000000000, 1.000000000000000000, -0.000000000000000000 ) ) ;
#38621 = CARTESIAN_POINT ( 'NONE',  ( -20.59131556071872282, -9.131246169528550283, -1.500000000000002220 ) ) ;
#38622 = CARTESIAN_POINT ( 'NONE',  ( 30.93860345374796594, -5.515143950957555496, 14.99689261510125249 ) ) ;
#38623 = ORIENTED_EDGE ( 'NONE', *, *, #55125, .F. ) ;
#38624 = CARTESIAN_POINT ( 'NONE',  ( 11.69063526134919684, 3.622774720514426949, -29.65990201929480108 ) ) ;
#38625 = CARTESIAN_POINT ( 'NONE',  ( 19.39309126630920588, -2.812899550206792831, 11.49999999999999645 ) ) ;
#38626 = FACE_OUTER_BOUND ( 'NONE', #42443, .T. ) ;
#38627 = CIRCLE ( 'NONE', #1344, 1.306876713926001354 ) ;
#38628 = CARTESIAN_POINT ( 'NONE',  ( 14.76093561896379214, 6.475225279485573360, -26.55548769130089681 ) ) ;
#38629 = ORIENTED_EDGE ( 'NONE', *, *, #2028, .F. ) ;
#38630 = CARTESIAN_POINT ( 'NONE',  ( -88.51121366609869767, -24.15620529776628800, 10.23563542870660115 ) ) ;
#38631 = CARTESIAN_POINT ( 'NONE',  ( -42.52287095715005449, -24.64965694238575011, 8.947790433994205372 ) ) ;
#38632 = CARTESIAN_POINT ( 'NONE',  ( -36.62287095715005592, -23.48783264082477729, -1.443836473390072372 ) ) ;
#38633 = B_SPLINE_CURVE_WITH_KNOTS ( 'NONE', 3,
 ( #14708, #33949, #56307, #39559 ),
 .UNSPECIFIED., .F., .F.,
 ( 4, 4 ),
 ( 0.000000000000000000, 9.999999999998897304E-05 ),
 .UNSPECIFIED. ) ;
#38634 = CARTESIAN_POINT ( 'NONE',  ( 15.33752688427012778, 12.42672799324400934, -1.500000000000002220 ) ) ;
#38635 = VECTOR ( 'NONE', #35555, 1000.000000000000114 ) ;
#38636 = ORIENTED_EDGE ( 'NONE', *, *, #99387, .F. ) ;
#38637 = CARTESIAN_POINT ( 'NONE',  ( 7.822518687389895753, 3.316774720514091168, -28.18023264461383448 ) ) ;
#38638 = APPROVAL_DATE_TIME ( #53879, #83531 ) ;
#38639 = VERTEX_POINT ( 'NONE', #94271 ) ;
#38640 = CARTESIAN_POINT ( 'NONE',  ( -109.6228709571500275, -24.51387760970724372, 9.387446482453409402 ) ) ;
#38641 = DIRECTION ( 'NONE',  ( 0.000000000000000000, 0.000000000000000000, 1.000000000000000000 ) ) ;
#38642 = CARTESIAN_POINT ( 'NONE',  ( -78.52287095715006160, -24.64965694238408034, 8.947790433994198267 ) ) ;
#38643 = LINE ( 'NONE', #8206, #72043 ) ;
#38644 = CARTESIAN_POINT ( 'NONE',  ( -28.98875734969026396, -5.965225279485572685, -0.08597719988137648983 ) ) ;
#38645 = EDGE_CURVE ( 'NONE', #88005, #76875, #93267, .T. ) ;
#38646 = LINE ( 'NONE', #46265, #19744 ) ;
#38647 = ADVANCED_FACE ( 'NONE', ( #78031 ), #8543, .T. ) ;
#38648 = FACE_OUTER_BOUND ( 'NONE', #28635, .T. ) ;
#38649 = CARTESIAN_POINT ( 'NONE',  ( -15.89961544564849305, 12.09337254111102844, 11.49999999999998934 ) ) ;
#38650 = EDGE_CURVE ( 'NONE', #60317, #94949, #80551, .T. ) ;
#38651 = CARTESIAN_POINT ( 'NONE',  ( -45.58953762381672448, -23.47593901973091235, -1.443836447539009749 ) ) ;
#38652 = CARTESIAN_POINT ( 'NONE',  ( -51.13339157368925214, -25.31518271292250688, 4.891899733068189704 ) ) ;
#38653 = ORIENTED_EDGE ( 'NONE', *, *, #98501, .F. ) ;
#38654 = ADVANCED_FACE ( 'NONE', ( #57732 ), #49125, .T. ) ;
#38655 = CARTESIAN_POINT ( 'NONE',  ( -79.58814944961092408, -24.35071581493543036, 9.817618358456028815 ) ) ;
#38656 = FACE_OUTER_BOUND ( 'NONE', #76578, .T. ) ;
#38657 = CARTESIAN_POINT ( 'NONE',  ( -120.6228709571500559, -24.83602698348162363, 1.605859176311272396 ) ) ;
#38658 = CARTESIAN_POINT ( 'NONE',  ( -28.62287095715004881, -23.33150569529546914, 11.44779297407613150 ) ) ;
#38659 = FACE_OUTER_BOUND ( 'NONE', #10627, .T. ) ;
#38660 = CARTESIAN_POINT ( 'NONE',  ( -83.58263009027983514, -24.65952944569305316, 1.056160979905701680 ) ) ;
#38661 = B_SPLINE_SURFACE_WITH_KNOTS ( 'NONE', 3, 3, ( 
 ( #22702, #84620, #60306, #5999 ),
 ( #68406, #30331, #99339, #37455 ),
 ( #91727, #45077, #22206, #92722 ),
 ( #23210, #84120, #85118, #36949 ),
 ( #45576, #15109, #36449, #76994 ),
 ( #76493, #98839, #37947, #68897 ),
 ( #67416, #28842, #67919, #99824 ) ),
 .UNSPECIFIED., .F., .F., .F.,
 ( 4, 3, 4 ),
 ( 4, 4 ),
 ( 0.2966607060324272793, 0.4953275639659514562, 0.6939944218994755776 ),
 ( 0.04303012530936223962, 0.1472998482329709868 ),
 .UNSPECIFIED. ) ;
#38662 = CARTESIAN_POINT ( 'NONE',  ( -3.095730855174848362, -5.876774720514413630, 20.04377961306771638 ) ) ;
#38663 = EDGE_CURVE ( 'NONE', #68434, #41774, #97031, .T. ) ;
#38664 = CARTESIAN_POINT ( 'NONE',  ( -40.52287095715006870, -23.84081130425358808, 10.88220057483156644 ) ) ;
#38665 = ORIENTED_EDGE ( 'NONE', *, *, #43587, .T. ) ;
#38666 = AXIS2_PLACEMENT_3D ( 'NONE', #95285, #80554, #26770 ) ;
#38667 = CARTESIAN_POINT ( 'NONE',  ( 5.465678960246475704, -19.50585317057041124, 11.49999999999998934 ) ) ;
#38668 = DIRECTION ( 'NONE',  ( 8.719066383522879804E-15, 0.000000000000000000, -1.000000000000000000 ) ) ;
#38669 = VECTOR ( 'NONE', #44965, 1000.000000000000000 ) ;
#38670 = CARTESIAN_POINT ( 'NONE',  ( -99.62287095715005592, -24.64898659630367916, 1.056161002820829697 ) ) ;
#38671 = ORIENTED_EDGE ( 'NONE', *, *, #89969, .F. ) ;
#38672 = DIRECTION ( 'NONE',  ( -3.773278334453080206E-23, 0.9999999999976377785, 2.173523156925979975E-06 ) ) ;
#38673 = CARTESIAN_POINT ( 'NONE',  ( 1.915021276000606454, 20.04344799065331628, -1.500000000000002220 ) ) ;
#38674 = CARTESIAN_POINT ( 'NONE',  ( 11.07546443054301655, -17.96822238807187233, 11.49999999999999645 ) ) ;
#38675 = VECTOR ( 'NONE', #70243, 1000.000000000000000 ) ;
#38676 = CARTESIAN_POINT ( 'NONE',  ( -19.76278938440450617, -9.944092408650034187, 11.49999999999998934 ) ) ;
#38677 = CARTESIAN_POINT ( 'NONE',  ( -14.38416181709762043, 14.64695106392160895, -1.500000000000002220 ) ) ;
#38678 = CARTESIAN_POINT ( 'NONE',  ( -78.52287095715006160, -24.64965694238408034, 8.947790433994198267 ) ) ;
#38679 = CARTESIAN_POINT ( 'NONE',  ( -126.6228709571500275, -23.94994826722566117, -0.6494450866342689199 ) ) ;
#38680 = ORIENTED_EDGE ( 'NONE', *, *, #88958, .T. ) ;
#38681 = DIRECTION ( 'NONE',  ( -3.773278334453079618E-23, 0.9999999999976377785, 2.173523156925979975E-06 ) ) ;
#38682 = EDGE_LOOP ( 'NONE', ( #97354, #32264, #12113, #34425 ) ) ;
#38683 = CARTESIAN_POINT ( 'NONE',  ( -51.62287095715005592, -24.64898659630367206, 1.056161002820821038 ) ) ;
#38684 = CARTESIAN_POINT ( 'NONE',  ( -51.52287095715006870, -29.50250243563736774, 8.947779886222146928 ) ) ;
#38685 = ORIENTED_EDGE ( 'NONE', *, *, #37752, .T. ) ;
#38686 = VERTEX_POINT ( 'NONE', #48625 ) ;
#38687 = ORIENTED_EDGE ( 'NONE', *, *, #50775, .T. ) ;
#38688 = CARTESIAN_POINT ( 'NONE',  ( 22.81105451610979173, -6.475225279485573360, -18.46691820600746681 ) ) ;
#38689 = CARTESIAN_POINT ( 'NONE',  ( -63.62287095715004881, -23.96127896941632685, -0.6493128931037893681 ) ) ;
#38690 = CARTESIAN_POINT ( 'NONE',  ( -68.59250175099369073, -24.15620529776627734, 10.23563542870660825 ) ) ;
#38691 = CARTESIAN_POINT ( 'NONE',  ( 20.62939718826500979, -0.8834638802319035866, -1.500000000000002220 ) ) ;
#38692 = CARTESIAN_POINT ( 'NONE',  ( -14.23256820581467785, 16.29125061305494526, 11.49999999999999645 ) ) ;
#38693 = EDGE_LOOP ( 'NONE', ( #33963, #36530, #14752, #89012 ) ) ;
#38694 = CARTESIAN_POINT ( 'NONE',  ( -29.62287095715004881, -29.50250243563707286, 8.947779751028683393 ) ) ;
#38695 = CARTESIAN_POINT ( 'NONE',  ( -60.62287095715004881, -24.99132157543084531, 2.256160258750667502 ) ) ;
#38696 = CARTESIAN_POINT ( 'NONE',  ( -1.986123035288760885, 22.30159847666916662, -1.500000000000002220 ) ) ;
#38697 = ADVANCED_FACE ( 'NONE', ( #26767 ), #52400, .T. ) ;
#38698 = CARTESIAN_POINT ( 'NONE',  ( -71.52287095715009002, -23.73907113216989373, -1.053371485793249684 ) ) ;
#38699 = CARTESIAN_POINT ( 'NONE',  ( -87.62287095715004170, -29.50248528299804818, 1.056150453629040253 ) ) ;
#38700 = ORIENTED_EDGE ( 'NONE', *, *, #5089, .F. ) ;
#38701 = B_SPLINE_CURVE_WITH_KNOTS ( 'NONE', 3,
 ( #17168, #71473, #46130, #31899 ),
 .UNSPECIFIED., .F., .F.,
 ( 4, 4 ),
 ( 0.05982864664972729896, 0.06883507792184291596 ),
 .UNSPECIFIED. ) ;
#38702 = CARTESIAN_POINT ( 'NONE',  ( 32.96821357219067750, -5.071478440980570213, -13.00504694253962867 ) ) ;
#38703 = FACE_OUTER_BOUND ( 'NONE', #80650, .T. ) ;
#38704 = CARTESIAN_POINT ( 'NONE',  ( -113.5228709571500616, -29.50248528299804818, 1.056150453629043584 ) ) ;
#38705 = CARTESIAN_POINT ( 'NONE',  ( 10.02768300834196502, -18.34552750054021786, 11.49999999999998934 ) ) ;
#38706 = VERTEX_POINT ( 'NONE', #17151 ) ;
#38707 = EDGE_CURVE ( 'NONE', #20665, #60599, #9856, .T. ) ;
#38708 = CARTESIAN_POINT ( 'NONE',  ( -86.51403199199435790, -23.96119346886881374, -0.6495511937831903726 ) ) ;
#38709 = ORIENTED_EDGE ( 'NONE', *, *, #15186, .T. ) ;
#38710 = VECTOR ( 'NONE', #46017, 1000.000000000000114 ) ;
#38711 = DIRECTION ( 'NONE',  ( 3.773278334444166432E-23, -1.000000000000000000, 0.000000000000000000 ) ) ;
#38712 = CARTESIAN_POINT ( 'NONE',  ( 18.66760434907605060, -10.05535386721697222, -1.500000000000002220 ) ) ;
#38713 = EDGE_LOOP ( 'NONE', ( #71249, #44997, #69809, #97420 ) ) ;
#38714 = CARTESIAN_POINT ( 'NONE',  ( -10.34999999999999254, 12.00000000000002309, 0.000000000000000000 ) ) ;
#38715 = CARTESIAN_POINT ( 'NONE',  ( -35.52287095715008292, -25.00182538069144655, 7.747789668545105535 ) ) ;
#38716 = CARTESIAN_POINT ( 'NONE',  ( -21.05831370385527990, 5.553659732266172711, -1.500000000000002220 ) ) ;
#38717 = CARTESIAN_POINT ( 'NONE',  ( -113.9228709571500531, -23.47596703998600631, 11.44779298504227860 ) ) ;
#38718 = CARTESIAN_POINT ( 'NONE',  ( -41.52287095715006870, -23.72747288104469732, -1.053458166803227680 ) ) ;
#38719 = CARTESIAN_POINT ( 'NONE',  ( -101.6228709571500559, -23.48786465467242479, 11.44779295918254114 ) ) ;
#38720 = CARTESIAN_POINT ( 'NONE',  ( 9.643594380127815668, 19.59848315111488759, -1.500000000000002220 ) ) ;
#38721 = CARTESIAN_POINT ( 'NONE',  ( -30.57287095715005876, -24.05191950036741488, 10.45812762691192255 ) ) ;
#38722 = ORIENTED_EDGE ( 'NONE', *, *, #79097, .T. ) ;
#38723 = CARTESIAN_POINT ( 'NONE',  ( -2.704906987277321040, -0.3587747205144061757, -28.92935364444904778 ) ) ;
#38724 = CARTESIAN_POINT ( 'NONE',  ( -70.22287095715006444, -23.47596703998600631, 11.44779298504227860 ) ) ;
#38725 = VERTEX_POINT ( 'NONE', #76780 ) ;
#38726 = ORIENTED_EDGE ( 'NONE', *, *, #3122, .T. ) ;
#38727 = ORIENTED_EDGE ( 'NONE', *, *, #85854, .T. ) ;
#38728 = CARTESIAN_POINT ( 'NONE',  ( 22.81105451610979173, 6.475225279485573360, -18.46691820600746681 ) ) ;
#38729 = CARTESIAN_POINT ( 'NONE',  ( 18.66760434907605060, -10.05535386721697222, -1.500000000000002220 ) ) ;
#38730 = CARTESIAN_POINT ( 'NONE',  ( -28.98875734969026041, 0.3587747205144265483, 17.86602280011862476 ) ) ;
#38731 = CARTESIAN_POINT ( 'NONE',  ( -79.05725560372792415, -25.27791764661166241, 6.604864350711941334 ) ) ;
#38732 = CARTESIAN_POINT ( 'NONE',  ( 20.57455539870830208, -4.132774720514426292, -18.22080502500661581 ) ) ;
#38733 = CARTESIAN_POINT ( 'NONE',  ( 33.07248226229787491, 4.977706540348799891, -12.91345179487514905 ) ) ;
#38734 = CARTESIAN_POINT ( 'NONE',  ( 14.52268490272241408, 12.84546865777419455, 11.49999999999998934 ) ) ;
#38735 = CARTESIAN_POINT ( 'NONE',  ( -40.93292953049032690, -25.30060000302003687, 6.009290021095885059 ) ) ;
#38736 = EDGE_LOOP ( 'NONE', ( #59314, #54212, #63706, #92408, #5119, #86038, #93301, #63703, #88878, #58788, #73158, #66421 ) ) ;
#38737 = VECTOR ( 'NONE', #51161, 1000.000000000000000 ) ;
#38738 = CARTESIAN_POINT ( 'NONE',  ( -15.31790942089943286, 12.02624123284522106, 11.49999999999999645 ) ) ;
#38739 = CARTESIAN_POINT ( 'NONE',  ( -34.62287095715004881, -23.48783264082478084, -1.443836473390074149 ) ) ;
#38740 = AXIS2_PLACEMENT_3D ( 'NONE', #73082, #95902, #96404 ) ;
#38741 = CARTESIAN_POINT ( 'NONE',  ( -103.5228709571500758, -23.95044443724991723, 10.65354141964649237 ) ) ;
#38742 = ORIENTED_EDGE ( 'NONE', *, *, #18898, .T. ) ;
#38743 = LINE ( 'NONE', #23003, #65293 ) ;
#38744 = CARTESIAN_POINT ( 'NONE',  ( 13.91401389203221406, 3.316774720514426456, 158.0376437107427137 ) ) ;
#38745 = CIRCLE ( 'NONE', #66382, 0.2499999999997798983 ) ;
#38746 = CARTESIAN_POINT ( 'NONE',  ( -76.62287095715007013, -23.47596703998600631, 11.44779298504227860 ) ) ;
#38747 = CARTESIAN_POINT ( 'NONE',  ( -55.62287095715004881, -25.00158670708909625, 2.256160236439165967 ) ) ;
#38748 = CARTESIAN_POINT ( 'NONE',  ( -11.98250242409135780, 15.54504917500377559, 11.49999999999998934 ) ) ;
#38749 = DIRECTION ( 'NONE',  ( -1.000000000000000000, -0.000000000000000000, -0.000000000000000000 ) ) ;
#38750 = ORIENTED_EDGE ( 'NONE', *, *, #82879, .F. ) ;
#38751 = CARTESIAN_POINT ( 'NONE',  ( -2.376235263977734657, 21.45616117177731041, 11.49999999999998934 ) ) ;
#38752 = AXIS2_PLACEMENT_3D ( 'NONE', #17331, #25948, #2130 ) ;
#38753 = CARTESIAN_POINT ( 'NONE',  ( 10.34999999999999254, -2.091390571243891402E-15, 2.100000000000000089 ) ) ;
#38754 = CARTESIAN_POINT ( 'NONE',  ( -40.58149357286682601, -24.73486907724916861, 1.287355809206965240 ) ) ;
#38755 = DIRECTION ( 'NONE',  ( 0.000000000000000000, 0.000000000000000000, 1.000000000000000000 ) ) ;
#38756 = CARTESIAN_POINT ( 'NONE',  ( 10.36671515591691950, -20.60271000134967068, -1.500000000000002220 ) ) ;
#38757 = PERSON_AND_ORGANIZATION_ROLE ( 'creator' ) ;
#38758 = CARTESIAN_POINT ( 'NONE',  ( -93.52216992446560084, -23.48783264082477018, -1.443836473390090358 ) ) ;
#38759 = DIRECTION ( 'NONE',  ( 1.000000000000000000, 3.773278334444167608E-23, 8.201307833595939069E-29 ) ) ;
#38760 = CARTESIAN_POINT ( 'NONE',  ( -40.43800977064336877, -25.27941802265787530, 6.123089462926260218 ) ) ;
#38761 = CARTESIAN_POINT ( 'NONE',  ( -39.44687923781921057, -29.50249209050310739, 4.188164501617993807 ) ) ;
#38762 = EDGE_CURVE ( 'NONE', #11930, #84470, #12034, .T. ) ;
#38763 = VECTOR ( 'NONE', #75232, 1000.000000000000000 ) ;
#38765 = B_SPLINE_CURVE_WITH_KNOTS ( 'NONE', 3,
 ( #30519, #6182, #62484, #38631 ),
 .UNSPECIFIED., .F., .F.,
 ( 4, 4 ),
 ( 0.000000000000000000, 9.999999999998900014E-05 ),
 .UNSPECIFIED. ) ;
#38764 = CARTESIAN_POINT ( 'NONE',  ( -111.1265005993262491, -25.10921425174257848, 3.068069789771319389 ) ) ;
#38766 = FACE_OUTER_BOUND ( 'NONE', #64603, .T. ) ;
#38767 = CARTESIAN_POINT ( 'NONE',  ( -99.41873814713473223, -25.26400843806960950, 4.744921592735869886 ) ) ;
#38768 = CARTESIAN_POINT ( 'NONE',  ( -4.768723929037996356, 19.30091236029735668, -1.500000000000002220 ) ) ;
#38769 = EDGE_CURVE ( 'NONE', #43985, #9229, #30123, .T. ) ;
#38770 = LINE ( 'NONE', #60639, #30648 ) ;
#38771 = CARTESIAN_POINT ( 'NONE',  ( 5.644138345009856117, 19.01542066204735448, -1.500000000000002220 ) ) ;
#38772 = CARTESIAN_POINT ( 'NONE',  ( 16.00000000000000000, 21.89999999999999858, 0.000000000000000000 ) ) ;
#38773 = EDGE_CURVE ( 'NONE', #58867, #87961, #52480, .T. ) ;
#38774 = B_SPLINE_CURVE_WITH_KNOTS ( 'NONE', 3,
 ( #61858, #37505, #78046, #92287, #23772, #69952 ),
 .UNSPECIFIED., .F., .F.,
 ( 4, 2, 4 ),
 ( 6.391158118956848875E-06, 0.001387004593080779424, 0.002767618028042601996 ),
 .UNSPECIFIED. ) ;
#38775 = EDGE_CURVE ( 'NONE', #59162, #24461, #69286, .T. ) ;
#38776 = CARTESIAN_POINT ( 'NONE',  ( -73.52287095715007581, -29.50250243563736774, 8.947779886222143375 ) ) ;
#38777 = CARTESIAN_POINT ( 'NONE',  ( -95.22287095715003602, -23.47593901973090169, -1.443836447538996870 ) ) ;
#38778 = CARTESIAN_POINT ( 'NONE',  ( 17.22178217532253086, -11.58000449095910867, 11.49999999999999645 ) ) ;
#38779 = DIRECTION ( 'NONE',  ( -3.773278334444167608E-23, 1.000000000000000000, 0.000000000000000000 ) ) ;
#38780 = EDGE_CURVE ( 'NONE', #89333, #36030, #76292, .T. ) ;
#38781 = B_SPLINE_CURVE_WITH_KNOTS ( 'NONE', 3,
 ( #93805, #54761, #40024, #64395 ),
 .UNSPECIFIED., .F., .F.,
 ( 4, 4 ),
 ( 0.000000000000000000, 0.0001000000000000028644 ),
 .UNSPECIFIED. ) ;
#38782 = CARTESIAN_POINT ( 'NONE',  ( -106.5177727992831223, -23.96119346886880663, -0.6495511937832030291 ) ) ;
#38783 = CARTESIAN_POINT ( 'NONE',  ( 16.14549698687068968, 15.95341496147077720, 11.49999999999999645 ) ) ;
#38784 = ORIENTED_EDGE ( 'NONE', *, *, #99973, .F. ) ;
#38785 = CARTESIAN_POINT ( 'NONE',  ( -69.64548755400529956, -23.73766607897669445, -1.055555164236460008 ) ) ;
#38786 = CARTESIAN_POINT ( 'NONE',  ( -106.6228709571500843, -24.50216790748207174, 0.6166512839542517277 ) ) ;
#38787 = ORIENTED_EDGE ( 'NONE', *, *, #5017, .T. ) ;
#38788 = CARTESIAN_POINT ( 'NONE',  ( 19.72175082351460063, -4.362005935662174316, -1.500000000000002220 ) ) ;
#38789 = EDGE_CURVE ( 'NONE', #94651, #19111, #52386, .T. ) ;
#38790 = CARTESIAN_POINT ( 'NONE',  ( -10.24059822343757808, -5.876774720514426953, 17.17691942396160698 ) ) ;
#38791 = DIRECTION ( 'NONE',  ( -1.000000000000000000, -3.773278334444166432E-23, -8.201307841325785021E-29 ) ) ;
#38792 = ORIENTED_EDGE ( 'NONE', *, *, #33994, .T. ) ;
#38793 = ORIENTED_EDGE ( 'NONE', *, *, #15511, .F. ) ;
#38794 = CARTESIAN_POINT ( 'NONE',  ( -76.62287095715007013, -29.50250243563736774, 8.947779886222141599 ) ) ;
#38795 = CARTESIAN_POINT ( 'NONE',  ( 12.20170062390598709, -19.39347807479101249, 11.49999999999998934 ) ) ;
#38796 = CARTESIAN_POINT ( 'NONE',  ( -51.29535283968221648, -25.27420699915789726, 3.923498428899851564 ) ) ;
#38797 = CARTESIAN_POINT ( 'NONE',  ( 14.58690015069645263, 15.99052346098381250, -1.500000000000002220 ) ) ;
#38798 = CARTESIAN_POINT ( 'NONE',  ( -123.5546994242114920, -24.34968618360933945, 0.1864209137778902459 ) ) ;
#38799 = CARTESIAN_POINT ( 'NONE',  ( -2.368302597431856782, 20.80102113048726409, 11.49999999999999645 ) ) ;
#38800 = ORIENTED_EDGE ( 'NONE', *, *, #60102, .T. ) ;
#38801 = CARTESIAN_POINT ( 'NONE',  ( -124.5563175110222147, -23.73766607897670866, -1.055555164236449350 ) ) ;
#38802 = CARTESIAN_POINT ( 'NONE',  ( -17.76638496452178018, -13.01238552544781335, 11.49999999999998934 ) ) ;
#38803 = CARTESIAN_POINT ( 'NONE',  ( -102.2228709571500644, -23.47593901973090524, -1.443836447538996648 ) ) ;
#38804 = CARTESIAN_POINT ( 'NONE',  ( 282.9764569301858046, 2.682774720514426559, 20.79159422840526616 ) ) ;
#38805 = ORIENTED_EDGE ( 'NONE', *, *, #72578, .F. ) ;
#38806 = DIRECTION ( 'NONE',  ( -0.5656310827093756766, 0.8246584009594636333, 1.161164194647626880E-16 ) ) ;
#38807 = DIRECTION ( 'NONE',  ( 0.000000000000000000, 0.000000000000000000, -1.000000000000000000 ) ) ;
#38808 = ORIENTED_EDGE ( 'NONE', *, *, #10588, .F. ) ;
#38809 = CARTESIAN_POINT ( 'NONE',  ( -72.55405769320448428, -23.96169478059712787, 10.65365249895718414 ) ) ;
#38810 = ORIENTED_EDGE ( 'NONE', *, *, #83022, .T. ) ;
#38811 = AXIS2_PLACEMENT_3D ( 'NONE', #99553, #37182, #68138 ) ;
#38812 = VERTEX_POINT ( 'NONE', #22994 ) ;
#38813 = LINE ( 'NONE', #91603, #25856 ) ;
#38814 = CARTESIAN_POINT ( 'NONE',  ( -83.52287095715006160, -23.72773821059536914, 11.05748984161097503 ) ) ;
#38815 = CARTESIAN_POINT ( 'NONE',  ( -4.147110899021980934, -6.376774720514418959, 20.45311193189268906 ) ) ;
#38816 = CARTESIAN_POINT ( 'NONE',  ( -15.03541999946025243, -13.88573836563254460, -1.500000000000002220 ) ) ;
#38817 = ADVANCED_FACE ( 'NONE', ( #37254 ), #66003, .T. ) ;
#38818 = EDGE_LOOP ( 'NONE', ( #14250, #6504, #1543, #38499 ) ) ;
#38819 = CARTESIAN_POINT ( 'NONE',  ( -99.69921442305546577, -25.29823723214318676, 5.426898400209082318 ) ) ;
#38820 = AXIS2_PLACEMENT_3D ( 'NONE', #30111, #59091, #52969 ) ;
#38821 = CARTESIAN_POINT ( 'NONE',  ( -44.64054379914810511, -24.15543982623906416, -0.2315651400026670914 ) ) ;
#38822 = LINE ( 'NONE', #69785, #77516 ) ;
#38823 = CARTESIAN_POINT ( 'NONE',  ( -17.00426676922356606, 14.40147940013276973, -1.500000000000002220 ) ) ;
#38824 = ADVANCED_FACE ( 'NONE', ( #81559 ), #75797, .T. ) ;
#38825 = CARTESIAN_POINT ( 'NONE',  ( -81.88534077628074215, -25.24685308744633616, 6.293942982122114671 ) ) ;
#38826 = CARTESIAN_POINT ( 'NONE',  ( -1.743696941008423984, -5.876774720514413630, 19.59984006504825160 ) ) ;
#38827 = ORIENTED_EDGE ( 'NONE', *, *, #70524, .T. ) ;
#38828 = CARTESIAN_POINT ( 'NONE',  ( -28.59999605021188884, -24.73585508254603837, 1.848451013847122626 ) ) ;
#38829 = AXIS2_PLACEMENT_3D ( 'NONE', #81756, #66565, #58436 ) ;
#38830 = CARTESIAN_POINT ( 'NONE',  ( 22.02124265030973760, -4.776774720514394446, 16.20402280011862217 ) ) ;
#38831 = CIRCLE ( 'NONE', #93947, 3.060000000000000053 ) ;
#38832 = CARTESIAN_POINT ( 'NONE',  ( -1.025521031027718299, 20.81036885881322362, 11.49999999999998934 ) ) ;
#38833 = ORIENTED_EDGE ( 'NONE', *, *, #97141, .F. ) ;
#38835 = ORIENTED_EDGE ( 'NONE', *, *, #15749, .F. ) ;
#38834 = FACE_OUTER_BOUND ( 'NONE', #77344, .T. ) ;
#38836 = CIRCLE ( 'NONE', #64808, 3.500000000000000000 ) ;
#38837 = DIRECTION ( 'NONE',  ( 0.000000000000000000, 0.000000000000000000, -1.000000000000000000 ) ) ;
#38838 = CARTESIAN_POINT ( 'NONE',  ( -19.58807393344005376, -7.628504261335002923, -1.500000000000002220 ) ) ;
#38839 = EDGE_CURVE ( 'NONE', #5107, #59182, #37743, .T. ) ;
#38840 = ORIENTED_EDGE ( 'NONE', *, *, #54136, .F. ) ;
#38841 = LINE ( 'NONE', #70302, #13781 ) ;
#38842 = CARTESIAN_POINT ( 'NONE',  ( -50.44065031394416820, -25.10935757545416891, 2.834208411262789884 ) ) ;
#38843 = DIRECTION ( 'NONE',  ( 1.000000000000000000, 0.000000000000000000, 0.000000000000000000 ) ) ;
#38844 = PLANE ( 'NONE',  #43692 ) ;
#38845 = DIRECTION ( 'NONE',  ( -0.000000000000000000, 1.000000000000000000, -0.000000000000000000 ) ) ;
#38846 = CARTESIAN_POINT ( 'NONE',  ( -100.5228709571500616, -25.00182538069145366, 7.747789668545101982 ) ) ;
#38848 = VERTEX_POINT ( 'NONE', #92025 ) ;
#38847 = CARTESIAN_POINT ( 'NONE',  ( -19.05511597014879044, -11.33806725510066826, 11.49999999999999645 ) ) ;
#38849 = FACE_OUTER_BOUND ( 'NONE', #24371, .T. ) ;
#38850 = EDGE_CURVE ( 'NONE', #50604, #68064, #22498, .T. ) ;
#38851 = CARTESIAN_POINT ( 'NONE',  ( -56.52287095715006870, -29.50248528299804818, 1.056150453629034924 ) ) ;
#38852 = VERTEX_POINT ( 'NONE', #94025 ) ;
#38853 = CARTESIAN_POINT ( 'NONE',  ( 10.43192878459595185, 20.09917060401269850, 11.49999999999998934 ) ) ;
#38855 = VERTEX_POINT ( 'NONE', #85410 ) ;
#38854 = CARTESIAN_POINT ( 'NONE',  ( -29.24562190895224489, -25.20408335486846951, 5.231737936259443167 ) ) ;
#38856 = ORIENTED_EDGE ( 'NONE', *, *, #5204, .F. ) ;
#38857 = DIRECTION ( 'NONE',  ( 0.000000000000000000, 0.000000000000000000, 1.000000000000000000 ) ) ;
#38858 = CC_DESIGN_DATE_AND_TIME_ASSIGNMENT ( #4339, #35289, ( #57555 ) ) ;
#38859 = CARTESIAN_POINT ( 'NONE',  ( -11.28321777122536140, 16.66956161807075887, 11.49999999999998934 ) ) ;
#38860 = B_SPLINE_SURFACE_WITH_KNOTS ( 'NONE', 3, 1, ( 
 ( #68740, #85446 ),
 ( #22535, #69232 ),
 ( #93552, #16432 ),
 ( #92065, #76332 ),
 ( #32163, #100150 ),
 ( #713, #76822 ),
 ( #46898, #30669 ),
 ( #24549, #62131 ),
 ( #7320, #8832 ),
 ( #84949, #24046 ),
 ( #61639, #55522 ),
 ( #15932, #63136 ),
 ( #93056, #37788 ),
 ( #99658, #46396 ),
 ( #23534, #39770 ) ),
 .UNSPECIFIED., .F., .F., .F.,
 ( 4, 1, 1, 1, 1, 1, 1, 1, 1, 1, 1, 1, 4 ),
 ( 2, 2 ),
 ( 0.000000000000000000, 0.08553210767726550368, 0.1690033828897672674, 0.2519432488916409363, 0.3356820104014504591, 0.4194085858192974636, 0.5012648984817446030, 0.5837029416042844865, 0.6680003590442504802, 0.7519186598620664075, 0.8345977112584781477, 0.9165256687801534019, 1.000000000000000000 ),
 ( 0.000000000000000000, 1.000000000000000000 ),
 .UNSPECIFIED. ) ;
#38861 = PLANE ( 'NONE',  #8438 ) ;
#38862 = EDGE_LOOP ( 'NONE', ( #45262, #21782, #47479, #38687 ) ) ;
#38863 = PLANE ( 'NONE',  #65018 ) ;
#38864 = CARTESIAN_POINT ( 'NONE',  ( 8.681249458320607459, -20.60847208623538762, -1.500000000000002220 ) ) ;
#38865 = ORIENTED_EDGE ( 'NONE', *, *, #48309, .F. ) ;
#38866 = ORIENTED_EDGE ( 'NONE', *, *, #15538, .T. ) ;
#38867 = DIRECTION ( 'NONE',  ( -1.000000000000000000, 0.000000000000000000, 0.000000000000000000 ) ) ;
#38868 = CARTESIAN_POINT ( 'NONE',  ( 32.16024265030974050, 5.965225279485572685, 14.03360796525321774 ) ) ;
#38869 = DIRECTION ( 'NONE',  ( 0.000000000000000000, 0.000000000000000000, 1.000000000000000000 ) ) ;
#38870 = CARTESIAN_POINT ( 'NONE',  ( -116.5228709571500616, -24.64965694238575011, 8.947790433994191162 ) ) ;
#38871 = CARTESIAN_POINT ( 'NONE',  ( -30.61345265565988782, -24.26743686635980524, 0.04347934593174110351 ) ) ;
#38872 = CARTESIAN_POINT ( 'NONE',  ( 12.07855387261060898, -15.37489856218140183, -1.500000000000002220 ) ) ;
#38873 = DIRECTION ( 'NONE',  ( -0.9940716917543757081, 0.000000000000000000, -0.1087265912856348327 ) ) ;
#38874 = CARTESIAN_POINT ( 'NONE',  ( 8.900169022907615357, -19.58186849131130813, -1.500000000000002220 ) ) ;
#38875 = LINE ( 'NONE', #31772, #5826 ) ;
#38876 = FACE_OUTER_BOUND ( 'NONE', #56464, .T. ) ;
#38878 = B_SPLINE_CURVE_WITH_KNOTS ( 'NONE', 3,
 ( #37857, #6904, #70813, #92631 ),
 .UNSPECIFIED., .F., .F.,
 ( 4, 4 ),
 ( 3.130749735702545926E-09, 0.004340662820791676285 ),
 .UNSPECIFIED. ) ;
#38877 = PLANE ( 'NONE',  #2059 ) ;
#38879 = CIRCLE ( 'NONE', #46926, 2.500000000000002220 ) ;
#38880 = CARTESIAN_POINT ( 'NONE',  ( -107.5228709571500758, -23.47596703998600631, 11.44779298504228038 ) ) ;
#38881 = CARTESIAN_POINT ( 'NONE',  ( -20.58715743568940226, -9.973749938417524774, -1.500000000000002220 ) ) ;
#38882 = CALENDAR_DATE ( 2026, 9, 10 ) ;
#38883 = DIRECTION ( 'NONE',  ( -0.000000000000000000, 1.000000000000000000, -0.000000000000000000 ) ) ;
#38884 = CARTESIAN_POINT ( 'NONE',  ( -2.750773227259631692, -5.876774720514414518, 19.84584863393302001 ) ) ;
#38885 = CARTESIAN_POINT ( 'NONE',  ( 19.70663390988245922, 3.666079223618853966, 11.49999999999999645 ) ) ;
#38886 = CARTESIAN_POINT ( 'NONE',  ( -109.6228709571500559, -24.66019654487199730, 8.947790411086124607 ) ) ;
#38887 = DIRECTION ( 'NONE',  ( -1.000000000000000000, -0.000000000000000000, -0.000000000000000000 ) ) ;
#38888 = AXIS2_PLACEMENT_3D ( 'NONE', #36702, #29082, #14846 ) ;
#38889 = CARTESIAN_POINT ( 'NONE',  ( 4.039061187531148178, -5.876774720514401196, 18.18637930035166761 ) ) ;
#38890 = CARTESIAN_POINT ( 'NONE',  ( -103.5562042904833930, -24.64898659630528854, 1.056161002820824590 ) ) ;
#38891 = EDGE_CURVE ( 'NONE', #61060, #54056, #84819, .T. ) ;
#38892 = ORIENTED_EDGE ( 'NONE', *, *, #25418, .T. ) ;
#38893 = CARTESIAN_POINT ( 'NONE',  ( -50.62287095715007013, -24.92604778743017491, 8.074972756849360778 ) ) ;
#38894 = CARTESIAN_POINT ( 'NONE',  ( -110.3139465455115129, -25.11033443737754212, 2.832404817301930056 ) ) ;
#38895 = CARTESIAN_POINT ( 'NONE',  ( 6.829227106855087825, -20.66181959361685827, 11.49999999999998934 ) ) ;
#38896 = CARTESIAN_POINT ( 'NONE',  ( -58.52287095715006160, -29.50248528299804818, 1.056150453629034924 ) ) ;
#38897 = VECTOR ( 'NONE', #77895, 1000.000000000000114 ) ;
#38898 = CARTESIAN_POINT ( 'NONE',  ( -16.92291128558595048, 9.936001969431544012, -1.500000000000002220 ) ) ;
#38899 = DIRECTION ( 'NONE',  ( 0.000000000000000000, 0.9999999999976377785, 2.173523156925979975E-06 ) ) ;
#38900 = B_SPLINE_CURVE_WITH_KNOTS ( 'NONE', 3,
 ( #35143, #81806, #43257, #49881, #19399, #57992 ),
 .UNSPECIFIED., .F., .F.,
 ( 4, 2, 4 ),
 ( 1.570887131794638196E-05, 0.001396322306279761073, 0.002776935741241575838 ),
 .UNSPECIFIED. ) ;
#38901 = VECTOR ( 'NONE', #62830, 1000.000000000000114 ) ;
#38902 = CARTESIAN_POINT ( 'NONE',  ( -109.3584176993576591, -25.27925665775238073, 4.206202527071893904 ) ) ;
#38903 = EDGE_CURVE ( 'NONE', #31485, #35718, #29193, .T. ) ;
#38904 = VECTOR ( 'NONE', #14580, 1000.000000000000114 ) ;
#38905 = CARTESIAN_POINT ( 'NONE',  ( -5.366453405989236813, 0.000000000000000000, 0.000000000000000000 ) ) ;
#38906 = CARTESIAN_POINT ( 'NONE',  ( 2.745953332610513442, -5.876774720514418959, 21.05053573504278575 ) ) ;
#38907 = CARTESIAN_POINT ( 'NONE',  ( -3.210669876418242197, 20.33209092710186638, 11.49999999999999645 ) ) ;
#38908 = CARTESIAN_POINT ( 'NONE',  ( 30.61004588589006659, 4.070814610512477394, 27.12580813198458785 ) ) ;
#38909 = EDGE_CURVE ( 'NONE', #59077, #91381, #41253, .T. ) ;
#38910 = CARTESIAN_POINT ( 'NONE',  ( -120.5181857807525745, -24.52300882791530512, 0.6510814631126412566 ) ) ;
#38911 = VECTOR ( 'NONE', #47360, 1000.000000000000114 ) ;
#38912 = VERTEX_POINT ( 'NONE', #25522 ) ;
#38913 = CARTESIAN_POINT ( 'NONE',  ( -70.22494714645260672, -25.12219144110276048, 7.098707458017251781 ) ) ;
#38914 = CARTESIAN_POINT ( 'NONE',  ( 2.899999999999999467, 33.29999999999999716, 2.100000000000000089 ) ) ;
#38915 = DIRECTION ( 'NONE',  ( 1.000000000000000000, 0.000000000000000000, 0.000000000000000000 ) ) ;
#38916 = CARTESIAN_POINT ( 'NONE',  ( -19.77875734969026311, 5.356774720514426491, 27.45402280011862217 ) ) ;
#38917 = EDGE_CURVE ( 'NONE', #36701, #63790, #37823, .T. ) ;
#38918 = CARTESIAN_POINT ( 'NONE',  ( -25.88669879221086134, -24.93063363318205461, 7.002165060778218653 ) ) ;
#38919 = PLANE ( 'NONE',  #86876 ) ;
#38920 = CARTESIAN_POINT ( 'NONE',  ( 5.395019145045520048, -22.42585393411717121, 11.49999999999999645 ) ) ;
#38921 = CARTESIAN_POINT ( 'NONE',  ( 22.20067557195093855, 5.203973054738295190, -1.500000000000002220 ) ) ;
#38922 = CARTESIAN_POINT ( 'NONE',  ( -74.63458474643041995, -24.15543982623907127, -0.2315651400026650930 ) ) ;
#38923 = CARTESIAN_POINT ( 'NONE',  ( -88.52287095715004739, -23.96127896941632329, -0.6493128931038041340 ) ) ;
#38924 = CARTESIAN_POINT ( 'NONE',  ( -119.5562042904834072, -24.64898659630529210, 1.056161002820831696 ) ) ;
#38925 = CARTESIAN_POINT ( 'NONE',  ( 22.03792223356247604, -4.036589945906135846, 11.49999999999999645 ) ) ;
#38926 = ORIENTED_EDGE ( 'NONE', *, *, #51529, .T. ) ;
#38927 = CARTESIAN_POINT ( 'NONE',  ( -69.55620429048339304, -24.65952944569304606, 1.056160979905699016 ) ) ;
#38928 = CARTESIAN_POINT ( 'NONE',  ( -34.62287095715005592, -24.64965695001467694, 8.947790433994189385 ) ) ;
#38929 = CARTESIAN_POINT ( 'NONE',  ( 1.885617179787854036, 21.85875792104173598, -1.500000000000002220 ) ) ;
#38930 = PLANE ( 'NONE',  #13768 ) ;
#38931 = CARTESIAN_POINT ( 'NONE',  ( 32.53346577320678534, 0.6027747205144262654, -11.93731717363831102 ) ) ;
#38932 = CARTESIAN_POINT ( 'NONE',  ( -56.58953762381673158, -23.48786465467241413, 11.44779295918254824 ) ) ;
#38933 = CARTESIAN_POINT ( 'NONE',  ( -78.54308978932711227, -24.51314013834315375, 0.6176544820404143987 ) ) ;
#38934 = CARTESIAN_POINT ( 'NONE',  ( -112.6228709571500417, -24.66019654487199730, 8.947790411086124607 ) ) ;
#38935 = ORIENTED_EDGE ( 'NONE', *, *, #15077, .T. ) ;
#38936 = CARTESIAN_POINT ( 'NONE',  ( -15.50425215161893355, 13.37805140191733777, -1.500000000000002220 ) ) ;
#38937 = VERTEX_POINT ( 'NONE', #16904 ) ;
#38938 = VERTEX_POINT ( 'NONE', #78787 ) ;
#38939 = ORIENTED_EDGE ( 'NONE', *, *, #54743, .T. ) ;
#38940 = ORIENTED_EDGE ( 'NONE', *, *, #75302, .F. ) ;
#38941 = CARTESIAN_POINT ( 'NONE',  ( -22.22199965279648737, -6.226755796435518242, -1.500000000000002220 ) ) ;
#38942 = CARTESIAN_POINT ( 'NONE',  ( -49.10457154551149728, -25.27419814425984512, 3.999772249604824914 ) ) ;
#38943 = CARTESIAN_POINT ( 'NONE',  ( 17.44645523915803764, -10.38078700900905993, -1.500000000000002220 ) ) ;
#38944 = ORIENTED_EDGE ( 'NONE', *, *, #56545, .T. ) ;
#38945 = CARTESIAN_POINT ( 'NONE',  ( 19.75748517575715368, 5.965225279485572685, 28.87153971905864580 ) ) ;
#38946 = CARTESIAN_POINT ( 'NONE',  ( -92.62814048523338784, -24.34968618360935011, 0.1864209137778965741 ) ) ;
#38947 = EDGE_CURVE ( 'NONE', #39863, #11676, #99384, .T. ) ;
#38948 = DIRECTION ( 'NONE',  ( 0.000000000000000000, -0.000000000000000000, -1.000000000000000000 ) ) ;
#38949 = CARTESIAN_POINT ( 'NONE',  ( -70.55210020511036362, -24.15503026093916006, -0.2815557561904372674 ) ) ;
#38951 = ORIENTED_EDGE ( 'NONE', *, *, #76220, .T. ) ;
#38950 = CARTESIAN_POINT ( 'NONE',  ( -20.95461191387366284, 4.708766595171775649, 11.49999999999999645 ) ) ;
#38952 = CARTESIAN_POINT ( 'NONE',  ( -75.58685686046939622, -24.63355581998385802, 0.9682620441943947664 ) ) ;
#38953 = CARTESIAN_POINT ( 'NONE',  ( -61.51535964669244549, -23.73791477778911840, 11.05961554403170766 ) ) ;
#38954 = EDGE_LOOP ( 'NONE', ( #92618, #6920 ) ) ;
#38955 = CARTESIAN_POINT ( 'NONE',  ( 17.22178217532253086, -11.58000449095910867, 11.49999999999998934 ) ) ;
#38956 = VECTOR ( 'NONE', #30201, 1000.000000000000114 ) ;
#38957 = ORIENTED_EDGE ( 'NONE', *, *, #69534, .T. ) ;
#38959 = VERTEX_POINT ( 'NONE', #86915 ) ;
#38958 = DIRECTION ( 'NONE',  ( 3.639962309748244178E-15, -1.000000000000000000, -2.135627652102599075E-15 ) ) ;
#38960 = EDGE_CURVE ( 'NONE', #39939, #13092, #6187, .T. ) ;
#38961 = CARTESIAN_POINT ( 'NONE',  ( -111.5158189371944104, -24.35071581493544457, 9.817618358456018157 ) ) ;
#38962 = CARTESIAN_POINT ( 'NONE',  ( -48.52287095715006160, -24.65952944569304606, 1.056160979905693686 ) ) ;
#38963 = ORIENTED_EDGE ( 'NONE', *, *, #2752, .T. ) ;
#38964 = ORIENTED_EDGE ( 'NONE', *, *, #19528, .F. ) ;
#38965 = CARTESIAN_POINT ( 'NONE',  ( 4.115763745420833786, -5.876774720514401196, 18.20859014712428348 ) ) ;
#38966 = CARTESIAN_POINT ( 'NONE',  ( -42.55305635006578058, -23.96169478059712787, 10.65365249895718947 ) ) ;
#38967 = B_SPLINE_CURVE_WITH_KNOTS ( 'NONE', 3,
 ( #81729, #43669, #13699, #44674 ),
 .UNSPECIFIED., .F., .F.,
 ( 4, 4 ),
 ( 1.387778780781445521E-17, 9.999999999998898659E-05 ),
 .UNSPECIFIED. ) ;
#38968 = DIRECTION ( 'NONE',  ( 0.000000000000000000, 1.000000000000000000, 0.000000000000000000 ) ) ;
#38969 = CARTESIAN_POINT ( 'NONE',  ( -15.57331531552114612, -15.56871402003811333, 11.49999999999999645 ) ) ;
#38970 = DIRECTION ( 'NONE',  ( 0.000000000000000000, 3.563215788492900483E-15, -1.000000000000000000 ) ) ;
#38971 = CARTESIAN_POINT ( 'NONE',  ( 16.93931825803137414, 14.88162037096512158, 11.49999999999998934 ) ) ;
#38972 = CARTESIAN_POINT ( 'NONE',  ( 20.40321384664088811, -4.974606123342796060, 11.49999999999998934 ) ) ;
#38973 = CARTESIAN_POINT ( 'NONE',  ( 6.431189903846153300, -6.376774720514415407, 20.08974358974358765 ) ) ;
#38974 = ORIENTED_EDGE ( 'NONE', *, *, #9811, .T. ) ;
#38975 = AXIS2_PLACEMENT_3D ( 'NONE', #79551, #88675, #18644 ) ;
#38976 = ORIENTED_EDGE ( 'NONE', *, *, #26020, .T. ) ;
#38977 = AXIS2_PLACEMENT_3D ( 'NONE', #48830, #79756, #65071 ) ;
#38978 = CARTESIAN_POINT ( 'NONE',  ( -32.52287095715006160, -23.48786465467240347, 11.44779295918255357 ) ) ;
#38979 = EDGE_CURVE ( 'NONE', #82227, #48546, #93340, .T. ) ;
#38980 = VECTOR ( 'NONE', #49263, 1000.000000000000114 ) ;
#38981 = CARTESIAN_POINT ( 'NONE',  ( -90.62287095715005592, -24.82576562982392687, 8.398263435472967942 ) ) ;
#38982 = ORIENTED_EDGE ( 'NONE', *, *, #16919, .F. ) ;
#38983 = CARTESIAN_POINT ( 'NONE',  ( 9.152908845159860363, 19.05633030926415472, -1.500000000000002220 ) ) ;
#38984 = CARTESIAN_POINT ( 'NONE',  ( 282.9764569301858046, -5.965225279485572685, 20.79159422840526616 ) ) ;
#38985 = CARTESIAN_POINT ( 'NONE',  ( -51.06671402896819956, -25.26041094286820154, 7.458179734008862916 ) ) ;
#38986 = CARTESIAN_POINT ( 'NONE',  ( -49.64242587230348391, -25.29033691608420398, 4.386389768557750202 ) ) ;
#38987 = DIRECTION ( 'NONE',  ( -3.773278334453080206E-23, 0.9999999999976377785, 2.173523156925979975E-06 ) ) ;
#38988 = LINE ( 'NONE', #47617, #32456 ) ;
#38989 = CARTESIAN_POINT ( 'NONE',  ( 19.07224962250127831, -11.27678277851665634, -1.500000000000002220 ) ) ;
#38990 = CARTESIAN_POINT ( 'NONE',  ( -71.62697868567160242, -24.51314013834315730, 0.6176544820404130665 ) ) ;
#38991 = EDGE_LOOP ( 'NONE', ( #100405, #93884, #18263, #27623 ) ) ;
#38992 = CARTESIAN_POINT ( 'NONE',  ( -51.88058966555665563, -25.31633273641005388, 5.810524250483315001 ) ) ;
#38993 = CARTESIAN_POINT ( 'NONE',  ( 22.81105451610979173, 8.475225279485572472, -18.46691820600746681 ) ) ;
#38994 = CARTESIAN_POINT ( 'NONE',  ( -126.5212072554304541, -24.15543982623907482, -0.2315651400026573492 ) ) ;
#38995 = EDGE_CURVE ( 'NONE', #54673, #96355, #16394, .T. ) ;
#38996 = ADVANCED_FACE ( 'NONE', ( #1693 ), #25010, .F. ) ;
#38997 = CARTESIAN_POINT ( 'NONE',  ( 4.784292611718076849, 5.356774720514425603, -25.54547254883186014 ) ) ;
#38998 = CARTESIAN_POINT ( 'NONE',  ( -33.62287095715003460, -24.33927499327853639, 9.819080762295824272 ) ) ;
#38999 = CARTESIAN_POINT ( 'NONE',  ( 19.29218144733592055, -2.436590042558338443, -1.500000000000002220 ) ) ;
#39000 = EDGE_CURVE ( 'NONE', #42693, #66086, #34575, .T. ) ;
#39001 = CARTESIAN_POINT ( 'NONE',  ( 20.92345209525186078, -4.499874906010187026, 11.49999999999998934 ) ) ;
#39002 = CARTESIAN_POINT ( 'NONE',  ( 21.57151214508649772, 3.625915217019311583E-15, 0.5000000000000000000 ) ) ;
#39003 = CARTESIAN_POINT ( 'NONE',  ( -60.61726691528298971, -23.48786465467241058, 11.44779295918254824 ) ) ;
#39004 = CARTESIAN_POINT ( 'NONE',  ( -51.59924294399129963, -23.96119346886880663, -0.6495511937832119109 ) ) ;
#39005 = CARTESIAN_POINT ( 'NONE',  ( -100.5840138597264826, -25.18440012323539179, 3.299226137916170920 ) ) ;
#39006 = CARTESIAN_POINT ( 'NONE',  ( 17.32531159343115945, 14.66459048539768162, -1.500000000000002220 ) ) ;
#39007 = LINE ( 'NONE', #15671, #53190 ) ;
#39008 = CARTESIAN_POINT ( 'NONE',  ( 31.63608488009065667, 6.376774720514426953, 27.34773273846995068 ) ) ;
#39009 = CARTESIAN_POINT ( 'NONE',  ( 15.56394622224390645, 12.30447529683395125, 11.49999999999999645 ) ) ;
#39010 = CARTESIAN_POINT ( 'NONE',  ( -51.62287095715005592, -23.47596703998600631, 11.44779298504227505 ) ) ;
#39011 = CARTESIAN_POINT ( 'NONE',  ( -59.56094173781918499, -25.20074414198133539, 3.409327697718782080 ) ) ;
#39012 = EDGE_CURVE ( 'NONE', #45125, #51264, #33131, .T. ) ;
#39013 = B_SPLINE_CURVE_WITH_KNOTS ( 'NONE', 3,
 ( #28487, #89896, #36600, #20363 ),
 .UNSPECIFIED., .F., .F.,
 ( 4, 4 ),
 ( 0.000000000000000000, 9.999999999998897304E-05 ),
 .UNSPECIFIED. ) ;
#39014 = ORIENTED_EDGE ( 'NONE', *, *, #4975, .T. ) ;
#39015 = DIRECTION ( 'NONE',  ( -0.000000000000000000, 1.000000000000000000, -0.000000000000000000 ) ) ;
#39016 = CARTESIAN_POINT ( 'NONE',  ( -5.941268476065055815, -6.376774720514417183, 20.11414146978959749 ) ) ;
#39017 = CARTESIAN_POINT ( 'NONE',  ( -115.5562042904833930, -25.00158670708909625, 2.256160236439166855 ) ) ;
#39018 = CARTESIAN_POINT ( 'NONE',  ( 17.85095790706337127, 12.24325521369631176, 11.49999999999998934 ) ) ;
#39019 = CARTESIAN_POINT ( 'NONE',  ( -56.48828734240129990, -24.66019654487199375, 8.947790411086122830 ) ) ;
#39020 = CARTESIAN_POINT ( 'NONE',  ( -0.1161231997828221785, -19.40653004597026410, -1.500000000000002220 ) ) ;
#39022 = CARTESIAN_POINT ( 'NONE',  ( -55.48852725927024920, -24.63419186844611986, 9.035850630976923981 ) ) ;
#39021 = B_SPLINE_CURVE_WITH_KNOTS ( 'NONE', 3,
 ( #38501, #46121, #13647, #14149 ),
 .UNSPECIFIED., .F., .F.,
 ( 4, 4 ),
 ( 0.000000000000000000, 1.000000000000000000 ),
 .UNSPECIFIED. ) ;
#39023 = CARTESIAN_POINT ( 'NONE',  ( 1.158388978951967463, 19.79969207489630634, -1.500000000000002220 ) ) ;
#39024 = ORIENTED_EDGE ( 'NONE', *, *, #37289, .F. ) ;
#39025 = B_SPLINE_CURVE_WITH_KNOTS ( 'NONE', 3,
 ( #9554, #86181, #40522, #79568, #47635, #32903, #32398, #94287 ),
 .UNSPECIFIED., .F., .F.,
 ( 4, 2, 2, 4 ),
 ( -0.001224554619866341076, -0.0002241820295893607630, 0.0007761905606876195497, 0.002776935741241580175 ),
 .UNSPECIFIED. ) ;
#39026 = CARTESIAN_POINT ( 'NONE',  ( -0.5597704280004801580, 20.37679164443051505, 11.49999999999999645 ) ) ;
#39027 = CARTESIAN_POINT ( 'NONE',  ( -80.49410119740149128, -24.92564183028979130, 1.928384488918253536 ) ) ;
#39028 = AXIS2_PLACEMENT_3D ( 'NONE', #10015, #80028, #28740 ) ;
#39029 = ADVANCED_FACE ( 'NONE', ( #48367 ), #79297, .T. ) ;
#39030 = DIRECTION ( 'NONE',  ( -3.773278334453079030E-23, 0.9999999999976377785, 2.173523156925979128E-06 ) ) ;
#39031 = EDGE_CURVE ( 'NONE', #81379, #32756, #86174, .T. ) ;
#39032 = ORIENTED_EDGE ( 'NONE', *, *, #82578, .T. ) ;
#39033 = CARTESIAN_POINT ( 'NONE',  ( -79.53077639109011443, -25.09533482913100499, 7.254442253322116230 ) ) ;
#39034 = LINE ( 'NONE', #53775, #76847 ) ;
#39035 = CARTESIAN_POINT ( 'NONE',  ( -49.43920486724100982, -25.31601856400028794, 5.121422751188677402 ) ) ;
#39036 = CARTESIAN_POINT ( 'NONE',  ( -66.52287095715006160, -29.50250786944525672, 11.44777988621623699 ) ) ;
#39037 = CARTESIAN_POINT ( 'NONE',  ( -0.6227173540047638012, -5.876774720514413630, 19.48351902941045211 ) ) ;
#39038 = CARTESIAN_POINT ( 'NONE',  ( 5.780499401231428358, -19.25771307485560158, 11.49999999999998934 ) ) ;
#39039 = ADVANCED_FACE ( 'NONE', ( #31624, #39737 ), #70693, .F. ) ;
#39040 = PLANE ( 'NONE',  #46815 ) ;
#39041 = ORIENTED_EDGE ( 'NONE', *, *, #82193, .F. ) ;
#39042 = CARTESIAN_POINT ( 'NONE',  ( -91.62287095715005592, -23.48786465467241769, 11.44779295918254114 ) ) ;
#39043 = ADVANCED_FACE ( 'NONE', ( #9793 ), #71704, .F. ) ;
#39044 = AXIS2_PLACEMENT_3D ( 'NONE', #84422, #61104, #24015 ) ;
#39045 = CARTESIAN_POINT ( 'NONE',  ( 10.67403711042701353, -20.27515232684288549, 11.49999999999999645 ) ) ;
#39046 = CARTESIAN_POINT ( 'NONE',  ( 6.262736145392394427, -21.83385498489561272, -1.500000000000002220 ) ) ;
#39047 = VERTEX_POINT ( 'NONE', #97030 ) ;
#39048 = CARTESIAN_POINT ( 'NONE',  ( -45.52287095715006160, -25.00158670708908915, 2.256160236439166411 ) ) ;
#39049 = LINE ( 'NONE', #77098, #47771 ) ;
#39050 = CARTESIAN_POINT ( 'NONE',  ( -39.48084026492560383, -25.26931200938422961, 3.940603736575979177 ) ) ;
#39051 = CARTESIAN_POINT ( 'NONE',  ( -30.57287095715006942, -23.79114969660752621, -0.9649529075300503633 ) ) ;
#39052 = CARTESIAN_POINT ( 'NONE',  ( -128.6235869392866675, -24.51419770103157703, 9.386484678747171628 ) ) ;
#39053 = B_SPLINE_CURVE_WITH_KNOTS ( 'NONE', 3,
 ( #27491, #96992, #59947, #34604 ),
 .UNSPECIFIED., .F., .F.,
 ( 4, 4 ),
 ( 0.000000000000000000, 9.999999999997510880E-05 ),
 .UNSPECIFIED. ) ;
#39054 = DIRECTION ( 'NONE',  ( -0.000000000000000000, 0.000000000000000000, 1.000000000000000000 ) ) ;
#39055 = ORIENTED_EDGE ( 'NONE', *, *, #32360, .T. ) ;
#39056 = CARTESIAN_POINT ( 'NONE',  ( 14.85214116200856083, 13.97194181870810326, -1.500000000000002220 ) ) ;
#39057 = ORIENTED_EDGE ( 'NONE', *, *, #98670, .F. ) ;
#39058 = CARTESIAN_POINT ( 'NONE',  ( -19.99251892732797486, -11.32171818645973538, -1.500000000000002220 ) ) ;
#39059 = FACE_OUTER_BOUND ( 'NONE', #16987, .T. ) ;
#39060 = ORIENTED_EDGE ( 'NONE', *, *, #5340, .T. ) ;
#39061 = CARTESIAN_POINT ( 'NONE',  ( -101.2818275285644773, -25.17579918040796372, 6.774827964654662971 ) ) ;
#39062 = CARTESIAN_POINT ( 'NONE',  ( 13.57151214508650305, -0.8999999999999998002, 0.000000000000000000 ) ) ;
#39063 = ADVANCED_FACE ( 'NONE', ( #28024 ), #51361, .T. ) ;
#39064 = CARTESIAN_POINT ( 'NONE',  ( -111.5228709571500758, -23.72773821059536914, 11.05748984161097326 ) ) ;
#39066 = ORIENTED_EDGE ( 'NONE', *, *, #69351, .T. ) ;
#39065 = CARTESIAN_POINT ( 'NONE',  ( -21.31669061289120037, -0.5855882196083471714, 11.49999999999999645 ) ) ;
#39067 = VERTEX_POINT ( 'NONE', #96529 ) ;
#39068 = CARTESIAN_POINT ( 'NONE',  ( 16.02632597834478645, 15.35701383120132313, -1.500000000000002220 ) ) ;
#39069 = CARTESIAN_POINT ( 'NONE',  ( 11.79242832063081892, -16.95861370568002613, 11.49999999999998934 ) ) ;
#39070 = ORIENTED_EDGE ( 'NONE', *, *, #86314, .T. ) ;
#39071 = EDGE_LOOP ( 'NONE', ( #82038, #81256, #99714, #55187 ) ) ;
#39072 = ADVANCED_FACE ( 'NONE', ( #87925 ), #43749, .F. ) ;
#39073 = CARTESIAN_POINT ( 'NONE',  ( -109.1951039547969202, -25.27682750245845611, 4.973674001946442935 ) ) ;
#39074 = CARTESIAN_POINT ( 'NONE',  ( -69.86008333542852711, -25.11539253604531297, 2.804427796191110378 ) ) ;
#39075 = ORIENTED_EDGE ( 'NONE', *, *, #23318, .T. ) ;
#39076 = FACE_OUTER_BOUND ( 'NONE', #78252, .T. ) ;
#39077 = VERTEX_POINT ( 'NONE', #66613 ) ;
#39078 = FACE_OUTER_BOUND ( 'NONE', #16580, .T. ) ;
#39079 = FACE_OUTER_BOUND ( 'NONE', #4277, .T. ) ;
#39080 = CARTESIAN_POINT ( 'NONE',  ( -17.17656601037699104, 11.78060583124977256, -1.500000000000002220 ) ) ;
#39081 = CARTESIAN_POINT ( 'NONE',  ( 21.36706796925463792, 4.321743776461201669, 11.49999999999999645 ) ) ;
#39082 = CARTESIAN_POINT ( 'NONE',  ( -84.62287095715005592, -24.64965695001469115, 8.947790433994182280 ) ) ;
#39083 = CARTESIAN_POINT ( 'NONE',  ( -28.98875734969026041, -5.965225279485572685, 25.61802280011862720 ) ) ;
#39084 = CARTESIAN_POINT ( 'NONE',  ( -22.33494257564923302, 2.542849975942539587, 11.49999999999998934 ) ) ;
#39085 = CARTESIAN_POINT ( 'NONE',  ( -118.5933811847046684, -23.48786465467241769, 11.44779295918253581 ) ) ;
#39086 = DIRECTION ( 'NONE',  ( 0.6599726524652352877, 0.000000000000000000, -0.7512896232465891000 ) ) ;
#39087 = CARTESIAN_POINT ( 'NONE',  ( -31.62287095715005236, -24.64965695001467694, 8.947790433994189385 ) ) ;
#39088 = ORIENTED_EDGE ( 'NONE', *, *, #18191, .F. ) ;
#39089 = ORIENTED_EDGE ( 'NONE', *, *, #65844, .F. ) ;
#39090 = CIRCLE ( 'NONE', #66655, 1.249999999999997558 ) ;
#39091 = VERTEX_POINT ( 'NONE', #42277 ) ;
#39092 = EDGE_CURVE ( 'NONE', #57212, #19469, #89689, .T. ) ;
#39093 = CARTESIAN_POINT ( 'NONE',  ( 18.61059577090848549, -10.47110149595715711, -1.500000000000002220 ) ) ;
#39094 = ORIENTED_EDGE ( 'NONE', *, *, #98079, .T. ) ;
#39095 = CARTESIAN_POINT ( 'NONE',  ( -20.60145385712877797, -4.430719527714695793, 11.49999999999998934 ) ) ;
#39096 = LINE ( 'NONE', #31992, #54654 ) ;
#39097 = CARTESIAN_POINT ( 'NONE',  ( -19.25010300378637851, 5.133817055790010464, -1.500000000000002220 ) ) ;
#39098 = CARTESIAN_POINT ( 'NONE',  ( -117.6228709571500417, -24.65952944569305316, 1.056160979905706121 ) ) ;
#39099 = CARTESIAN_POINT ( 'NONE',  ( 2.904244945035652670, -5.876774720514415407, 20.04207437776001299 ) ) ;
#39100 = CARTESIAN_POINT ( 'NONE',  ( 0.3405503412851532130, 21.98688381012616233, -1.500000000000002220 ) ) ;
#39101 = CARTESIAN_POINT ( 'NONE',  ( -107.6228709571500701, -29.50248528299804818, 1.056150453629043584 ) ) ;
#39102 = ORIENTED_EDGE ( 'NONE', *, *, #64574, .F. ) ;
#39103 = DIRECTION ( 'NONE',  ( 1.000000000000000000, 3.773278334444166432E-23, 8.201307841325785021E-29 ) ) ;
#39104 = EDGE_CURVE ( 'NONE', #77838, #34072, #38900, .T. ) ;
#39105 = CARTESIAN_POINT ( 'NONE',  ( -32.30247028140506416, -6.475225279485573360, 27.60502002861223048 ) ) ;
#39106 = CARTESIAN_POINT ( 'NONE',  ( -10.15938669249390180, 18.18672505111813464, 11.49999999999999645 ) ) ;
#39107 = EDGE_CURVE ( 'NONE', #11909, #72410, #40166, .T. ) ;
#39108 = ADVANCED_FACE ( 'NONE', ( #82301 ), #61365, .T. ) ;
#39109 = CARTESIAN_POINT ( 'NONE',  ( 29.77147767949870882, -6.376774720514427841, 26.15915692125050995 ) ) ;
#39110 = VECTOR ( 'NONE', #37273, 1000.000000000000000 ) ;
#39111 = DIRECTION ( 'NONE',  ( 1.000000000000000000, 3.773278334444166432E-23, 8.201307841325785021E-29 ) ) ;
#39112 = EDGE_CURVE ( 'NONE', #64811, #10184, #13557, .T. ) ;
#39113 = CARTESIAN_POINT ( 'NONE',  ( -30.65075040189094580, -23.47621662958674804, 11.44779298504228215 ) ) ;
#39114 = CARTESIAN_POINT ( 'NONE',  ( -13.45305159987462851, 16.49040971879131234, 11.49999999999998934 ) ) ;
#39115 = CARTESIAN_POINT ( 'NONE',  ( -126.5228709571500616, -24.66019654487200441, 8.947790411086108620 ) ) ;
#39116 = CARTESIAN_POINT ( 'NONE',  ( -27.47983700607433732, -24.97064404397603710, 2.285865536977212731 ) ) ;
#39117 = CARTESIAN_POINT ( 'NONE',  ( -12.84880425037203011, 5.965225279485592225, -26.59900746623528534 ) ) ;
#39118 = DIRECTION ( 'NONE',  ( 0.000000000000000000, -2.173523156925979552E-06, 0.9999999999976378895 ) ) ;
#39119 = CARTESIAN_POINT ( 'NONE',  ( 19.77564376705174709, 10.73071584254150856, -1.500000000000002220 ) ) ;
#39120 = CARTESIAN_POINT ( 'NONE',  ( -109.9080821080480348, -25.30561928443788133, 5.929683345795315752 ) ) ;
#39121 = VERTEX_POINT ( 'NONE', #83791 ) ;
#39122 = CARTESIAN_POINT ( 'NONE',  ( -51.36387381899343296, -25.29840739023615015, 5.660634689548093235 ) ) ;
#39123 = CARTESIAN_POINT ( 'NONE',  ( 3.672440828437461224, -6.376774720514402972, 18.52532110411518573 ) ) ;
#39124 = CARTESIAN_POINT ( 'NONE',  ( 11.96684523812195700, 15.63349346248531546, 11.49999999999999645 ) ) ;
#39125 = DIRECTION ( 'NONE',  ( 1.257682986112628908E-16, 0.000000000000000000, 1.000000000000000000 ) ) ;
#39126 = CARTESIAN_POINT ( 'NONE',  ( -32.52287095715006160, -23.48786465467240347, 11.44779295918255357 ) ) ;
#39127 = EDGE_CURVE ( 'NONE', #37466, #87003, #74684, .T. ) ;
#39128 = ADVANCED_FACE ( 'NONE', ( #99504 ), #28899, .T. ) ;
#39129 = ORIENTED_EDGE ( 'NONE', *, *, #82637, .T. ) ;
#39130 = CARTESIAN_POINT ( 'NONE',  ( -99.54653831362026040, -24.65952944569304961, 1.056160979905703901 ) ) ;
#39131 = CARTESIAN_POINT ( 'NONE',  ( -127.4337102941773310, -25.40067779903719014, 5.393965687396610420 ) ) ;
#39132 = CARTESIAN_POINT ( 'NONE',  ( -88.86967830683752823, -25.30572777988223976, 5.920366768842380445 ) ) ;
#39133 = CARTESIAN_POINT ( 'NONE',  ( -10.11875734969026297, 3.316774720514426456, 30.51402280011862089 ) ) ;
#39135 = EDGE_CURVE ( 'NONE', #7254, #58462, #37636, .T. ) ;
#39134 = CARTESIAN_POINT ( 'NONE',  ( 10.86211995951333620, 16.47970581058804740, 11.49999999999998934 ) ) ;
#39136 = EDGE_LOOP ( 'NONE', ( #27519, #97344, #90362, #96361 ) ) ;
#39137 = CARTESIAN_POINT ( 'NONE',  ( -109.3600754929479990, -25.28541744376511247, 4.143928178231703008 ) ) ;
#39138 = EDGE_CURVE ( 'NONE', #71832, #54301, #75196, .T. ) ;
#39139 = AXIS2_PLACEMENT_3D ( 'NONE', #43368, #35752, #73803 ) ;
#39140 = PERSON_AND_ORGANIZATION ( #70597, #27821 ) ;
#39141 = ORIENTED_EDGE ( 'NONE', *, *, #38478, .F. ) ;
#39142 = DIRECTION ( 'NONE',  ( 0.000000000000000000, -1.000000000000000000, 0.000000000000000000 ) ) ;
#39143 = DIRECTION ( 'NONE',  ( -3.773278334453079618E-23, 0.9999999999976377785, 2.173523156925979975E-06 ) ) ;
#39144 = CARTESIAN_POINT ( 'NONE',  ( -70.23317170328631676, -25.30150784332992231, 5.317526772565525306 ) ) ;
#39145 = CARTESIAN_POINT ( 'NONE',  ( -66.52287095715007581, -24.50216790748205398, 0.6166512839542501734 ) ) ;
#39146 = DIRECTION ( 'NONE',  ( -3.773278334444167608E-23, 1.000000000000000000, 0.000000000000000000 ) ) ;
#39147 = CARTESIAN_POINT ( 'NONE',  ( 22.81105451610979173, -1.477225279485574028, -18.46691820600746681 ) ) ;
#39148 = CARTESIAN_POINT ( 'NONE',  ( 20.13489193910630703, -2.682774720514426559, -22.92085183005112370 ) ) ;
#39149 = CARTESIAN_POINT ( 'NONE',  ( 2.999408428739025023, -19.78128511538675127, 11.49999999999998934 ) ) ;
#39150 = EDGE_CURVE ( 'NONE', #57062, #49913, #63186, .T. ) ;
#39151 = CARTESIAN_POINT ( 'NONE',  ( -99.62559895716422886, -25.10935090793326907, 3.076829667107262356 ) ) ;
#39152 = CARTESIAN_POINT ( 'NONE',  ( -80.52287095715006160, -29.50247984919015209, -1.443849546365053582 ) ) ;
#39153 = ORIENTED_EDGE ( 'NONE', *, *, #2051, .T. ) ;
#39154 = ADVANCED_FACE ( 'NONE', ( #84288 ), #53858, .F. ) ;
#39155 = EDGE_CURVE ( 'NONE', #17609, #54808, #29007, .T. ) ;
#39156 = CARTESIAN_POINT ( 'NONE',  ( -79.56370193356575271, -23.48786465467241058, 11.44779295918254824 ) ) ;
#39157 = CARTESIAN_POINT ( 'NONE',  ( -110.3346797185884327, -25.29012725434539277, 3.293942888057630025 ) ) ;
#39158 = CARTESIAN_POINT ( 'NONE',  ( 0.01063402156994475850, -0.1430980438411110500, 9.000000000000000000 ) ) ;
#39159 = DIRECTION ( 'NONE',  ( -0.000000000000000000, 2.173523156925979552E-06, -0.9999999999976378895 ) ) ;
#39160 = VECTOR ( 'NONE', #12931, 1000.000000000000000 ) ;
#39161 = CARTESIAN_POINT ( 'NONE',  ( -6.660000000000001030, -10.15233964170348457, -1.303165529866009420 ) ) ;
#39162 = CARTESIAN_POINT ( 'NONE',  ( 6.660000000000001030, 8.793627758918228565, -2.994553991265763049 ) ) ;
#39163 = B_SPLINE_CURVE_WITH_KNOTS ( 'NONE', 3,
 ( #32509, #94404, #33016, #34516 ),
 .UNSPECIFIED., .F., .F.,
 ( 4, 4 ),
 ( 0.000000000000000000, 9.999999999996123101E-05 ),
 .UNSPECIFIED. ) ;
#39164 = CYLINDRICAL_SURFACE ( 'NONE', #52803, 1.050000000000000488 ) ;
#39165 = CARTESIAN_POINT ( 'NONE',  ( 5.541369867593821219, -6.376774720514426065, 21.42815349816763160 ) ) ;
#39166 = ORIENTED_EDGE ( 'NONE', *, *, #16248, .T. ) ;
#39167 = CARTESIAN_POINT ( 'NONE',  ( 5.353267490507026771, -19.58905154090721368, -1.500000000000002220 ) ) ;
#39168 = CARTESIAN_POINT ( 'NONE',  ( -114.6228709571500559, -23.47593901973091235, -1.443836447538999312 ) ) ;
#39169 = CC_DESIGN_SECURITY_CLASSIFICATION ( #37589, ( #100433 ) ) ;
#39170 = CARTESIAN_POINT ( 'NONE',  ( -40.48848276756407927, -25.18740891339376731, 6.892728034667198855 ) ) ;
#39171 = ORIENTED_EDGE ( 'NONE', *, *, #63135, .T. ) ;
#39172 = CARTESIAN_POINT ( 'NONE',  ( -115.6228709571500559, -29.50248789122583659, 2.256150453626215580 ) ) ;
#39173 = VECTOR ( 'NONE', #37032, 1000.000000000000114 ) ;
#39174 = CARTESIAN_POINT ( 'NONE',  ( 10.01938154005162218, -17.43019892170380913, -1.500000000000002220 ) ) ;
#39175 = CARTESIAN_POINT ( 'NONE',  ( 4.565063516603933280, 20.63981631578574039, 11.49999999999999645 ) ) ;
#39176 = CC_DESIGN_APPROVAL ( #21550, ( #40782 ) ) ;
#39177 = CARTESIAN_POINT ( 'NONE',  ( 2.710298230372018669, -21.94706154713207980, 11.49999999999998934 ) ) ;
#39178 = CARTESIAN_POINT ( 'NONE',  ( 3.262959013008915665, -20.29835246810489835, -1.500000000000002220 ) ) ;
#39179 = CARTESIAN_POINT ( 'NONE',  ( -60.54143455719881217, -24.52300882791528380, 0.6510814631126233820 ) ) ;
#39180 = ORIENTED_EDGE ( 'NONE', *, *, #24360, .T. ) ;
#39181 = CARTESIAN_POINT ( 'NONE',  ( -116.5895376238167103, -24.64965694238408034, 8.947790433994647685 ) ) ;
#39182 = ORIENTED_EDGE ( 'NONE', *, *, #34766, .T. ) ;
#39183 = CARTESIAN_POINT ( 'NONE',  ( -6.265203266387573855, -6.376774720514408301, 19.29154511076646017 ) ) ;
#39184 = CARTESIAN_POINT ( 'NONE',  ( -86.52287095715006160, -23.47593901973090169, -1.443836447538996648 ) ) ;
#39185 = ORIENTED_EDGE ( 'NONE', *, *, #50928, .F. ) ;
#39186 = EDGE_LOOP ( 'NONE', ( #60555, #70326, #67319, #87218 ) ) ;
#39187 = EDGE_LOOP ( 'NONE', ( #50206, #73656, #22074, #96256 ) ) ;
#39188 = CARTESIAN_POINT ( 'NONE',  ( -112.6228709571500701, -23.73907113216992215, -1.053371485793222595 ) ) ;
#39189 = CARTESIAN_POINT ( 'NONE',  ( -74.55620429048340725, -24.66019654487199020, 8.947790411086131712 ) ) ;
#39190 = CARTESIAN_POINT ( 'NONE',  ( -68.62714824416330828, -24.51419770103157347, 9.386484678747180510 ) ) ;
#39191 = CARTESIAN_POINT ( 'NONE',  ( -15.52656095410427817, -13.64048245868121434, -1.500000000000002220 ) ) ;
#39192 = CARTESIAN_POINT ( 'NONE',  ( 21.36531308999010648, 3.172564587314818052, 11.49999999999999645 ) ) ;
#39193 = VERTEX_POINT ( 'NONE', #59979 ) ;
#39194 = FACE_OUTER_BOUND ( 'NONE', #15232, .T. ) ;
#39195 = CARTESIAN_POINT ( 'NONE',  ( 2.936453026386435017, -5.876774720514406525, 18.60215244312560401 ) ) ;
#39196 = CARTESIAN_POINT ( 'NONE',  ( -9.622923231576368863, -20.19340101508991125, 11.49999999999998934 ) ) ;
#39197 = B_SPLINE_CURVE_WITH_KNOTS ( 'NONE', 3,
 ( #16927, #40272, #3233, #49902, #95055, #19921, #88451, #43280 ),
 .UNSPECIFIED., .F., .F.,
 ( 4, 2, 2, 4 ),
 ( 0.000000000000000000, 0.002001079623178224527, 0.003001619434767337658, 0.004002159246356450789 ),
 .UNSPECIFIED. ) ;
#39198 = CARTESIAN_POINT ( 'NONE',  ( -47.53067075290624643, -24.66019654487199730, 8.947790411086117501 ) ) ;
#39199 = LINE ( 'NONE', #38699, #38341 ) ;
#39200 = EDGE_LOOP ( 'NONE', ( #6174, #47158, #30346, #80760 ) ) ;
#39201 = CARTESIAN_POINT ( 'NONE',  ( -100.1809493305549807, -25.31121442495619789, 4.675423118741687922 ) ) ;
#39202 = CARTESIAN_POINT ( 'NONE',  ( -35.56110783281771859, -23.85049219812685095, 10.88485053497527488 ) ) ;
#39203 = CARTESIAN_POINT ( 'NONE',  ( -12.67655569012464944, 16.65582705476778358, -1.500000000000002220 ) ) ;
#39204 = ORIENTED_EDGE ( 'NONE', *, *, #7531, .F. ) ;
#39205 = CARTESIAN_POINT ( 'NONE',  ( -45.52287095715007581, -24.14406661686763300, 10.28769366194075019 ) ) ;
#39206 = ORIENTED_EDGE ( 'NONE', *, *, #71943, .F. ) ;
#39207 = VECTOR ( 'NONE', #5799, 1000.000000000000114 ) ;
#39208 = CARTESIAN_POINT ( 'NONE',  ( -86.62287095715004170, -29.50248528299804818, 1.056150453629040253 ) ) ;
#39209 = CARTESIAN_POINT ( 'NONE',  ( -0.1268723920767304558, 21.18662008908366445, -1.500000000000002220 ) ) ;
#39210 = EDGE_LOOP ( 'NONE', ( #42387, #91016, #68828, #5512 ) ) ;
#39211 = PLANE ( 'NONE',  #80296 ) ;
#39212 = EDGE_CURVE ( 'NONE', #70182, #75883, #90913, .T. ) ;
#39213 = CARTESIAN_POINT ( 'NONE',  ( -21.42251255223715134, 3.917230396363152067, 11.49999999999998934 ) ) ;
#39214 = CARTESIAN_POINT ( 'NONE',  ( -121.5228709571501042, -24.51387760970724727, 9.387446482453400520 ) ) ;
#39215 = EDGE_CURVE ( 'NONE', #67600, #91984, #92927, .T. ) ;
#39216 = CARTESIAN_POINT ( 'NONE',  ( -36.62287095715005592, -24.50216790748205042, 0.6166512839542488411 ) ) ;
#39217 = CARTESIAN_POINT ( 'NONE',  ( -116.6228709571501270, -24.34917612406838927, 0.1852690917426708661 ) ) ;
#39218 = CARTESIAN_POINT ( 'NONE',  ( 16.38291735060997567, -14.39268585342195905, -1.500000000000002220 ) ) ;
#39219 = CARTESIAN_POINT ( 'NONE',  ( -30.57287095715005520, -24.91181100195775500, 1.926074808287914886 ) ) ;
#39220 = ORIENTED_EDGE ( 'NONE', *, *, #21794, .F. ) ;
#39221 = CARTESIAN_POINT ( 'NONE',  ( 30.53060340732036337, -1.682774720514426114, -8.442346167188910400 ) ) ;
#39222 = LINE ( 'NONE', #15885, #26490 ) ;
#39223 = ORIENTED_EDGE ( 'NONE', *, *, #82364, .T. ) ;
#39224 = ADVANCED_FACE ( 'NONE', ( #79181 ), #18212, .T. ) ;
#39225 = EDGE_CURVE ( 'NONE', #6738, #45200, #32515, .T. ) ;
#39226 = ORIENTED_EDGE ( 'NONE', *, *, #44181, .T. ) ;
#39227 = EDGE_CURVE ( 'NONE', #94973, #68532, #93906, .T. ) ;
#39228 = ORIENTED_EDGE ( 'NONE', *, *, #77025, .T. ) ;
#39229 = VECTOR ( 'NONE', #92792, 1000.000000000000000 ) ;
#39230 = CARTESIAN_POINT ( 'NONE',  ( -27.83188564017057942, -24.78446414523650176, 2.282593631282324953 ) ) ;
#39231 = DIRECTION ( 'NONE',  ( 0.8246584009594635223, 0.5656310827093757876, 0.000000000000000000 ) ) ;
#39232 = CARTESIAN_POINT ( 'NONE',  ( 20.79131504077403747, 4.132458064796619368, -1.500000000000002220 ) ) ;
#39233 = VECTOR ( 'NONE', #11818, 1000.000000000000114 ) ;
#39234 = CARTESIAN_POINT ( 'NONE',  ( -71.62287095715005592, -24.66019654487199020, 8.947790411086131712 ) ) ;
#39235 = DIRECTION ( 'NONE',  ( 0.000000000000000000, 0.000000000000000000, -1.000000000000000000 ) ) ;
#39236 = DIRECTION ( 'NONE',  ( -1.000000000000000000, 0.000000000000000000, 0.000000000000000000 ) ) ;
#39237 = CARTESIAN_POINT ( 'NONE',  ( -128.5562042904834072, -23.47593901973091235, -1.443836447538995760 ) ) ;
#39238 = CARTESIAN_POINT ( 'NONE',  ( 17.72857150710123619, 7.855407458714720903, 11.49999999999998934 ) ) ;
#39239 = CARTESIAN_POINT ( 'NONE',  ( -39.98262533683074338, -25.20650829394578096, 6.812666491500988464 ) ) ;
#39240 = ORIENTED_EDGE ( 'NONE', *, *, #88791, .F. ) ;
#39241 = CARTESIAN_POINT ( 'NONE',  ( -18.70048401425367501, 5.426029767813830063, 11.49999999999999645 ) ) ;
#39242 = PLANE ( 'NONE',  #74675 ) ;
#39243 = CARTESIAN_POINT ( 'NONE',  ( -2.749999999999999112, 27.59999999999999432, 0.000000000000000000 ) ) ;
#39244 = ADVANCED_FACE ( 'NONE', ( #23890 ), #9172, .F. ) ;
#39245 = ORIENTED_EDGE ( 'NONE', *, *, #70090, .T. ) ;
#39246 = CARTESIAN_POINT ( 'NONE',  ( -93.62287095715002749, -24.50216790748099882, 0.6166512839513739186 ) ) ;
#39247 = CARTESIAN_POINT ( 'NONE',  ( -59.52287095715003318, -23.73934037231755667, 11.05740245334329330 ) ) ;
#39248 = CARTESIAN_POINT ( 'NONE',  ( -106.5228709571500616, -24.50216790748204332, 0.6166512839542641622 ) ) ;
#39249 = AXIS2_PLACEMENT_3D ( 'NONE', #9960, #40911, #1855 ) ;
#39250 = CARTESIAN_POINT ( 'NONE',  ( -93.58623170259684798, -24.51419770103157703, 9.386484678747164523 ) ) ;
#39252 = EDGE_CURVE ( 'NONE', #75907, #91581, #8719, .T. ) ;
#39251 = CARTESIAN_POINT ( 'NONE',  ( 19.42422255247381457, -2.945173967302487039, -1.500000000000002220 ) ) ;
#39253 = CARTESIAN_POINT ( 'NONE',  ( -128.5228709571500758, -29.50248528299804818, 1.056150453629047137 ) ) ;
#39255 = ORIENTED_EDGE ( 'NONE', *, *, #11318, .T. ) ;
#39254 = LOCAL_TIME ( 0, 54, 15.00000000000000000, #57010 ) ;
#39256 = CARTESIAN_POINT ( 'NONE',  ( -8.750087785235610482, 19.73178376063210138, -1.500000000000002220 ) ) ;
#39257 = CARTESIAN_POINT ( 'NONE',  ( 8.160000000000000142, -5.396855673853237919E-16, 5.288828319098142217 ) ) ;
#39258 = DIRECTION ( 'NONE',  ( 0.000000000000000000, 0.000000000000000000, 1.000000000000000000 ) ) ;
#39259 = CARTESIAN_POINT ( 'NONE',  ( -7.156825135384894843, 21.90021990432103038, -1.500000000000002220 ) ) ;
#39260 = APPROVAL_DATE_TIME ( #29654, #100233 ) ;
#39261 = CARTESIAN_POINT ( 'NONE',  ( 0.000000000000000000, 5.356774720514425603, 6.000000000000000888 ) ) ;
#39262 = PLANE ( 'NONE',  #89582 ) ;
#39263 = DIRECTION ( 'NONE',  ( -1.000000000000000000, -3.773278334444166432E-23, -8.201307841325785021E-29 ) ) ;
#39264 = CARTESIAN_POINT ( 'NONE',  ( 6.660000000000001030, 0.000000000000000000, 0.000000000000000000 ) ) ;
#39265 = CARTESIAN_POINT ( 'NONE',  ( 5.641025641025643189, -6.376774720514420736, 20.78665865384615330 ) ) ;
#39266 = CARTESIAN_POINT ( 'NONE',  ( -129.5222683595572732, -23.48783264082477729, -1.443836473390078590 ) ) ;
#39267 = AXIS2_PLACEMENT_3D ( 'NONE', #80786, #19374, #58952 ) ;
#39268 = CARTESIAN_POINT ( 'NONE',  ( -99.15308351095438866, -25.31565957498872521, 4.278189846497874704 ) ) ;
#39269 = CARTESIAN_POINT ( 'NONE',  ( -5.841000908416043913, -19.03464889989004050, 11.49999999999998934 ) ) ;
#39270 = CARTESIAN_POINT ( 'NONE',  ( -32.62287095715004881, -23.47593901973091235, -1.443836447539013301 ) ) ;
#39271 = CARTESIAN_POINT ( 'NONE',  ( 7.713363164125232707, -18.29545692620113684, -1.500000000000002220 ) ) ;
#39272 = DIRECTION ( 'NONE',  ( -0.000000000000000000, 1.000000000000000000, -0.000000000000000000 ) ) ;
#39273 = EDGE_CURVE ( 'NONE', #48122, #29681, #55365, .T. ) ;
#39274 = DIRECTION ( 'NONE',  ( 0.000000000000000000, 0.000000000000000000, -1.000000000000000000 ) ) ;
#39275 = DIRECTION ( 'NONE',  ( -0.2488812114211666759, 0.000000000000000000, -0.9685340172660599212 ) ) ;
#39276 = CARTESIAN_POINT ( 'NONE',  ( -20.61657899823519813, -2.091364977790679980, 11.49999999999999645 ) ) ;
#39277 = CARTESIAN_POINT ( 'NONE',  ( -7.635352852713973348, -5.876774720514415407, 20.14409848895066091 ) ) ;
#39278 = B_SPLINE_CURVE_WITH_KNOTS ( 'NONE', 3,
 ( #51297, #6614, #97948, #13216 ),
 .UNSPECIFIED., .F., .F.,
 ( 4, 4 ),
 ( 0.000000000000000000, 0.0001000000000000028508 ),
 .UNSPECIFIED. ) ;
#39279 = EDGE_CURVE ( 'NONE', #88430, #40707, #78663, .T. ) ;
#39280 = CARTESIAN_POINT ( 'NONE',  ( -106.5486723502721844, -24.65952944569304961, 1.056160979905703456 ) ) ;
#39281 = CARTESIAN_POINT ( 'NONE',  ( -22.52399778787742335, 3.408274809117095572, 11.49999999999999645 ) ) ;
#39282 = CIRCLE ( 'NONE', #62033, 91.74549126261076992 ) ;
#39283 = VERTEX_POINT ( 'NONE', #2083 ) ;
#39284 = B_SPLINE_SURFACE_WITH_KNOTS ( 'NONE', 3, 1, ( 
 ( #29662, #99652 ),
 ( #82943, #60637 ),
 ( #91558, #14925 ),
 ( #92058, #53019 ),
 ( #22529, #43901 ),
 ( #83949, #52513 ),
 ( #91062, #30157 ),
 ( #61131, #75830 ),
 ( #36785, #76815 ),
 ( #82452, #13433 ),
 ( #44407, #53522 ),
 ( #21536, #7314 ),
 ( #69226, #67248 ),
 ( #98167, #90565 ),
 ( #75332, #7821 ),
 ( #40774, #62625 ),
 ( #86945, #30664 ),
 ( #93544, #211 ),
 ( #55012, #9823 ) ),
 .UNSPECIFIED., .F., .F., .F.,
 ( 4, 1, 1, 1, 1, 1, 1, 1, 1, 1, 1, 1, 1, 1, 1, 1, 4 ),
 ( 2, 2 ),
 ( 0.000000000000000000, 0.06443867159524530042, 0.1265469112716785804, 0.1868871534365660614, 0.2458775355894579628, 0.3040408846912645568, 0.3621912180726578612, 0.4209759327916451910, 0.4806602832796664782, 0.5406002749537588414, 0.6006890983494537206, 0.6619357897571975791, 0.7244425059139834033, 0.7890383938817431275, 0.8563137570509946617, 0.9263520282058630428, 1.000000000000000000 ),
 ( 0.000000000000000000, 1.000000000000000000 ),
 .UNSPECIFIED. ) ;
#39285 = CARTESIAN_POINT ( 'NONE',  ( -69.53739244225492655, -24.65952944569304606, 1.056160979905704567 ) ) ;
#39286 = B_SPLINE_CURVE_WITH_KNOTS ( 'NONE', 3,
 ( #11895, #4293, #89029, #42864 ),
 .UNSPECIFIED., .F., .F.,
 ( 4, 4 ),
 ( 3.876650091915111752E-09, 0.002303383447661763554 ),
 .UNSPECIFIED. ) ;
#39287 = DIRECTION ( 'NONE',  ( -0.7512896232465891000, -0.000000000000000000, -0.6599726524652351767 ) ) ;
#39288 = ORIENTED_EDGE ( 'NONE', *, *, #27731, .T. ) ;
#39289 = CARTESIAN_POINT ( 'NONE',  ( 8.473373031455752269, -18.34320851062214430, 11.49999999999998934 ) ) ;
#39290 = FACE_OUTER_BOUND ( 'NONE', #67810, .T. ) ;
#39291 = CARTESIAN_POINT ( 'NONE',  ( -40.73433408427551683, -25.30552906146762027, 5.044818317511085226 ) ) ;
#39292 = ORIENTED_EDGE ( 'NONE', *, *, #78461, .T. ) ;
#39293 = ORIENTED_EDGE ( 'NONE', *, *, #20480, .T. ) ;
#39294 = CARTESIAN_POINT ( 'NONE',  ( -127.5228709571500900, -24.34917612406837861, 0.1852690917426607076 ) ) ;
#39295 = CARTESIAN_POINT ( 'NONE',  ( 15.42672287639063100, 16.92133821996916865, 11.49999999999998934 ) ) ;
#39296 = CARTESIAN_POINT ( 'NONE',  ( -41.80014015042835496, -25.25166947788726191, 3.754039313533760858 ) ) ;
#39297 = CARTESIAN_POINT ( 'NONE',  ( -15.70146493180990888, -14.86199287721409590, -1.500000000000002220 ) ) ;
#39298 = CARTESIAN_POINT ( 'NONE',  ( 14.61581676223891613, -3.316774720514426900, -27.35847991879931485 ) ) ;
#39299 = VECTOR ( 'NONE', #28782, 1000.000000000000114 ) ;
#39300 = CARTESIAN_POINT ( 'NONE',  ( 2.299058169534009100, 20.76012671103276475, 11.49999999999999645 ) ) ;
#39301 = ORIENTED_EDGE ( 'NONE', *, *, #15326, .T. ) ;
#39302 = CARTESIAN_POINT ( 'NONE',  ( -61.25483235428281148, -25.21329443217976873, 6.713654904961149583 ) ) ;
#39303 = CARTESIAN_POINT ( 'NONE',  ( -68.93918693012690824, -25.24754535617828921, 6.184868461386431093 ) ) ;
#39304 = CARTESIAN_POINT ( 'NONE',  ( -20.87105610827876134, -7.033761084331515256, -1.500000000000002220 ) ) ;
#39305 = DIRECTION ( 'NONE',  ( 1.000000000000000000, 4.986391167143583514E-16, 0.000000000000000000 ) ) ;
#39306 = LINE ( 'NONE', #70262, #57776 ) ;
#39307 = ORIENTED_EDGE ( 'NONE', *, *, #77120, .F. ) ;
#39308 = CARTESIAN_POINT ( 'NONE',  ( 9.383883476483161346, 17.86611652351680846, 2.100000000000000089 ) ) ;
#39309 = LINE ( 'NONE', #86981, #98021 ) ;
#39310 = ORIENTED_EDGE ( 'NONE', *, *, #95831, .T. ) ;
#39311 = FACE_OUTER_BOUND ( 'NONE', #24098, .T. ) ;
#39312 = ORIENTED_EDGE ( 'NONE', *, *, #37545, .T. ) ;
#39313 = EDGE_LOOP ( 'NONE', ( #38608, #43982, #45565, #51130, #9341, #86769, #74993, #56497 ) ) ;
#39314 = CARTESIAN_POINT ( 'NONE',  ( -106.6228709571500275, -24.51283580621364067, 0.6167428607019890263 ) ) ;
#39315 = CARTESIAN_POINT ( 'NONE',  ( -27.83739072329610664, -0.3587747205143967943, -8.084349702057700426 ) ) ;
#39316 = CARTESIAN_POINT ( 'NONE',  ( -4.289200894924355190, -5.876774720514413630, 19.85590024959437017 ) ) ;
#39317 = CARTESIAN_POINT ( 'NONE',  ( -20.46784169311667867, 0.4426517378232717737, -1.500000000000002220 ) ) ;
#39318 = ORIENTED_EDGE ( 'NONE', *, *, #73619, .F. ) ;
#39319 = CARTESIAN_POINT ( 'NONE',  ( -71.62287095715005592, -24.35013146730204170, 9.818937971375111928 ) ) ;
#39320 = CARTESIAN_POINT ( 'NONE',  ( -44.60008626239309848, -23.96119346886879597, -0.6495511937832129101 ) ) ;
#39321 = CARTESIAN_POINT ( 'NONE',  ( -77.52287095715006160, -24.64898659630367916, 1.056161002820826145 ) ) ;
#39322 = CARTESIAN_POINT ( 'NONE',  ( -8.840690135214121170, 20.45858245768130956, -1.500000000000002220 ) ) ;
#39324 = CARTESIAN_POINT ( 'NONE',  ( -55.52287095715006160, -24.83620972994591014, 8.398175272781369216 ) ) ;
#39323 = AXIS2_PLACEMENT_3D ( 'NONE', #52255, #6570, #45638 ) ;
#39325 = CARTESIAN_POINT ( 'NONE',  ( -27.70544111104076990, -24.64017222881049207, 8.251826729410561612 ) ) ;
#39326 = ORIENTED_EDGE ( 'NONE', *, *, #62657, .T. ) ;
#39327 = CARTESIAN_POINT ( 'NONE',  ( 26.73860345374794534, 1.477225279485574028, 3.440769881205036427E-15 ) ) ;
#39328 = CARTESIAN_POINT ( 'NONE',  ( -29.77636857527935277, -24.63645529384542954, 5.788904288867858128 ) ) ;
#39329 = APPROVAL_PERSON_ORGANIZATION ( #84811, #47590, #77685 ) ;
#39330 = CARTESIAN_POINT ( 'NONE',  ( -20.33245250387252767, 4.503473919074798104, -1.500000000000002220 ) ) ;
#39331 = VERTEX_POINT ( 'NONE', #71085 ) ;
#39333 = ORIENTED_EDGE ( 'NONE', *, *, #84712, .F. ) ;
#39332 = DIRECTION ( 'NONE',  ( -1.000000000000000000, -3.773278334444167608E-23, -8.201307833595939069E-29 ) ) ;
#39335 = ORIENTED_EDGE ( 'NONE', *, *, #18044, .T. ) ;
#39334 = B_SPLINE_CURVE_WITH_KNOTS ( 'NONE', 3,
 ( #7127, #38077, #69032, #99960 ),
 .UNSPECIFIED., .F., .F.,
 ( 4, 4 ),
 ( 0.000000000000000000, 9.999999999998897304E-05 ),
 .UNSPECIFIED. ) ;
#39336 = VECTOR ( 'NONE', #10571, 1000.000000000000114 ) ;
#39337 = CARTESIAN_POINT ( 'NONE',  ( -58.52287095715006870, -23.95044443724993144, 10.65354141964648882 ) ) ;
#39338 = CARTESIAN_POINT ( 'NONE',  ( 18.89479412359299815, 9.153864009170110450, -1.500000000000002220 ) ) ;
#39339 = ORIENTED_EDGE ( 'NONE', *, *, #8881, .T. ) ;
#39340 = LINE ( 'NONE', #56083, #72196 ) ;
#39342 = EDGE_CURVE ( 'NONE', #59659, #35661, #24892, .T. ) ;
#39341 = CARTESIAN_POINT ( 'NONE',  ( -55.62287095715004881, -24.82576562982391621, 8.398263435472967942 ) ) ;
#39343 = CARTESIAN_POINT ( 'NONE',  ( 11.25623914429021788, -5.356774720514424715, -27.04805245727492036 ) ) ;
#39344 = VECTOR ( 'NONE', #72080, 1000.000000000000114 ) ;
#39345 = DIRECTION ( 'NONE',  ( -3.773278334453079618E-23, 0.9999999999976377785, 2.173523156925979975E-06 ) ) ;
#39346 = B_SPLINE_CURVE_WITH_KNOTS ( 'NONE', 3,
 ( #51671, #97828, #36433, #21197, #67397, #59790, #28825, #90724, #52163, #99322, #83093, #44552, #75477, #5982, #36931 ),
 .UNSPECIFIED., .F., .F.,
 ( 4, 1, 1, 1, 1, 1, 1, 1, 1, 1, 1, 1, 4 ),
 ( 0.000000000000000000, 0.08433472199262730118, 0.1670523184160740138, 0.2495660772409658001, 0.3327404818018465660, 0.4159148863627275539, 0.4978280095399964522, 0.5803725886080518537, 0.6646001210565030126, 0.7494666931126164888, 0.8325102339401410090, 0.9156392816681726554, 1.000000000000000000 ),
 .UNSPECIFIED. ) ;
#39347 = CARTESIAN_POINT ( 'NONE',  ( -59.50360827014927168, -24.15543982623906416, -0.2315651400026668416 ) ) ;
#39348 = DIRECTION ( 'NONE',  ( -0.9903949459893287566, -0.09776975748868939331, -0.09776975748869010108 ) ) ;
#39350 = ORIENTED_EDGE ( 'NONE', *, *, #56085, .T. ) ;
#39349 = CARTESIAN_POINT ( 'NONE',  ( 16.02632597834478645, 15.35701383120132313, 11.49999999999999645 ) ) ;
#39351 = CARTESIAN_POINT ( 'NONE',  ( -8.978253834636468866, -5.876774720514426953, 21.48128695274316158 ) ) ;
#39352 = DIRECTION ( 'NONE',  ( 0.000000000000000000, -1.000000000000000000, 0.000000000000000000 ) ) ;
#39353 = ORIENTED_EDGE ( 'NONE', *, *, #58876, .F. ) ;
#39354 = EDGE_CURVE ( 'NONE', #16401, #43562, #18415, .T. ) ;
#39355 = CARTESIAN_POINT ( 'NONE',  ( -22.46375958613465684, 3.124547546656453179, -1.500000000000002220 ) ) ;
#39356 = ADVANCED_FACE ( 'NONE', ( #50747 ), #17794, .T. ) ;
#39358 = ORIENTED_EDGE ( 'NONE', *, *, #34195, .T. ) ;
#39357 = CARTESIAN_POINT ( 'NONE',  ( -28.37391457004085638, -24.89382844618185331, 7.412098205223180081 ) ) ;
#39359 = ADVANCED_FACE ( 'NONE', ( #65495 ), #73582, .T. ) ;
#39360 = ORIENTED_EDGE ( 'NONE', *, *, #74673, .T. ) ;
#39361 = ADVANCED_FACE ( 'NONE', ( #26406 ), #88309, .F. ) ;
#39362 = FACE_OUTER_BOUND ( 'NONE', #6065, .T. ) ;
#39363 = AXIS2_PLACEMENT_3D ( 'NONE', #80444, #57622, #27162 ) ;
#39364 = B_SPLINE_CURVE_WITH_KNOTS ( 'NONE', 3,
 ( #78107, #79623, #55810, #49201 ),
 .UNSPECIFIED., .F., .F.,
 ( 4, 4 ),
 ( 2.677034095660378764E-09, 0.001652431040122505791 ),
 .UNSPECIFIED. ) ;
#39365 = CARTESIAN_POINT ( 'NONE',  ( 7.141438900065890216, -18.84860497471923679, 11.49999999999998934 ) ) ;
#39366 = DIRECTION ( 'NONE',  ( 0.7512896232465892110, 0.000000000000000000, 0.6599726524652351767 ) ) ;
#39367 = ORIENTED_EDGE ( 'NONE', *, *, #19528, .T. ) ;
#39368 = CARTESIAN_POINT ( 'NONE',  ( -80.96226385320385077, -25.14083923594767001, 2.947789366383926968 ) ) ;
#39369 = CARTESIAN_POINT ( 'NONE',  ( -14.53400517605410158, 16.95891092046126403, -1.500000000000002220 ) ) ;
#39370 = ORIENTED_EDGE ( 'NONE', *, *, #67200, .T. ) ;
#39371 = ORIENTED_EDGE ( 'NONE', *, *, #89994, .F. ) ;
#39372 = CARTESIAN_POINT ( 'NONE',  ( -29.62287095715004881, -29.50250786944496539, 11.44777975102276812 ) ) ;
#39374 = CARTESIAN_POINT ( 'NONE',  ( -4.401146115524053215, -5.876774720514411854, 19.34190049657481936 ) ) ;
#39373 = AXIS2_PLACEMENT_3D ( 'NONE', #82764, #13246, #36591 ) ;
#39375 = LINE ( 'NONE', #61730, #2049 ) ;
#39376 = CARTESIAN_POINT ( 'NONE',  ( -57.52287095715005449, -24.64965694238407323, 8.947790433994201820 ) ) ;
#39377 = CARTESIAN_POINT ( 'NONE',  ( -63.93900422158343844, -24.04615231314291535, -0.4716817114508916609 ) ) ;
#39378 = CARTESIAN_POINT ( 'NONE',  ( -0.4769873229303308038, -19.55164744950295841, 11.49999999999998934 ) ) ;
#39379 = VECTOR ( 'NONE', #55402, 1000.000000000000000 ) ;
#39380 = CARTESIAN_POINT ( 'NONE',  ( -5.457842845122470976, -5.876774720514410966, 19.25892998154168367 ) ) ;
#39381 = CARTESIAN_POINT ( 'NONE',  ( 15.57385778016992894, -14.83193121981731544, 11.49999999999998934 ) ) ;
#39382 = CARTESIAN_POINT ( 'NONE',  ( -2.794644232660540961, -5.876774720514413630, 20.26757654895259009 ) ) ;
#39383 = DIRECTION ( 'NONE',  ( -3.773278334453079618E-23, 0.9999999999976377785, 2.173523156925979975E-06 ) ) ;
#39384 = FACE_BOUND ( 'NONE', #73276, .T. ) ;
#39385 = DIRECTION ( 'NONE',  ( -0.000000000000000000, -0.000000000000000000, -1.000000000000000000 ) ) ;
#39386 = CARTESIAN_POINT ( 'NONE',  ( 19.70479270790718829, 11.56945388388114360, -1.500000000000002220 ) ) ;
#39387 = B_SPLINE_CURVE_WITH_KNOTS ( 'NONE', 3,
 ( #35604, #66575, #90873, #97488 ),
 .UNSPECIFIED., .F., .F.,
 ( 4, 4 ),
 ( 0.9104360445717412098, 0.9194424758438565215 ),
 .UNSPECIFIED. ) ;
#39388 = PERSON_AND_ORGANIZATION ( #70597, #27821 ) ;
#39389 = DIRECTION ( 'NONE',  ( 0.000000000000000000, -2.173523156925980399E-06, 0.9999999999976378895 ) ) ;
#39390 = CARTESIAN_POINT ( 'NONE',  ( -53.60569991856895911, -23.73766607897669090, -1.055555164236459564 ) ) ;
#39391 = CARTESIAN_POINT ( 'NONE',  ( -18.81269933604069067, 6.858547123926768130, 11.49999999999999645 ) ) ;
#39392 = CARTESIAN_POINT ( 'NONE',  ( -100.2228709571500787, -23.47593901973090169, -1.443836447538996870 ) ) ;
#39393 = FACE_OUTER_BOUND ( 'NONE', #17697, .T. ) ;
#39394 = DIRECTION ( 'NONE',  ( 1.000000000000000000, -0.000000000000000000, -0.000000000000000000 ) ) ;
#39395 = DIRECTION ( 'NONE',  ( -3.773278334453079618E-23, 0.9999999999976377785, 2.173523156925979975E-06 ) ) ;
#39396 = ORIENTED_EDGE ( 'NONE', *, *, #68696, .F. ) ;
#39397 = CARTESIAN_POINT ( 'NONE',  ( 10.34999999999998010, 27.69999999999999929, 2.100000000000000089 ) ) ;
#39398 = CARTESIAN_POINT ( 'NONE',  ( -13.65724274058436194, -16.95215541261048742, 11.49999999999998934 ) ) ;
#39399 = CARTESIAN_POINT ( 'NONE',  ( 7.160000000000000142, -6.754662360505033547, 7.925641719537454222 ) ) ;
#39400 = CARTESIAN_POINT ( 'NONE',  ( -16.08770303010339831, 11.32657509950784736, -1.500000000000002220 ) ) ;
#39401 = CARTESIAN_POINT ( 'NONE',  ( 10.86264265030973952, 5.965225279485574461, -28.64597719988137570 ) ) ;
#39402 = B_SPLINE_CURVE_WITH_KNOTS ( 'NONE', 3,
 ( #8939, #31779, #326, #62750, #94673, #32276 ),
 .UNSPECIFIED., .F., .F.,
 ( 4, 2, 4 ),
 ( 0.000000000000000000, 0.001380764517854765399, 0.002761529035709530799 ),
 .UNSPECIFIED. ) ;
#39403 = AXIS2_PLACEMENT_3D ( 'NONE', #75697, #69092, #22403 ) ;
#39404 = CARTESIAN_POINT ( 'NONE',  ( -41.46432051929361506, -25.27404221065474843, 4.124998039036684716 ) ) ;
#39405 = DATE_AND_TIME ( #39902, #53976 ) ;
#39406 = ORGANIZATION ( 'NAUO-ORG10', 'UNSPECIFIED', 'UNSPECIFIED' ) ;
#39407 = CARTESIAN_POINT ( 'NONE',  ( -20.77875734969026311, 6.143225279485574397, 27.35402280011862430 ) ) ;
#39408 = CARTESIAN_POINT ( 'NONE',  ( -73.62287095715007013, -24.66019654487199020, 8.947790411086131712 ) ) ;
#39409 = CARTESIAN_POINT ( 'NONE',  ( 20.52540449432101610, 0.9483640940595650104, 11.49999999999999645 ) ) ;
#39410 = CARTESIAN_POINT ( 'NONE',  ( 3.787259615384621192, -5.876774720514425177, 21.48076923076922640 ) ) ;
#39411 = EDGE_CURVE ( 'NONE', #23469, #92122, #64500, .T. ) ;
#39412 = LINE ( 'NONE', #24178, #54589 ) ;
#39413 = VECTOR ( 'NONE', #23532, 1000.000000000000000 ) ;
#39414 = CARTESIAN_POINT ( 'NONE',  ( 18.79633983808273712, -12.56333175589740847, 11.49999999999999645 ) ) ;
#39415 = EDGE_LOOP ( 'NONE', ( #65100, #11747, #36091, #2186 ) ) ;
#39416 = EDGE_CURVE ( 'NONE', #73037, #95392, #21993, .T. ) ;
#39417 = CARTESIAN_POINT ( 'NONE',  ( -99.53249707683190195, -25.31296311462813975, 4.095394517951907787 ) ) ;
#39418 = CARTESIAN_POINT ( 'NONE',  ( -37.52287095715006870, -24.64898659630367206, 1.056161002820819261 ) ) ;
#39419 = CARTESIAN_POINT ( 'NONE',  ( -125.5890726425938055, -24.83644354573579349, 8.397322867130096569 ) ) ;
#39420 = DIRECTION ( 'NONE',  ( -0.8264557562326038109, -6.454799914155187856E-16, -0.5630016722799275897 ) ) ;
#39421 = VECTOR ( 'NONE', #41365, 1000.000000000000000 ) ;
#39422 = CARTESIAN_POINT ( 'NONE',  ( -33.62287095715007013, -24.33832256527048088, 0.1851278514138572917 ) ) ;
#39423 = CARTESIAN_POINT ( 'NONE',  ( -75.55620429048340725, -23.47593901973091235, -1.443836447539004642 ) ) ;
#39424 = VERTEX_POINT ( 'NONE', #11180 ) ;
#39425 = CARTESIAN_POINT ( 'NONE',  ( 1.912052097559287844, -22.98750448113701239, 11.49999999999999645 ) ) ;
#39426 = CARTESIAN_POINT ( 'NONE',  ( 21.14626179850551324, 8.528272852130310611, -1.500000000000002220 ) ) ;
#39427 = CARTESIAN_POINT ( 'NONE',  ( 3.825970207471427020, -5.876774720514403860, 18.52126221587801780 ) ) ;
#39428 = B_SPLINE_SURFACE_WITH_KNOTS ( 'NONE', 3, 1, ( 
 ( #29739, #84019 ),
 ( #6899, #60706 ),
 ( #91627, #14506 ),
 ( #76396, #88032 ),
 ( #95639, #18010 ),
 ( #17004, #48973 ),
 ( #78395, #79904 ),
 ( #26124, #10904 ),
 ( #2301, #96144 ),
 ( #55590, #41867 ),
 ( #34245, #9894 ),
 ( #24610, #8898 ),
 ( #65220, #32731 ),
 ( #71307, #40353 ),
 ( #39844, #25111 ),
 ( #26631, #88528 ),
 ( #1792, #72811 ),
 ( #17510, #57095 ),
 ( #94631, #57591 ) ),
 .UNSPECIFIED., .F., .F., .F.,
 ( 4, 1, 1, 1, 1, 1, 1, 1, 1, 1, 1, 1, 1, 1, 1, 1, 4 ),
 ( 2, 2 ),
 ( 0.000000000000000000, 0.06554117033740432252, 0.1289631677825942568, 0.1903771361885626123, 0.2500923616690557960, 0.3085484324592007166, 0.3663979630552985367, 0.4245421892666791930, 0.4831699964229071442, 0.5422433998311213532, 0.6017393520173313082, 0.6625060022496070955, 0.7248555134488467999, 0.7891278292811820805, 0.8563463998785099118, 0.9262952349869061353, 1.000000000000000000 ),
 ( 0.000000000000000000, 1.000000000000000000 ),
 .UNSPECIFIED. ) ;
#39429 = CARTESIAN_POINT ( 'NONE',  ( -72.62287095715005592, -24.66019654487199020, 8.947790411086131712 ) ) ;
#39430 = CARTESIAN_POINT ( 'NONE',  ( -35.52287095715006870, -23.47593901973090169, -1.443836447538997092 ) ) ;
#39431 = CARTESIAN_POINT ( 'NONE',  ( 19.55810785529653373, 10.91776788121007868, 11.49999999999999645 ) ) ;
#39432 = VERTEX_POINT ( 'NONE', #95415 ) ;
#39433 = CARTESIAN_POINT ( 'NONE',  ( -125.6228709571500275, -23.48783264082479505, -1.443836473390057273 ) ) ;
#39434 = DIRECTION ( 'NONE',  ( 0.000000000000000000, -0.9999999999976377785, -2.173523156925979128E-06 ) ) ;
#39435 = CARTESIAN_POINT ( 'NONE',  ( 20.73430856240977249, 7.200853762728330665, 11.49999999999998934 ) ) ;
#39436 = CC_DESIGN_DATE_AND_TIME_ASSIGNMENT ( #19061, #34799, ( #37589 ) ) ;
#39437 = CARTESIAN_POINT ( 'NONE',  ( -5.837039262820512775, -5.876774720514413630, 19.76512419871795245 ) ) ;
#39438 = CARTESIAN_POINT ( 'NONE',  ( -34.52670523829452520, -24.66019654487199730, 8.947790411086117501 ) ) ;
#39439 = FACE_OUTER_BOUND ( 'NONE', #22820, .T. ) ;
#39440 = ORIENTED_EDGE ( 'NONE', *, *, #33550, .T. ) ;
#39441 = CARTESIAN_POINT ( 'NONE',  ( -98.62287095715005592, -29.50247984919015209, -1.443849546365050029 ) ) ;
#39442 = CARTESIAN_POINT ( 'NONE',  ( 30.53060340732036337, -5.297812262124697469, 1.539714685317310483 ) ) ;
#39443 = ORIENTED_EDGE ( 'NONE', *, *, #78866, .T. ) ;
#39444 = CARTESIAN_POINT ( 'NONE',  ( 16.11427877760282001, 12.65940972936023812, -1.500000000000002220 ) ) ;
#39445 = APPLICATION_CONTEXT ( 'configuration controlled 3d designs of mechanical parts and assemblies' ) ;
#39446 = ORIENTED_EDGE ( 'NONE', *, *, #50517, .T. ) ;
#39447 = ORIENTED_EDGE ( 'NONE', *, *, #60215, .F. ) ;
#39448 = ORIENTED_EDGE ( 'NONE', *, *, #31913, .F. ) ;
#39449 = VERTEX_POINT ( 'NONE', #58366 ) ;
#39450 = CARTESIAN_POINT ( 'NONE',  ( 18.43541038833219758, -13.85303862407246811, -1.500000000000002220 ) ) ;
#39451 = CARTESIAN_POINT ( 'NONE',  ( -41.47855695116675889, -25.26871255744267231, 3.880430150159563496 ) ) ;
#39452 = CARTESIAN_POINT ( 'NONE',  ( -2.356373108420451334, 20.14613781377289214, -1.500000000000002220 ) ) ;
#39453 = CIRCLE ( 'NONE', #91305, 2.499999999999998668 ) ;
#39454 = ORIENTED_EDGE ( 'NONE', *, *, #92415, .T. ) ;
#39455 = CARTESIAN_POINT ( 'NONE',  ( -128.6228709571500417, -29.50250243563736774, 8.947779886222132717 ) ) ;
#39456 = CARTESIAN_POINT ( 'NONE',  ( -92.62572919848177833, -24.51314013834316796, 0.6176544820404266112 ) ) ;
#39457 = LINE ( 'NONE', #9503, #23742 ) ;
#39458 = CARTESIAN_POINT ( 'NONE',  ( 4.127614219445591814, -6.376774720514408301, 18.60403502951120558 ) ) ;
#39460 = ORIENTED_EDGE ( 'NONE', *, *, #58743, .T. ) ;
#39459 = CARTESIAN_POINT ( 'NONE',  ( -16.43003769262999469, -13.82051474754189258, 11.49999999999999645 ) ) ;
#39461 = CARTESIAN_POINT ( 'NONE',  ( -75.62366544631902343, -25.00158670708910691, 2.256160236439223699 ) ) ;
#39463 = VECTOR ( 'NONE', #13813, 1000.000000000000000 ) ;
#39462 = CARTESIAN_POINT ( 'NONE',  ( -61.53885010291545399, -24.51419770103157347, 9.386484678747178734 ) ) ;
#39464 = ORIENTED_EDGE ( 'NONE', *, *, #29862, .T. ) ;
#39465 = CARTESIAN_POINT ( 'NONE',  ( 1.902724757927627408, 20.64897553884969028, 11.49999999999998934 ) ) ;
#39466 = ORIENTED_EDGE ( 'NONE', *, *, #83004, .T. ) ;
#39468 = EDGE_LOOP ( 'NONE', ( #81509, #50680, #48785, #31444, #43036, #52216, #87268, #24215, #17376, #58424, #64686, #63798, #12797, #4048, #43232 ) ) ;
#39467 = LINE ( 'NONE', #70419, #63714 ) ;
#39469 = CARTESIAN_POINT ( 'NONE',  ( -111.5524794374848625, -24.35071581493544457, 9.817618358456018157 ) ) ;
#39470 = DIRECTION ( 'NONE',  ( 0.000000000000000000, -1.000000000000000000, 0.000000000000000000 ) ) ;
#39471 = ORIENTED_EDGE ( 'NONE', *, *, #1901, .F. ) ;
#39472 = VERTEX_POINT ( 'NONE', #87807 ) ;
#39473 = CARTESIAN_POINT ( 'NONE',  ( -40.52287095715005449, -25.00158670708908915, 2.256160236439166411 ) ) ;
#39474 = CARTESIAN_POINT ( 'NONE',  ( -42.52914555497864058, -24.66019654487198665, 8.947790411086131712 ) ) ;
#39475 = DIRECTION ( 'NONE',  ( 0.000000000000000000, 1.000000000000000000, -0.000000000000000000 ) ) ;
#39476 = CARTESIAN_POINT ( 'NONE',  ( 19.92286461850947887, -9.344431347164146473, 11.49999999999999645 ) ) ;
#39477 = AXIS2_PLACEMENT_3D ( 'NONE', #98202, #59166, #43936 ) ;
#39478 = LINE ( 'NONE', #24740, #17195 ) ;
#39479 = CARTESIAN_POINT ( 'NONE',  ( -10.21242994381667657, -20.12718729479640700, 11.49999999999998934 ) ) ;
#39480 = CARTESIAN_POINT ( 'NONE',  ( -10.24336464640716216, -18.35016636821181280, -1.500000000000002220 ) ) ;
#39481 = VECTOR ( 'NONE', #67380, 1000.000000000000000 ) ;
#39482 = CARTESIAN_POINT ( 'NONE',  ( 6.658651924251966392, -6.376774720514415407, 20.11748569626183425 ) ) ;
#39484 = ORIENTED_EDGE ( 'NONE', *, *, #19991, .T. ) ;
#39483 = CARTESIAN_POINT ( 'NONE',  ( -99.29687923781919778, -25.26138073939643292, 6.149712181314777482 ) ) ;
#39485 = ADVANCED_FACE ( 'NONE', ( #18293 ), #48758, .T. ) ;
#39486 = VERTEX_POINT ( 'NONE', #3083 ) ;
#39487 = ADVANCED_FACE ( 'NONE', ( #50250 ), #80192, .F. ) ;
#39488 = CYLINDRICAL_SURFACE ( 'NONE', #83845, 1.325999999999990298 ) ;
#39489 = VECTOR ( 'NONE', #7063, 1000.000000000000000 ) ;
#39490 = DIRECTION ( 'NONE',  ( -0.000000000000000000, 1.000000000000000000, -0.000000000000000000 ) ) ;
#39491 = EDGE_LOOP ( 'NONE', ( #62425, #55688, #67121, #86094 ) ) ;
#39492 = CARTESIAN_POINT ( 'NONE',  ( 20.45381123341165619, -5.387677532796200097, -1.500000000000002220 ) ) ;
#39493 = CARTESIAN_POINT ( 'NONE',  ( -2.899999999999996358, 33.29999999999999716, 2.100000000000000089 ) ) ;
#39494 = CARTESIAN_POINT ( 'NONE',  ( -50.40895856474225667, -25.26041117107507006, 7.563173721887078038 ) ) ;
#39495 = FACE_OUTER_BOUND ( 'NONE', #83152, .T. ) ;
#39496 = CARTESIAN_POINT ( 'NONE',  ( -29.49875734969025842, 0.3587747205144265483, 17.86602280011862476 ) ) ;
#39497 = CARTESIAN_POINT ( 'NONE',  ( -122.5228709571500616, -29.50250243563736774, 8.947779886222134493 ) ) ;
#39498 = CARTESIAN_POINT ( 'NONE',  ( 10.50125231818214289, 19.49540335892314502, -1.500000000000002220 ) ) ;
#39499 = AXIS2_PLACEMENT_3D ( 'NONE', #15896, #46859, #93515 ) ;
#39500 = CARTESIAN_POINT ( 'NONE',  ( -81.50937295599044319, -24.15620529776628089, 10.23563542870661180 ) ) ;
#39501 = EDGE_CURVE ( 'NONE', #68398, #34688, #42519, .T. ) ;
#39502 = ORIENTED_EDGE ( 'NONE', *, *, #92652, .F. ) ;
#39503 = CARTESIAN_POINT ( 'NONE',  ( -82.62287095715004170, -23.47596703998600631, 11.44779298504227860 ) ) ;
#39504 = CARTESIAN_POINT ( 'NONE',  ( -37.55289829746592289, -23.96119346886880663, -0.6495511937831990323 ) ) ;
#39505 = CARTESIAN_POINT ( 'NONE',  ( 3.675000000000002487, 14.49999999999999822, 12.73734666247253244 ) ) ;
#39506 = CARTESIAN_POINT ( 'NONE',  ( -75.92287095715006728, -23.47593901973090169, -1.443836447538997536 ) ) ;
#39507 = DIRECTION ( 'NONE',  ( 0.000000000000000000, 0.000000000000000000, -1.000000000000000000 ) ) ;
#39508 = CARTESIAN_POINT ( 'NONE',  ( 4.201609111248720829, -18.99613120386805676, -1.500000000000002220 ) ) ;
#39509 = CARTESIAN_POINT ( 'NONE',  ( 6.029407872858970840, -20.54391778677962677, -1.500000000000002220 ) ) ;
#39510 = DIRECTION ( 'NONE',  ( -0.9980236263794188822, 0.000000000000000000, 0.06283980576413537855 ) ) ;
#39511 = CARTESIAN_POINT ( 'NONE',  ( -60.58331481027634879, -24.73531770709804078, 8.716586749031112191 ) ) ;
#39512 = DIRECTION ( 'NONE',  ( 1.000000000000000000, -0.000000000000000000, -0.000000000000000000 ) ) ;
#39513 = CARTESIAN_POINT ( 'NONE',  ( -44.52287095715005449, -23.95044443724991723, 10.65354141964648882 ) ) ;
#39514 = CARTESIAN_POINT ( 'NONE',  ( 4.020035926878589905, 22.33396232419688587, -1.500000000000002220 ) ) ;
#39515 = CARTESIAN_POINT ( 'NONE',  ( -98.63501208860351710, -23.73766607897669445, -1.055555164236453569 ) ) ;
#39516 = CARTESIAN_POINT ( 'NONE',  ( 15.22325621495362391, 2.682774720514426559, -27.23549315679322547 ) ) ;
#39517 = CARTESIAN_POINT ( 'NONE',  ( 15.03354914759215966, -12.96403794047452607, 11.49999999999999645 ) ) ;
#39518 = CARTESIAN_POINT ( 'NONE',  ( 5.627902640648289712, -6.376774720514413630, 20.02890049923285787 ) ) ;
#39519 = PLANE ( 'NONE',  #97612 ) ;
#39520 = CARTESIAN_POINT ( 'NONE',  ( -40.94687923781921768, -29.50249942614373921, 7.563164501610022405 ) ) ;
#39521 = ORIENTED_EDGE ( 'NONE', *, *, #32273, .F. ) ;
#39522 = DIRECTION ( 'NONE',  ( -2.313651251573816365E-16, 1.000000000000000000, -8.068660792749104624E-16 ) ) ;
#39523 = CARTESIAN_POINT ( 'NONE',  ( -6.275748223059703257, -5.876774720514411854, 19.59984006504824805 ) ) ;
#39524 = CIRCLE ( 'NONE', #52489, 251.4258649670780699 ) ;
#39525 = CARTESIAN_POINT ( 'NONE',  ( -51.19185979282234200, -25.27412279900076797, 3.072503657614854777 ) ) ;
#39526 = CARTESIAN_POINT ( 'NONE',  ( -0.4625342273119020797, 21.68341340789531912, -1.500000000000002220 ) ) ;
#39527 = CARTESIAN_POINT ( 'NONE',  ( -56.53760808179874431, -24.51419770103157347, 9.386484678747180510 ) ) ;
#39528 = CARTESIAN_POINT ( 'NONE',  ( 18.45204572605500104, 6.281640480902235701, -1.500000000000002220 ) ) ;
#39529 = CARTESIAN_POINT ( 'NONE',  ( -123.6228709571500701, -23.96177878511308634, 10.65340807706329684 ) ) ;
#39530 = EDGE_CURVE ( 'NONE', #81255, #89515, #11667, .T. ) ;
#39531 = VERTEX_POINT ( 'NONE', #18780 ) ;
#39532 = AXIS2_PLACEMENT_3D ( 'NONE', #90112, #90606, #20588 ) ;
#39533 = CARTESIAN_POINT ( 'NONE',  ( -18.95781532540867076, -7.450117396690965066, 11.49999999999999645 ) ) ;
#39534 = CARTESIAN_POINT ( 'NONE',  ( -80.62364778154437772, -25.00158670708910691, 2.256160236439221034 ) ) ;
#39535 = EDGE_CURVE ( 'NONE', #8654, #69272, #12294, .T. ) ;
#39536 = DIRECTION ( 'NONE',  ( -0.000000000000000000, -0.000000000000000000, -1.000000000000000000 ) ) ;
#39537 = ORIENTED_EDGE ( 'NONE', *, *, #80201, .T. ) ;
#39538 = CARTESIAN_POINT ( 'NONE',  ( -79.99253962700090881, -25.04791361497069957, 7.492507233463702399 ) ) ;
#39539 = CARTESIAN_POINT ( 'NONE',  ( -29.62287095715004526, -24.27255113093383088, 0.1850815668343412101 ) ) ;
#39540 = CARTESIAN_POINT ( 'NONE',  ( -48.99007696559036162, -25.31601964366231172, 5.618156375692663573 ) ) ;
#39541 = CARTESIAN_POINT ( 'NONE',  ( -40.47471336972785139, -24.83644354573577928, 8.397322867130096569 ) ) ;
#39542 = CARTESIAN_POINT ( 'NONE',  ( -89.40841769935767047, -25.05712065398430966, 7.447789548358837663 ) ) ;
#39543 = CARTESIAN_POINT ( 'NONE',  ( 6.297820759360134524, 19.07352124001985771, -1.500000000000002220 ) ) ;
#39544 = B_SPLINE_CURVE_WITH_KNOTS ( 'NONE', 3,
 ( #72756, #26065, #95577, #59027 ),
 .UNSPECIFIED., .F., .F.,
 ( 4, 4 ),
 ( 0.000000000000000000, 0.0001000000000000028644 ),
 .UNSPECIFIED. ) ;
#39545 = DIRECTION ( 'NONE',  ( 1.000000000000000000, 0.000000000000000000, 0.000000000000000000 ) ) ;
#39546 = ORIENTED_EDGE ( 'NONE', *, *, #83621, .T. ) ;
#39547 = CARTESIAN_POINT ( 'NONE',  ( -36.52287095715007581, -23.72747288104469732, -1.053458166803228124 ) ) ;
#39548 = CARTESIAN_POINT ( 'NONE',  ( -2.941484630304247450, -22.72858670154147376, 11.49999999999999645 ) ) ;
#39549 = CARTESIAN_POINT ( 'NONE',  ( -16.51154719052397724, 15.62863258182435189, 11.49999999999998934 ) ) ;
#39550 = ORIENTED_EDGE ( 'NONE', *, *, #50040, .T. ) ;
#39551 = CARTESIAN_POINT ( 'NONE',  ( -109.6228709571500417, -23.48783264082478794, -1.443836473390060382 ) ) ;
#39552 = CARTESIAN_POINT ( 'NONE',  ( -97.58953762381672448, -23.47593901973091235, -1.443836447539001089 ) ) ;
#39553 = CARTESIAN_POINT ( 'NONE',  ( -39.44687923781921057, -25.28830591450888221, 4.188173661249233959 ) ) ;
#39554 = LINE ( 'NONE', #32440, #72471 ) ;
#39555 = EDGE_CURVE ( 'NONE', #22708, #54184, #55502, .T. ) ;
#39556 = APPROVAL ( #13424, 'UNSPECIFIED' ) ;
#39557 = B_SPLINE_CURVE_WITH_KNOTS ( 'NONE', 3,
 ( #3315, #96145, #19505, #34246 ),
 .UNSPECIFIED., .F., .F.,
 ( 4, 4 ),
 ( 0.5301645019713113749, 0.5391709332434267976 ),
 .UNSPECIFIED. ) ;
#39558 = CARTESIAN_POINT ( 'NONE',  ( -128.5214463091758716, -24.51419770103157703, 9.386484678747171628 ) ) ;
#39559 = CARTESIAN_POINT ( 'NONE',  ( -34.62287095715005592, -24.65952944569303895, 1.056160979905691688 ) ) ;
#39560 = ORIENTED_EDGE ( 'NONE', *, *, #76556, .F. ) ;
#39561 = CARTESIAN_POINT ( 'NONE',  ( -5.191926799570463658, 19.71030214607805675, -1.500000000000002220 ) ) ;
#39562 = VERTEX_POINT ( 'NONE', #27407 ) ;
#39563 = B_SPLINE_CURVE_WITH_KNOTS ( 'NONE', 3,
 ( #28907, #37520, #61372, #75567, #84687, #5069, #6066, #22770 ),
 .UNSPECIFIED., .F., .F.,
 ( 4, 2, 2, 4 ),
 ( 0.000000000000000000, 0.2499999999999974465, 0.4999999999999948930, 1.000000000000000000 ),
 .UNSPECIFIED. ) ;
#39564 = CARTESIAN_POINT ( 'NONE',  ( -14.90462150274475306, 17.49973755783957685, -1.500000000000002220 ) ) ;
#39565 = CARTESIAN_POINT ( 'NONE',  ( -7.326695514711824231, -5.876774720514418071, 20.26757654895259719 ) ) ;
#39566 = CARTESIAN_POINT ( 'NONE',  ( -88.52287095715007581, -24.50216790748205398, 0.6166512839542540592 ) ) ;
#39568 = VERTEX_POINT ( 'NONE', #90799 ) ;
#39567 = ADVANCED_FACE ( 'NONE', ( #51238 ), #36007, .T. ) ;
#39569 = CARTESIAN_POINT ( 'NONE',  ( -122.5228709571500616, -24.65952944569305316, 1.056160979905705899 ) ) ;
#39570 = DIRECTION ( 'NONE',  ( 0.000000000000000000, 1.000000000000000000, -0.000000000000000000 ) ) ;
#39572 = ORIENTED_EDGE ( 'NONE', *, *, #4999, .T. ) ;
#39571 = CARTESIAN_POINT ( 'NONE',  ( -6.620899627221215944, -20.26055204357936290, 11.49999999999999645 ) ) ;
#39573 = ORIENTED_EDGE ( 'NONE', *, *, #85319, .F. ) ;
#39574 = CARTESIAN_POINT ( 'NONE',  ( -14.87450875942801254, -16.50811611944624602, -1.500000000000002220 ) ) ;
#39575 = CARTESIAN_POINT ( 'NONE',  ( 20.50092990308456464, -2.467789585553555654, -1.500000000000002220 ) ) ;
#39576 = AXIS2_PLACEMENT_3D ( 'NONE', #67999, #46660, #92812 ) ;
#39577 = VERTEX_POINT ( 'NONE', #68959 ) ;
#39578 = CARTESIAN_POINT ( 'NONE',  ( -112.6228709571500559, -24.64965695001469115, 8.947790433994176951 ) ) ;
#39579 = CARTESIAN_POINT ( 'NONE',  ( -95.58652046637003252, -24.73531770709095312, 8.716586749053508498 ) ) ;
#39580 = ORIENTED_EDGE ( 'NONE', *, *, #40107, .F. ) ;
#39581 = CARTESIAN_POINT ( 'NONE',  ( -111.9228709571500673, -23.47593901973090524, -1.443836447538996648 ) ) ;
#39582 = ORIENTED_EDGE ( 'NONE', *, *, #18835, .F. ) ;
#39583 = CARTESIAN_POINT ( 'NONE',  ( -93.62287095715005592, -23.47593901973091235, -1.443836447539002865 ) ) ;
#39584 = CARTESIAN_POINT ( 'NONE',  ( -115.9228709571500673, -23.47596703998600631, 11.44779298504227860 ) ) ;
#39585 = CARTESIAN_POINT ( 'NONE',  ( 12.70736309587848645, -16.60074808024427284, -1.500000000000002220 ) ) ;
#39586 = EDGE_CURVE ( 'NONE', #74711, #97718, #52245, .T. ) ;
#39587 = CARTESIAN_POINT ( 'NONE',  ( 19.92038474643397805, 8.973206291307779026, 11.49999999999999645 ) ) ;
#39588 = CARTESIAN_POINT ( 'NONE',  ( -27.07602811445854130, -24.89279971831744831, 7.457967357350439919 ) ) ;
#39589 = CARTESIAN_POINT ( 'NONE',  ( -99.05895993289298929, -25.17595066986875807, 6.775462437080328471 ) ) ;
#39590 = CARTESIAN_POINT ( 'NONE',  ( 22.44084908143146251, -0.7541981612834567361, -1.500000000000002220 ) ) ;
#39591 = CARTESIAN_POINT ( 'NONE',  ( -118.5191024237056325, -24.15620529776628800, 10.23563542870659759 ) ) ;
#39592 = DIRECTION ( 'NONE',  ( -0.9921023176230514551, 0.000000000000000000, 0.1254312216594016816 ) ) ;
#39593 = CARTESIAN_POINT ( 'NONE',  ( 4.854822496258163866, -5.876774720514422512, 20.96950945262037891 ) ) ;
#39594 = ORIENTED_EDGE ( 'NONE', *, *, #78333, .F. ) ;
#39595 = ORIENTED_EDGE ( 'NONE', *, *, #26088, .F. ) ;
#39596 = EDGE_CURVE ( 'NONE', #88353, #36769, #83171, .T. ) ;
#39597 = ORIENTED_EDGE ( 'NONE', *, *, #95374, .T. ) ;
#39598 = CARTESIAN_POINT ( 'NONE',  ( -21.18999663186871274, 2.814949255606389311, -1.500000000000002220 ) ) ;
#39599 = CARTESIAN_POINT ( 'NONE',  ( -22.26391555059773353, 2.265117081278330780, 11.49999999999999645 ) ) ;
#39600 = ORIENTED_EDGE ( 'NONE', *, *, #57924, .F. ) ;
#39601 = CARTESIAN_POINT ( 'NONE',  ( 3.661087877195506213, -20.73962600213626217, 11.49999999999998934 ) ) ;
#39602 = DIRECTION ( 'NONE',  ( -3.773278334453079030E-23, 0.9999999999976377785, 2.173523156925979128E-06 ) ) ;
#39603 = CARTESIAN_POINT ( 'NONE',  ( 12.75013301566243129, -15.34773647900153115, -1.500000000000002220 ) ) ;
#39604 = DIRECTION ( 'NONE',  ( 0.000000000000000000, 0.9513357669802769978, -0.3081562241202474572 ) ) ;
#39605 = CARTESIAN_POINT ( 'NONE',  ( -49.28939602672390663, -25.12437686555682248, 7.151409255195910752 ) ) ;
#39606 = CARTESIAN_POINT ( 'NONE',  ( -10.95654650054425794, 19.06054500580150446, -1.500000000000002220 ) ) ;
#39607 = DIRECTION ( 'NONE',  ( 0.000000000000000000, 1.000000000000000000, -8.393823270855521221E-16 ) ) ;
#39608 = ORIENTED_EDGE ( 'NONE', *, *, #27446, .F. ) ;
#39609 = CARTESIAN_POINT ( 'NONE',  ( -39.52287095715006870, -23.47593901973090524, -1.443836447538997092 ) ) ;
#39610 = EDGE_CURVE ( 'NONE', #80254, #31222, #98898, .T. ) ;
#39611 = CARTESIAN_POINT ( 'NONE',  ( -70.55620429048340725, -23.47593901973091235, -1.443836447539006196 ) ) ;
#39612 = CARTESIAN_POINT ( 'NONE',  ( -20.82185584224439978, -0.2524610531272265534, 11.49999999999999645 ) ) ;
#39613 = CARTESIAN_POINT ( 'NONE',  ( 31.67047468188982862, -5.333900073052421753, 28.72484383265714314 ) ) ;
#39614 = CARTESIAN_POINT ( 'NONE',  ( -40.62287095715005592, -29.50247984919015209, -1.443849546365060466 ) ) ;
#39615 = AXIS2_PLACEMENT_3D ( 'NONE', #28970, #21344, #90374 ) ;
#39616 = PLANE ( 'NONE',  #4360 ) ;
#39617 = CARTESIAN_POINT ( 'NONE',  ( -12.43717309395686499, -17.31322327496724611, 11.49999999999998934 ) ) ;
#39618 = CARTESIAN_POINT ( 'NONE',  ( -98.59947919455895260, -23.48786465467241058, 11.44779295918254114 ) ) ;
#39619 = CARTESIAN_POINT ( 'NONE',  ( -46.52287095715006160, -24.64965694238406613, 8.947790433994203596 ) ) ;
#39620 = CARTESIAN_POINT ( 'NONE',  ( -64.62365174556643410, -24.66019654487199730, 8.947790411086115725 ) ) ;
#39621 = CARTESIAN_POINT ( 'NONE',  ( -71.31679247717998749, -25.22594453560301631, 6.517383687127669134 ) ) ;
#39622 = CARTESIAN_POINT ( 'NONE',  ( -18.95691745938505335, -12.16397891629814865, -1.500000000000002220 ) ) ;
#39624 = CARTESIAN_POINT ( 'NONE',  ( -1.751198251822016161, 22.56127314141087581, 2.100000000000000089 ) ) ;
#39623 = B_SPLINE_CURVE_WITH_KNOTS ( 'NONE', 3,
 ( #5665, #68074, #36616, #21373, #52349, #83782, #75660, #45238 ),
 .UNSPECIFIED., .F., .F.,
 ( 4, 2, 2, 4 ),
 ( -0.001240666984356058331, -0.0002401179793396601269, 0.0007604310256767380771, 0.002761529035709534702 ),
 .UNSPECIFIED. ) ;
#39625 = VERTEX_POINT ( 'NONE', #66982 ) ;
#39626 = CARTESIAN_POINT ( 'NONE',  ( -51.52764846858840997, -25.25773520710183817, 6.187572766161611781 ) ) ;
#39627 = DIRECTION ( 'NONE',  ( 1.000000000000000000, 0.000000000000000000, -1.104558621438292892E-14 ) ) ;
#39628 = CARTESIAN_POINT ( 'NONE',  ( 19.69511366699831001, -0.05742560045514189665, 11.49999999999999645 ) ) ;
#39629 = CARTESIAN_POINT ( 'NONE',  ( -109.5228709571500616, -24.64965694238408034, 8.947790433994192938 ) ) ;
#39630 = B_SPLINE_CURVE_WITH_KNOTS ( 'NONE', 3,
 ( #25940, #65037, #49298, #2618, #4112, #95949 ),
 .UNSPECIFIED., .F., .F.,
 ( 4, 2, 4 ),
 ( 6.384118678611710879E-06, 0.001386860460828373467, 0.002767336802978134953 ),
 .UNSPECIFIED. ) ;
#39631 = CARTESIAN_POINT ( 'NONE',  ( 14.47945362154707816, -3.630796101029359679, -28.34983287945845731 ) ) ;
#39632 = ORIENTED_EDGE ( 'NONE', *, *, #45911, .T. ) ;
#39633 = CARTESIAN_POINT ( 'NONE',  ( -99.62355589612486995, -24.65952944569304961, 1.056160979905703901 ) ) ;
#39634 = DIRECTION ( 'NONE',  ( 0.000000000000000000, -1.000000000000000000, 0.000000000000000000 ) ) ;
#39635 = DIRECTION ( 'NONE',  ( 0.000000000000000000, -1.000000000000000000, 0.000000000000000000 ) ) ;
#39636 = CARTESIAN_POINT ( 'NONE',  ( 31.64143112576189765, -6.376774720514426953, 14.03360796525321774 ) ) ;
#39637 = CARTESIAN_POINT ( 'NONE',  ( 11.81298147481671279, -15.83112273922526470, 11.49999999999998934 ) ) ;
#39638 = ORIENTED_EDGE ( 'NONE', *, *, #72683, .T. ) ;
#39639 = CARTESIAN_POINT ( 'NONE',  ( 10.16466294932649106, 6.376774720514429617, -24.98589889747637116 ) ) ;
#39640 = VECTOR ( 'NONE', #5962, 1000.000000000000227 ) ;
#39641 = EDGE_CURVE ( 'NONE', #66316, #43365, #76549, .T. ) ;
#39642 = CALENDAR_DATE ( 2026, 9, 10 ) ;
#39643 = EDGE_LOOP ( 'NONE', ( #35126, #22447, #47104, #31863 ) ) ;
#39644 = CARTESIAN_POINT ( 'NONE',  ( -8.499999999999987566, 18.74999999999999645, 2.100000000000000089 ) ) ;
#39645 = CARTESIAN_POINT ( 'NONE',  ( 19.57151214508649772, 3.625915217019311583E-15, 0.000000000000000000 ) ) ;
#39646 = CARTESIAN_POINT ( 'NONE',  ( -10.16634758543296613, -5.965225279485572685, 30.00402280011862288 ) ) ;
#39647 = LINE ( 'NONE', #32038, #88193 ) ;
#39648 = CARTESIAN_POINT ( 'NONE',  ( -85.58953762381671027, -23.48783264082478794, -1.443836473390063713 ) ) ;
#39649 = LINE ( 'NONE', #62498, #55406 ) ;
#39650 = DIRECTION ( 'NONE',  ( 0.000000000000000000, -0.000000000000000000, -1.000000000000000000 ) ) ;
#39651 = CARTESIAN_POINT ( 'NONE',  ( -6.099057486122481997, -19.05896565686126110, 11.49999999999998934 ) ) ;
#39652 = CIRCLE ( 'NONE', #78540, 27.94799999999999685 ) ;
#39653 = CARTESIAN_POINT ( 'NONE',  ( 5.471383689419962337, -5.965225279485594001, -29.02273493113403902 ) ) ;
#39654 = CARTESIAN_POINT ( 'NONE',  ( 31.46635748159467383, -4.132774720514425404, -3.372935991075822759 ) ) ;
#39655 = VERTEX_POINT ( 'NONE', #6056 ) ;
#39656 = CARTESIAN_POINT ( 'NONE',  ( 8.599999999999999645, 24.84999999999999787, 2.100000000000000089 ) ) ;
#39657 = CARTESIAN_POINT ( 'NONE',  ( -109.3608459871604026, -25.18430332269756633, 4.114985099319373951 ) ) ;
#39658 = CARTESIAN_POINT ( 'NONE',  ( -35.59336923871764924, -24.40034930558991277, 0.3402023900116170063 ) ) ;
#39659 = CARTESIAN_POINT ( 'NONE',  ( -28.62287095715005236, -23.58365284793268302, 11.05752274016301584 ) ) ;
#39660 = CARTESIAN_POINT ( 'NONE',  ( -76.62287095715007013, -29.50250243563736774, 8.947779886222141599 ) ) ;
#39661 = DIRECTION ( 'NONE',  ( -3.773278334453079618E-23, 0.9999999999976377785, 2.173523156925978705E-06 ) ) ;
#39662 = EDGE_CURVE ( 'NONE', #82122, #88018, #20271, .T. ) ;
#39663 = CARTESIAN_POINT ( 'NONE',  ( -63.62287095715001328, -23.73934037231756378, 11.05740245334329153 ) ) ;
#39664 = ADVANCED_FACE ( 'NONE', ( #29393 ), #67975, .F. ) ;
#39665 = CARTESIAN_POINT ( 'NONE',  ( -50.40445135320380388, -25.18492896333868103, 3.293943116708552221 ) ) ;
#39666 = ORIENTED_EDGE ( 'NONE', *, *, #41191, .T. ) ;
#39667 = CARTESIAN_POINT ( 'NONE',  ( 6.837353022973060135, 19.10023500134885310, -1.500000000000002220 ) ) ;
#39668 = DIRECTION ( 'NONE',  ( 0.000000000000000000, 0.000000000000000000, -1.000000000000000000 ) ) ;
#39669 = EDGE_CURVE ( 'NONE', #9517, #44155, #80064, .T. ) ;
#39670 = CARTESIAN_POINT ( 'NONE',  ( -59.48966412625335920, -24.66019654487199730, 8.947790411086124607 ) ) ;
#39671 = EDGE_CURVE ( 'NONE', #19988, #21619, #15888, .T. ) ;
#39672 = EDGE_LOOP ( 'NONE', ( #38581, #29233, #81776, #73969 ) ) ;
#39673 = FACE_OUTER_BOUND ( 'NONE', #60486, .T. ) ;
#39674 = CARTESIAN_POINT ( 'NONE',  ( 8.007726535620864894, 18.53121347637897287, -1.500000000000002220 ) ) ;
#39675 = CARTESIAN_POINT ( 'NONE',  ( -18.40674794014382698, -10.35651468716735657, 11.49999999999999645 ) ) ;
#39676 = EDGE_CURVE ( 'NONE', #32756, #37373, #70356, .T. ) ;
#39677 = CIRCLE ( 'NONE', #13744, 2.500000000000000444 ) ;
#39678 = CARTESIAN_POINT ( 'NONE',  ( -21.04927197579530329, -6.814310187297170529, -1.500000000000002220 ) ) ;
#39679 = CARTESIAN_POINT ( 'NONE',  ( -17.31529204923715071, 11.11782870402162260, -1.500000000000002220 ) ) ;
#39680 = CARTESIAN_POINT ( 'NONE',  ( 15.99960863614630391, 3.577630190450220571, -27.91116951066582175 ) ) ;
#39681 = ORIENTED_EDGE ( 'NONE', *, *, #21343, .T. ) ;
#39682 = FACE_OUTER_BOUND ( 'NONE', #75803, .T. ) ;
#39683 = ORIENTED_EDGE ( 'NONE', *, *, #3859, .F. ) ;
#39684 = LINE ( 'NONE', #76728, #17137 ) ;
#39685 = CARTESIAN_POINT ( 'NONE',  ( -110.6228709571500559, -23.85229601348996908, 10.88205029486208808 ) ) ;
#39686 = ORIENTED_EDGE ( 'NONE', *, *, #90892, .F. ) ;
#39687 = ORIENTED_EDGE ( 'NONE', *, *, #26422, .T. ) ;
#39688 = VERTEX_POINT ( 'NONE', #67468 ) ;
#39689 = CARTESIAN_POINT ( 'NONE',  ( -110.7007163551309361, -25.12832023213188037, 2.875934489414091466 ) ) ;
#39690 = CARTESIAN_POINT ( 'NONE',  ( 7.155337544004596317, -6.376774720514417183, 20.64714842558261765 ) ) ;
#39691 = CARTESIAN_POINT ( 'NONE',  ( -68.55392418078596961, -23.96169478059712787, 10.65365249895718414 ) ) ;
#39692 = CARTESIAN_POINT ( 'NONE',  ( -20.55277978778089576, -2.218614319624547360, -1.500000000000002220 ) ) ;
#39693 = ADVANCED_FACE ( 'NONE', ( #76061 ), #6560, .T. ) ;
#39694 = CARTESIAN_POINT ( 'NONE',  ( 19.61570337458852364, 9.273991169892711994, 11.49999999999999645 ) ) ;
#39695 = VERTEX_POINT ( 'NONE', #37509 ) ;
#39696 = FACE_OUTER_BOUND ( 'NONE', #42738, .T. ) ;
#39697 = CARTESIAN_POINT ( 'NONE',  ( 2.993128331772667572, -5.876774720514403860, 18.53171057923899312 ) ) ;
#39698 = CARTESIAN_POINT ( 'NONE',  ( 3.752539591237177508, -22.04708138622333635, -1.500000000000002220 ) ) ;
#39699 = CARTESIAN_POINT ( 'NONE',  ( -79.34687923781920915, -25.12205563760222304, 5.960409599525325675 ) ) ;
#39700 = CARTESIAN_POINT ( 'NONE',  ( -84.50376481693795938, -24.51314013834316441, 0.6176544820404183955 ) ) ;
#39701 = VERTEX_POINT ( 'NONE', #59350 ) ;
#39702 = CARTESIAN_POINT ( 'NONE',  ( -118.8947150340837311, -25.34770440169397787, 6.200377556431414305 ) ) ;
#39703 = CARTESIAN_POINT ( 'NONE',  ( -76.62287095715005592, -24.33927499327854704, 9.819080762295818943 ) ) ;
#39704 = ORIENTED_EDGE ( 'NONE', *, *, #88838, .F. ) ;
#39705 = VECTOR ( 'NONE', #51284, 1000.000000000000114 ) ;
#39707 = EDGE_CURVE ( 'NONE', #6225, #39922, #68464, .T. ) ;
#39706 = CARTESIAN_POINT ( 'NONE',  ( -70.62287095715004170, -23.48783264082478084, -1.443836473390067265 ) ) ;
#39708 = ORIENTED_EDGE ( 'NONE', *, *, #20090, .T. ) ;
#39709 = CARTESIAN_POINT ( 'NONE',  ( -109.5906666788849009, -24.15620529776628800, 10.23563542870660115 ) ) ;
#39710 = CARTESIAN_POINT ( 'NONE',  ( -14.79452276021403634, 15.15755283273500531, -1.500000000000002220 ) ) ;
#39711 = EDGE_CURVE ( 'NONE', #55090, #90388, #30390, .T. ) ;
#39712 = EDGE_LOOP ( 'NONE', ( #76844, #81735, #67010, #49442 ) ) ;
#39713 = CARTESIAN_POINT ( 'NONE',  ( -50.60042094805579183, -24.15503026093913164, -0.2815557561904566963 ) ) ;
#39714 = CARTESIAN_POINT ( 'NONE',  ( -16.21501377034323710, -14.60173171477820198, -1.500000000000002220 ) ) ;
#39715 = CARTESIAN_POINT ( 'NONE',  ( -7.491187506528125262, -6.376774720514410077, 19.53857357749109980 ) ) ;
#39716 = CARTESIAN_POINT ( 'NONE',  ( -52.62287095715005592, -29.50250786944525672, 11.44777988621624054 ) ) ;
#39717 = CARTESIAN_POINT ( 'NONE',  ( 5.271800844963591359, 6.376774720514426953, -28.56638892015329034 ) ) ;
#39718 = CARTESIAN_POINT ( 'NONE',  ( -5.167225684058948332, 21.16526716281445530, -1.500000000000002220 ) ) ;
#39719 = CARTESIAN_POINT ( 'NONE',  ( -1.174900045708346497, -6.376774720514411854, 19.48569229636960998 ) ) ;
#39720 = ORIENTED_EDGE ( 'NONE', *, *, #53212, .T. ) ;
#39721 = DIRECTION ( 'NONE',  ( 0.5656310827093757876, 2.995395837334948684E-15, -0.8246584009594636333 ) ) ;
#39722 = CARTESIAN_POINT ( 'NONE',  ( -85.51575146014167217, -23.85049219812685450, 10.88485053497527133 ) ) ;
#39724 = VERTEX_POINT ( 'NONE', #53246 ) ;
#39723 = EDGE_CURVE ( 'NONE', #13349, #51586, #51746, .T. ) ;
#39725 = VECTOR ( 'NONE', #92002, 1000.000000000000000 ) ;
#39726 = VECTOR ( 'NONE', #92964, 1000.000000000000000 ) ;
#39727 = ADVANCED_FACE ( 'NONE', ( #82679 ), #37012, .T. ) ;
#39728 = ORIENTED_EDGE ( 'NONE', *, *, #5552, .T. ) ;
#39729 = ADVANCED_FACE ( 'NONE', ( #9057 ), #62874, .T. ) ;
#39730 = ORIENTED_EDGE ( 'NONE', *, *, #71933, .F. ) ;
#39731 = DIRECTION ( 'NONE',  ( 0.9913618264504691080, -7.885106708985488048E-16, -0.1311553622875927805 ) ) ;
#39732 = CARTESIAN_POINT ( 'NONE',  ( -113.6228709571500417, -24.51283580621365132, 0.6167428607019899145 ) ) ;
#39733 = CARTESIAN_POINT ( 'NONE',  ( -19.98547761299008130, 7.154247560337752887, -1.500000000000002220 ) ) ;
#39734 = CARTESIAN_POINT ( 'NONE',  ( -121.6228709571500417, -24.64898659630368627, 1.056161002820833028 ) ) ;
#39735 = CARTESIAN_POINT ( 'NONE',  ( -30.61048516611183601, -24.43626637953622804, 0.1835287498755953373 ) ) ;
#39736 = CARTESIAN_POINT ( 'NONE',  ( -38.62287095715005592, -29.50247984919015209, -1.443849546365060466 ) ) ;
#39737 = FACE_OUTER_BOUND ( 'NONE', #33, .T. ) ;
#39738 = CARTESIAN_POINT ( 'NONE',  ( 2.844571010020486845, -19.19604305453586690, 11.49999999999998934 ) ) ;
#39739 = CARTESIAN_POINT ( 'NONE',  ( -41.89562512939934891, -25.03707806782366418, 7.590868867492675420 ) ) ;
#39740 = EDGE_LOOP ( 'NONE', ( #74011, #87375, #90015, #60433 ) ) ;
#39741 = CARTESIAN_POINT ( 'NONE',  ( -1.849579639615634097, -19.42000222497389927, 11.49999999999999645 ) ) ;
#39742 = CARTESIAN_POINT ( 'NONE',  ( -42.52287095715005449, -24.50321055353804311, 9.387540953477529371 ) ) ;
#39743 = CARTESIAN_POINT ( 'NONE',  ( -79.57618923056713811, -25.19206956779440887, 6.661130867067107886 ) ) ;
#39744 = ORIENTED_EDGE ( 'NONE', *, *, #45458, .F. ) ;
#39745 = CARTESIAN_POINT ( 'NONE',  ( 4.966987340572156739, -6.376774720514417183, 20.16530235339958210 ) ) ;
#39746 = DIRECTION ( 'NONE',  ( 0.000000000000000000, 0.000000000000000000, 1.000000000000000000 ) ) ;
#39747 = CARTESIAN_POINT ( 'NONE',  ( -103.5895376238167387, -23.47593901973091235, -1.443836447539001089 ) ) ;
#39748 = CARTESIAN_POINT ( 'NONE',  ( -93.51533444581417598, -23.96169478059713853, 10.65365249895717348 ) ) ;
#39749 = CARTESIAN_POINT ( 'NONE',  ( -3.719764837209879271, -19.30396570740023421, -1.500000000000002220 ) ) ;
#39750 = CARTESIAN_POINT ( 'NONE',  ( -41.15947890742572923, -25.31583714713193700, 4.822226109655245452 ) ) ;
#39751 = ORIENTED_EDGE ( 'NONE', *, *, #70513, .F. ) ;
#39752 = VECTOR ( 'NONE', #22053, 1000.000000000000000 ) ;
#39753 = CARTESIAN_POINT ( 'NONE',  ( 21.54666897473465070, 1.519730039111064412, -1.500000000000002220 ) ) ;
#39754 = DIRECTION ( 'NONE',  ( 0.000000000000000000, 0.000000000000000000, 1.000000000000000000 ) ) ;
#39755 = FACE_OUTER_BOUND ( 'NONE', #37060, .T. ) ;
#39756 = CARTESIAN_POINT ( 'NONE',  ( -13.34915495237762251, 18.83725853537101358, -1.500000000000002220 ) ) ;
#39757 = APPROVAL_STATUS ( 'not_yet_approved' ) ;
#39758 = CARTESIAN_POINT ( 'NONE',  ( -92.22287095715005023, -23.47593901973090169, -1.443836447538996870 ) ) ;
#39759 = CARTESIAN_POINT ( 'NONE',  ( -130.5728709571500588, -23.47593901973090524, -1.443836447538995982 ) ) ;
#39760 = DIRECTION ( 'NONE',  ( 3.773278334444166432E-23, -1.000000000000000000, 0.000000000000000000 ) ) ;
#39761 = DIRECTION ( 'NONE',  ( -1.000000000000000000, 0.000000000000000000, 0.000000000000000000 ) ) ;
#39762 = CARTESIAN_POINT ( 'NONE',  ( -111.6658724870577117, -25.29824007310582701, 3.734855809897266621 ) ) ;
#39763 = CARTESIAN_POINT ( 'NONE',  ( -98.52287095715009002, -23.72747288104470798, -1.053458166803226126 ) ) ;
#39764 = FACE_OUTER_BOUND ( 'NONE', #24430, .T. ) ;
#39765 = CARTESIAN_POINT ( 'NONE',  ( 2.927915493035635031, 19.71835975189664936, -1.500000000000002220 ) ) ;
#39766 = CARTESIAN_POINT ( 'NONE',  ( -75.54453366976977691, -24.52399227489127043, 9.353111116836526406 ) ) ;
#39767 = CARTESIAN_POINT ( 'NONE',  ( -17.59554656748941071, 9.132484154288260214, -1.500000000000002220 ) ) ;
#39768 = ORIENTED_EDGE ( 'NONE', *, *, #28886, .F. ) ;
#39769 = CARTESIAN_POINT ( 'NONE',  ( -56.55997151016966029, -23.73766607897670511, -1.055555164236459342 ) ) ;
#39770 = CARTESIAN_POINT ( 'NONE',  ( -39.04303308397305727, -25.10925892954523064, 4.215217319642836635 ) ) ;
#39771 = FACE_OUTER_BOUND ( 'NONE', #92885, .T. ) ;
#39772 = CARTESIAN_POINT ( 'NONE',  ( -18.43438512255917772, -9.567967903218889347, 11.49999999999999645 ) ) ;
#39773 = CARTESIAN_POINT ( 'NONE',  ( -100.6814946224345846, -29.50249328176098729, 4.736241424693623081 ) ) ;
#39774 = CIRCLE ( 'NONE', #901, 15.00000000000000178 ) ;
#39775 = CARTESIAN_POINT ( 'NONE',  ( -106.5908035580171287, -24.15543982623907127, -0.2315651400026576268 ) ) ;
#39776 = CARTESIAN_POINT ( 'NONE',  ( -10.92962168092244823, 19.99562239114850826, 11.49999999999999645 ) ) ;
#39777 = CIRCLE ( 'NONE', #54362, 0.8160000000000007248 ) ;
#39779 = EDGE_CURVE ( 'NONE', #52807, #20892, #38701, .T. ) ;
#39778 = ORIENTED_EDGE ( 'NONE', *, *, #20418, .T. ) ;
#39780 = CARTESIAN_POINT ( 'NONE',  ( -7.662324775236974972, 31.59999999999999787, 2.100000000000000089 ) ) ;
#39782 = EDGE_CURVE ( 'NONE', #62158, #89034, #3686, .T. ) ;
#39781 = CARTESIAN_POINT ( 'NONE',  ( -70.26171360675115807, -25.12330951983202709, 7.099796482853127699 ) ) ;
#39783 = ORIENTED_EDGE ( 'NONE', *, *, #62995, .F. ) ;
#39784 = VECTOR ( 'NONE', #34503, 1000.000000000000000 ) ;
#39785 = CARTESIAN_POINT ( 'NONE',  ( -19.33604739795523741, 5.927148246271303655, 11.49999999999998934 ) ) ;
#39786 = DIRECTION ( 'NONE',  ( -0.000000000000000000, 2.173523156925979552E-06, -0.9999999999976378895 ) ) ;
#39787 = AXIS2_PLACEMENT_3D ( 'NONE', #66853, #66359, #28269 ) ;
#39788 = EDGE_CURVE ( 'NONE', #50965, #57581, #7558, .T. ) ;
#39789 = CARTESIAN_POINT ( 'NONE',  ( -110.5228709571500048, -24.15516710230294350, 10.28746687063725140 ) ) ;
#39790 = ADVANCED_FACE ( 'NONE', ( #86182 ), #94288, .F. ) ;
#39791 = CIRCLE ( 'NONE', #88417, 19.00000000000000355 ) ;
#39792 = EDGE_CURVE ( 'NONE', #21561, #28755, #27939, .T. ) ;
#39793 = B_SPLINE_CURVE_WITH_KNOTS ( 'NONE', 3,
 ( #69348, #44519, #37900, #91673, #5450, #67362 ),
 .UNSPECIFIED., .F., .F.,
 ( 4, 2, 4 ),
 ( 6.391158118966174708E-06, 0.001387004593080782677, 0.002767618028042598960 ),
 .UNSPECIFIED. ) ;
#39794 = VERTEX_POINT ( 'NONE', #40523 ) ;
#39795 = CARTESIAN_POINT ( 'NONE',  ( -125.5228709571500616, -23.47593901973090524, -1.443836447538996204 ) ) ;
#39796 = CARTESIAN_POINT ( 'NONE',  ( 7.457602374657920308, -21.66695214233757838, -1.500000000000002220 ) ) ;
#39797 = CARTESIAN_POINT ( 'NONE',  ( -50.67443072449054853, -25.18439655831317836, 3.321634571026201854 ) ) ;
#39798 = CARTESIAN_POINT ( 'NONE',  ( -18.23705311251027794, 8.147635122911419003, -1.500000000000002220 ) ) ;
#39799 = FACE_OUTER_BOUND ( 'NONE', #89549, .T. ) ;
#39800 = CARTESIAN_POINT ( 'NONE',  ( 5.581485548573628996, 20.18083795961418403, 11.49999999999999645 ) ) ;
#39801 = VERTEX_POINT ( 'NONE', #1962 ) ;
#39802 = ADVANCED_FACE ( 'NONE', ( #92291 ), #22763, .F. ) ;
#39803 = CARTESIAN_POINT ( 'NONE',  ( -89.52287095715003318, -23.48783264083374789, -1.443836473376144180 ) ) ;
#39804 = CARTESIAN_POINT ( 'NONE',  ( -69.53040046975404209, -25.24754292466213101, 5.066170387013165133 ) ) ;
#39805 = CARTESIAN_POINT ( 'NONE',  ( -20.26759042640731323, -8.618136523154847239, 11.49999999999998934 ) ) ;
#39806 = DIRECTION ( 'NONE',  ( -1.000000000000000000, 0.000000000000000000, 0.000000000000000000 ) ) ;
#39807 = VERTEX_POINT ( 'NONE', #92784 ) ;
#39808 = CARTESIAN_POINT ( 'NONE',  ( -118.5228709571500474, -23.73934037231757443, 11.05740245334327909 ) ) ;
#39809 = CARTESIAN_POINT ( 'NONE',  ( -122.6228709571500417, -23.47596703998600631, 11.44779298504227860 ) ) ;
#39810 = B_SPLINE_CURVE_WITH_KNOTS ( 'NONE', 3,
 ( #25303, #9081, #86701, #69980 ),
 .UNSPECIFIED., .F., .F.,
 ( 4, 4 ),
 ( 0.000000000000000000, 9.999999999998897304E-05 ),
 .UNSPECIFIED. ) ;
#39811 = ORIENTED_EDGE ( 'NONE', *, *, #13804, .T. ) ;
#39812 = CARTESIAN_POINT ( 'NONE',  ( 2.834823996951755465, -6.376774720514406525, 18.76222163777333307 ) ) ;
#39813 = VERTEX_POINT ( 'NONE', #85178 ) ;
#39814 = EDGE_LOOP ( 'NONE', ( #32955, #51053, #63045, #99999 ) ) ;
#39815 = CARTESIAN_POINT ( 'NONE',  ( -101.3738023147422638, -25.26303730729093999, 3.986250639247583827 ) ) ;
#39816 = CARTESIAN_POINT ( 'NONE',  ( -100.5578068411443837, -25.27404630875477665, 2.834635289093140109 ) ) ;
#39817 = CARTESIAN_POINT ( 'NONE',  ( -4.165021623707020559, -6.376774720514417183, 20.26087634804756377 ) ) ;
#39818 = CARTESIAN_POINT ( 'NONE',  ( 20.25987197511681259, 2.754759976156288204, -1.500000000000002220 ) ) ;
#39819 = EDGE_CURVE ( 'NONE', #20097, #86154, #57260, .T. ) ;
#39820 = ORIENTED_EDGE ( 'NONE', *, *, #95820, .T. ) ;
#39821 = LINE ( 'NONE', #31714, #93172 ) ;
#39822 = CARTESIAN_POINT ( 'NONE',  ( -33.62287095715005592, -23.96177878511307568, 10.65340807706330573 ) ) ;
#39823 = CARTESIAN_POINT ( 'NONE',  ( 14.15579980161844986, 3.316774720514426456, -28.31186755866361437 ) ) ;
#39824 = CARTESIAN_POINT ( 'NONE',  ( 22.20884612314100792, -2.053178116692622623, -1.500000000000002220 ) ) ;
#39825 = DIRECTION ( 'NONE',  ( -0.000000000000000000, -1.000000000000000000, -0.000000000000000000 ) ) ;
#39826 = DIRECTION ( 'NONE',  ( 1.000000000000000000, 0.000000000000000000, 0.000000000000000000 ) ) ;
#39827 = EDGE_CURVE ( 'NONE', #82876, #50012, #81130, .T. ) ;
#39828 = VERTEX_POINT ( 'NONE', #80071 ) ;
#39829 = CARTESIAN_POINT ( 'NONE',  ( -27.89347163551325792, -24.62105267781937457, 1.634524268193336072 ) ) ;
#39830 = CARTESIAN_POINT ( 'NONE',  ( -118.5228709571500900, -24.33832256527048798, 0.1851278514138662290 ) ) ;
#39831 = VECTOR ( 'NONE', #16829, 1000.000000000000000 ) ;
#39832 = CARTESIAN_POINT ( 'NONE',  ( -16.21995886604411297, 13.06735728859114509, -1.500000000000002220 ) ) ;
#39833 = ORIENTED_EDGE ( 'NONE', *, *, #73694, .F. ) ;
#39836 = ORIENTED_EDGE ( 'NONE', *, *, #54445, .T. ) ;
#39835 = ADVANCED_FACE ( 'NONE', ( #11549 ), #50622, .T. ) ;
#39834 = CARTESIAN_POINT ( 'NONE',  ( -79.52287095715006160, -23.48786465467241058, 11.44779295918254469 ) ) ;
#39837 = ORIENTED_EDGE ( 'NONE', *, *, #54819, .F. ) ;
#39838 = DIRECTION ( 'NONE',  ( 1.000000000000000000, 4.218136541796977197E-15, 0.000000000000000000 ) ) ;
#39839 = CARTESIAN_POINT ( 'NONE',  ( -20.73700405699343463, 3.470425206167693233, -1.500000000000002220 ) ) ;
#39840 = VERTEX_POINT ( 'NONE', #34900 ) ;
#39841 = CARTESIAN_POINT ( 'NONE',  ( -37.52287095715006870, -24.64965694238406613, 8.947790433994205372 ) ) ;
#39842 = LINE ( 'NONE', #33230, #87122 ) ;
#39843 = LINE ( 'NONE', #1295, #85337 ) ;
#39844 = CARTESIAN_POINT ( 'NONE',  ( -101.8248201165894073, -25.25419362369936849, 6.680466494418182855 ) ) ;
#39845 = CARTESIAN_POINT ( 'NONE',  ( -60.62287095715004881, -24.51254535404256174, 9.355368623467651190 ) ) ;
#39846 = LINE ( 'NONE', #79406, #33566 ) ;
#39848 = ORIENTED_EDGE ( 'NONE', *, *, #77380, .T. ) ;
#39847 = CARTESIAN_POINT ( 'NONE',  ( 13.49617185221842952, 17.62045156095830123, 11.49999999999999645 ) ) ;
#39849 = CARTESIAN_POINT ( 'NONE',  ( -39.52287095715006870, -29.50250786944525672, 11.44777988621624232 ) ) ;
#39850 = CARTESIAN_POINT ( 'NONE',  ( -38.62287095715005592, -23.73907113216990794, -1.053371485793235918 ) ) ;
#39851 = ORIENTED_EDGE ( 'NONE', *, *, #21614, .T. ) ;
#39852 = CARTESIAN_POINT ( 'NONE',  ( -16.08347380570801377, -15.98036338121420030, 11.49999999999998934 ) ) ;
#39853 = ADVANCED_FACE ( 'NONE', ( #73462 ), #50129, .F. ) ;
#39855 = VERTEX_POINT ( 'NONE', #41514 ) ;
#39854 = DIRECTION ( 'NONE',  ( -3.773278334453079030E-23, 0.9999999999976377785, 2.173523156925979128E-06 ) ) ;
#39856 = ORIENTED_EDGE ( 'NONE', *, *, #84822, .F. ) ;
#39857 = CARTESIAN_POINT ( 'NONE',  ( 13.91401389203221406, 0.3587747205144265483, 158.0376437107427137 ) ) ;
#39858 = ADVANCED_FACE ( 'NONE', ( #64882 ), #77555, .T. ) ;
#39859 = B_SPLINE_CURVE_WITH_KNOTS ( 'NONE', 3,
 ( #84016, #84517, #77390, #15996, #99235, #39341, #46460, #62198 ),
 .UNSPECIFIED., .F., .F.,
 ( 4, 2, 2, 4 ),
 ( 0.000000000000000000, 0.002001079623178221491, 0.003001619434767333755, 0.004002159246356446452 ),
 .UNSPECIFIED. ) ;
#39860 = VECTOR ( 'NONE', #57301, 1000.000000000000114 ) ;
#39861 = CARTESIAN_POINT ( 'NONE',  ( 18.53703574427524359, 7.882278514257341051, 11.49999999999998934 ) ) ;
#39862 = CARTESIAN_POINT ( 'NONE',  ( -80.62287095715001328, -24.92579138211019085, 1.929029949965667123 ) ) ;
#39863 = VERTEX_POINT ( 'NONE', #25279 ) ;
#39864 = VECTOR ( 'NONE', #31978, 1000.000000000000000 ) ;
#39865 = CARTESIAN_POINT ( 'NONE',  ( -39.04303308397305727, -29.50249214928227914, 4.215207770848699020 ) ) ;
#39866 = CARTESIAN_POINT ( 'NONE',  ( -12.73782554413503654, -18.45060914899308457, -1.500000000000002220 ) ) ;
#39867 = AXIS2_PLACEMENT_3D ( 'NONE', #24284, #78550, #18169 ) ;
#39868 = ADVANCED_FACE ( 'NONE', ( #56257 ), #81073, .F. ) ;
#39869 = AXIS2_PLACEMENT_3D ( 'NONE', #55373, #93914, #70083 ) ;
#39870 = ORIENTED_EDGE ( 'NONE', *, *, #49137, .T. ) ;
#39871 = VERTEX_POINT ( 'NONE', #79569 ) ;
#39872 = CARTESIAN_POINT ( 'NONE',  ( -112.5905324053159262, -24.15620529776628445, 10.23563542870659582 ) ) ;
#39873 = CARTESIAN_POINT ( 'NONE',  ( -4.169309590939843879, -6.376774720514411854, 19.59793130852656518 ) ) ;
#39874 = DIRECTION ( 'NONE',  ( 0.000000000000000000, 0.9999999999976377785, 2.173523156925979975E-06 ) ) ;
#39875 = CARTESIAN_POINT ( 'NONE',  ( -122.6228709571500417, -29.50248528299804818, 1.056150453629045360 ) ) ;
#39876 = CARTESIAN_POINT ( 'NONE',  ( -97.25162849029662482, -24.37807914296825729, 0.3010598746230577216 ) ) ;
#39877 = CARTESIAN_POINT ( 'NONE',  ( -0.9579564967699066846, 19.55851204243107233, -1.500000000000002220 ) ) ;
#39878 = CARTESIAN_POINT ( 'NONE',  ( -5.378122165843598701, -5.876774720514410077, 19.21968329462762526 ) ) ;
#39879 = VERTEX_POINT ( 'NONE', #10058 ) ;
#39880 = CARTESIAN_POINT ( 'NONE',  ( 21.44729954461699251, -1.519088741117538000, -1.500000000000002220 ) ) ;
#39881 = CARTESIAN_POINT ( 'NONE',  ( -31.62287095715005236, -29.50250243563736774, 8.947779886222150481 ) ) ;
#39882 = CARTESIAN_POINT ( 'NONE',  ( -7.160000000000000142, 7.891155995661682354, 6.788828319098143993 ) ) ;
#39883 = CARTESIAN_POINT ( 'NONE',  ( -19.38764004357183168, -0.3587747205143967943, -21.62823517627351322 ) ) ;
#39884 = CARTESIAN_POINT ( 'NONE',  ( -80.62287095715004170, -24.82576562982391977, 8.398263435472973271 ) ) ;
#39885 = CARTESIAN_POINT ( 'NONE',  ( -9.675568039816649701, -20.77828039667204862, -1.500000000000002220 ) ) ;
#39886 = DATE_AND_TIME ( #53632, #24548 ) ;
#39887 = CARTESIAN_POINT ( 'NONE',  ( -96.51589611984518058, -23.96169478059713498, 10.65365249895717881 ) ) ;
#39888 = CARTESIAN_POINT ( 'NONE',  ( -2.283364382221138467, -5.876774720514412742, 19.46427715384223944 ) ) ;
#39889 = CARTESIAN_POINT ( 'NONE',  ( 12.62869658624171976, -15.57725692549414376, 11.49999999999999645 ) ) ;
#39890 = CARTESIAN_POINT ( 'NONE',  ( -79.79643364552497076, -25.31594337936764205, 4.606720419479115591 ) ) ;
#39891 = FACE_OUTER_BOUND ( 'NONE', #6759, .T. ) ;
#39892 = CARTESIAN_POINT ( 'NONE',  ( 4.531089049250198286, -5.876774720514405637, 18.46391971337801508 ) ) ;
#39893 = DIRECTION ( 'NONE',  ( 0.000000000000000000, -1.000000000000000000, 0.000000000000000000 ) ) ;
#39894 = VERTEX_POINT ( 'NONE', #71974 ) ;
#39895 = CARTESIAN_POINT ( 'NONE',  ( -83.62287095715005592, -29.50250243563736774, 8.947779886222141599 ) ) ;
#39896 = CARTESIAN_POINT ( 'NONE',  ( 21.40858030128615397, -3.853468400179685727, 11.49999999999998934 ) ) ;
#39897 = LINE ( 'NONE', #38896, #90126 ) ;
#39898 = CARTESIAN_POINT ( 'NONE',  ( -0.7274468246531539117, 19.66889477801398911, -1.500000000000002220 ) ) ;
#39899 = AXIS2_PLACEMENT_3D ( 'NONE', #71602, #2100, #33033 ) ;
#39900 = DIRECTION ( 'NONE',  ( 3.773278334444166432E-23, -1.000000000000000000, 0.000000000000000000 ) ) ;
#39901 = CARTESIAN_POINT ( 'NONE',  ( -104.5895376238167245, -23.48786465467241413, 11.44779295918254114 ) ) ;
#39902 = CALENDAR_DATE ( 2026, 9, 10 ) ;
#39903 = CARTESIAN_POINT ( 'NONE',  ( -91.54630222961577601, -24.51419770103159124, 9.386484678747176957 ) ) ;
#39904 = CARTESIAN_POINT ( 'NONE',  ( 2.611202098145462891, -6.376774720514420736, 20.45574432200782766 ) ) ;
#39905 = CARTESIAN_POINT ( 'NONE',  ( -16.28974412851428255, -12.55652860423730388, 11.49999999999999645 ) ) ;
#39906 = CARTESIAN_POINT ( 'NONE',  ( -24.90875734969025501, 6.376774720514426953, 30.51402280011862089 ) ) ;
#39907 = CARTESIAN_POINT ( 'NONE',  ( -120.5208179319231476, -23.85016227208581441, -0.8807180028928250914 ) ) ;
#39908 = CARTESIAN_POINT ( 'NONE',  ( -21.41681981171885951, -7.298096547245328303, 11.49999999999999645 ) ) ;
#39909 = ORIENTED_EDGE ( 'NONE', *, *, #16723, .F. ) ;
#39910 = EDGE_CURVE ( 'NONE', #60838, #55188, #2455, .T. ) ;
#39911 = CARTESIAN_POINT ( 'NONE',  ( -99.82150581108260212, -25.26387405423741583, 4.513512927829998134 ) ) ;
#39912 = LINE ( 'NONE', #71879, #59144 ) ;
#39914 = EDGE_CURVE ( 'NONE', #27902, #38599, #13363, .T. ) ;
#39913 = CARTESIAN_POINT ( 'NONE',  ( -125.5204572650066552, -24.40133493613050675, 9.663955038902798833 ) ) ;
#39915 = DIRECTION ( 'NONE',  ( -0.000000000000000000, -1.000000000000000000, -0.000000000000000000 ) ) ;
#39916 = EDGE_CURVE ( 'NONE', #21576, #65701, #25782, .T. ) ;
#39917 = CARTESIAN_POINT ( 'NONE',  ( -33.62287095715007013, -23.94994826722565762, -0.6494450866342740269 ) ) ;
#39918 = ADVANCED_FACE ( 'NONE', ( #53128 ), #36886, .T. ) ;
#39919 = PLANE ( 'NONE',  #36614 ) ;
#39920 = EDGE_CURVE ( 'NONE', #63059, #451, #27779, .T. ) ;
#39921 = VECTOR ( 'NONE', #28403, 1000.000000000000114 ) ;
#39922 = VERTEX_POINT ( 'NONE', #89681 ) ;
#39923 = CARTESIAN_POINT ( 'NONE',  ( -80.09072421954219578, -25.26749884311348282, 5.004106523481387292 ) ) ;
#39924 = CARTESIAN_POINT ( 'NONE',  ( -19.65108876255925807, -11.61119296138784662, -1.500000000000002220 ) ) ;
#39925 = CARTESIAN_POINT ( 'NONE',  ( 3.903461913076534451, -5.876774720514404748, 18.52532880998198905 ) ) ;
#39926 = CARTESIAN_POINT ( 'NONE',  ( -96.63021477443740537, -24.15543982623907482, -0.2315651400026596807 ) ) ;
#39927 = CARTESIAN_POINT ( 'NONE',  ( -63.62744501956971277, -24.51419770103158058, 9.386484678747173405 ) ) ;
#39928 = CARTESIAN_POINT ( 'NONE',  ( -15.60622653811170402, 16.18669697583415967, 11.49999999999999645 ) ) ;
#39929 = VERTEX_POINT ( 'NONE', #75935 ) ;
#39930 = CARTESIAN_POINT ( 'NONE',  ( 10.24059822343757808, -5.876774720514426953, 17.91871304725684766 ) ) ;
#39931 = CARTESIAN_POINT ( 'NONE',  ( 21.92589416912191069, -1.073809401359021143, -1.500000000000002220 ) ) ;
#39932 = DIRECTION ( 'NONE',  ( -0.9921023176230514551, 0.000000000000000000, 0.1254312216594016816 ) ) ;
#39933 = AXIS2_PLACEMENT_3D ( 'NONE', #92939, #71628, #15819 ) ;
#39934 = CARTESIAN_POINT ( 'NONE',  ( -44.58706610318112951, -24.35071581493542681, 9.817618358456025263 ) ) ;
#39935 = FACE_OUTER_BOUND ( 'NONE', #77489, .T. ) ;
#39936 = ORIENTED_EDGE ( 'NONE', *, *, #23551, .F. ) ;
#39937 = PLANE ( 'NONE',  #617 ) ;
#39938 = LINE ( 'NONE', #70900, #56616 ) ;
#39939 = VERTEX_POINT ( 'NONE', #74452 ) ;
#39940 = AXIS2_PLACEMENT_3D ( 'NONE', #41082, #86243, #93850 ) ;
#39941 = CARTESIAN_POINT ( 'NONE',  ( -12.74120943341865342, -16.01528480738631899, 11.49999999999998934 ) ) ;
#39942 = VERTEX_POINT ( 'NONE', #97292 ) ;
#39943 = AXIS2_PLACEMENT_3D ( 'NONE', #95616, #1772, #11377 ) ;
#39944 = VERTEX_POINT ( 'NONE', #59740 ) ;
#39945 = ORIENTED_EDGE ( 'NONE', *, *, #30441, .T. ) ;
#39946 = ORIENTED_EDGE ( 'NONE', *, *, #98079, .F. ) ;
#39947 = CARTESIAN_POINT ( 'NONE',  ( 10.36671515591691950, -20.60271000134967068, -1.500000000000002220 ) ) ;
#39948 = DIRECTION ( 'NONE',  ( 0.000000000000000000, 0.000000000000000000, 1.000000000000000000 ) ) ;
#39949 = CARTESIAN_POINT ( 'NONE',  ( -20.26613141553852060, -1.498020344548873561, -1.500000000000002220 ) ) ;
#39950 = ORIENTED_EDGE ( 'NONE', *, *, #4546, .F. ) ;
#39951 = CARTESIAN_POINT ( 'NONE',  ( 29.73860345376319003, -1.682774720514426114, -1.272392034746785860 ) ) ;
#39952 = CARTESIAN_POINT ( 'NONE',  ( -40.62287095715004170, -24.99156045073392463, 7.747789690856161648 ) ) ;
#39953 = CIRCLE ( 'NONE', #10834, 19.30000000000000071 ) ;
#39954 = CARTESIAN_POINT ( 'NONE',  ( -99.52287095715006160, -29.50250243563736774, 8.947779886222138046 ) ) ;
#39955 = CARTESIAN_POINT ( 'NONE',  ( 4.639502537026700679, -5.876774720514416295, 19.60647575951318800 ) ) ;
#39957 = ORIENTED_EDGE ( 'NONE', *, *, #42476, .F. ) ;
#39956 = CARTESIAN_POINT ( 'NONE',  ( -20.40864349294084334, -6.676163967499375573, 11.49999999999999645 ) ) ;
#39958 = CARTESIAN_POINT ( 'NONE',  ( -79.62287095715007013, -24.66019654487199375, 8.947790411086128159 ) ) ;
#39959 = CARTESIAN_POINT ( 'NONE',  ( -93.52287095715007581, -23.95044443724993144, 10.65354141964648882 ) ) ;
#39960 = ORIENTED_EDGE ( 'NONE', *, *, #82673, .F. ) ;
#39961 = CARTESIAN_POINT ( 'NONE',  ( 19.63682106917175929, 6.691539877478525966, -1.500000000000002220 ) ) ;
#39962 = VERTEX_POINT ( 'NONE', #66860 ) ;
#39964 = ORIENTED_EDGE ( 'NONE', *, *, #14167, .T. ) ;
#39963 = CARTESIAN_POINT ( 'NONE',  ( -125.5541640623637250, -24.92564183028979485, 1.928384488918254425 ) ) ;
#39965 = CARTESIAN_POINT ( 'NONE',  ( -111.5512703140825863, -24.51419770103157703, 9.386484678747162747 ) ) ;
#39966 = DIRECTION ( 'NONE',  ( 0.000000000000000000, 0.000000000000000000, 1.000000000000000000 ) ) ;
#39967 = ORIENTED_EDGE ( 'NONE', *, *, #99711, .T. ) ;
#39968 = ORIENTED_EDGE ( 'NONE', *, *, #65724, .F. ) ;
#39969 = CARTESIAN_POINT ( 'NONE',  ( -40.52287095715007581, -24.83602698348160231, 1.605859176311261960 ) ) ;
#39970 = CARTESIAN_POINT ( 'NONE',  ( -42.53972667629340521, -24.35071581493542681, 9.817618358456037697 ) ) ;
#39971 = CARTESIAN_POINT ( 'NONE',  ( -78.52287095715006160, -24.64898659630367916, 1.056161002820826145 ) ) ;
#39972 = CARTESIAN_POINT ( 'NONE',  ( -10.13730173486854369, -19.54584281717935568, 11.49999999999999645 ) ) ;
#39973 = CARTESIAN_POINT ( 'NONE',  ( -89.59823446461851404, -23.73791477778911840, 11.05961554403170233 ) ) ;
#39974 = CARTESIAN_POINT ( 'NONE',  ( -16.68516988606489448, 15.22057433622007316, -1.500000000000002220 ) ) ;
#39975 = EDGE_CURVE ( 'NONE', #98189, #40469, #8533, .T. ) ;
#39976 = VECTOR ( 'NONE', #14104, 1000.000000000000114 ) ;
#39977 = CARTESIAN_POINT ( 'NONE',  ( -1.027814097295878693, -20.98676634966329146, -1.500000000000002220 ) ) ;
#39979 = VERTEX_POINT ( 'NONE', #74932 ) ;
#39978 = PLANE ( 'NONE',  #42558 ) ;
#39980 = B_SPLINE_CURVE_WITH_KNOTS ( 'NONE', 3,
 ( #26160, #19043, #42414, #78934, #72348, #11435, #96669, #88568, #56130, #2844, #58129, #94668, #18048, #89066 ),
 .UNSPECIFIED., .F., .F.,
 ( 4, 2, 2, 2, 2, 2, 4 ),
 ( 0.000000000000000000, 0.0002404508101542971810, 0.0004809016203085943620, 0.0009618032406171489338, 0.001442704860925703722, 0.001683155671079981062, 0.001923606481234258186 ),
 .UNSPECIFIED. ) ;
#39981 = VERTEX_POINT ( 'NONE', #6439 ) ;
#39982 = AXIS2_PLACEMENT_3D ( 'NONE', #93010, #54468, #70188 ) ;
#39983 = DIRECTION ( 'NONE',  ( 0.000000000000000000, -0.9999999999976377785, -2.173523156925979128E-06 ) ) ;
#39984 = EDGE_CURVE ( 'NONE', #11247, #14389, #84056, .T. ) ;
#39985 = EDGE_CURVE ( 'NONE', #25180, #41495, #49703, .T. ) ;
#39986 = CARTESIAN_POINT ( 'NONE',  ( -90.62287095715005592, -24.91570333823099759, 8.075032458375558164 ) ) ;
#39987 = VERTEX_POINT ( 'NONE', #22143 ) ;
#39988 = CARTESIAN_POINT ( 'NONE',  ( 21.14167878903947084, -0.5806874866175276706, -1.500000000000002220 ) ) ;
#39989 = CARTESIAN_POINT ( 'NONE',  ( -117.5228709571500758, -23.47593901973090524, -1.443836447538996204 ) ) ;
#39990 = CARTESIAN_POINT ( 'NONE',  ( -51.32936205048392964, -25.03148689476321564, 7.321356269641313474 ) ) ;
#39991 = CARTESIAN_POINT ( 'NONE',  ( -121.5901305642217807, -24.15543982623907482, -0.2315651400026574047 ) ) ;
#39992 = CARTESIAN_POINT ( 'NONE',  ( -51.92287095715005307, -23.47593901973090169, -1.443836447538997758 ) ) ;
#39993 = CARTESIAN_POINT ( 'NONE',  ( -127.5228709571500616, -23.96177878511310411, 10.65340807706329684 ) ) ;
#39994 = CARTESIAN_POINT ( 'NONE',  ( 21.93305185196877360, -3.456643806985262302, -1.500000000000002220 ) ) ;
#39995 = DIRECTION ( 'NONE',  ( 1.000000000000000000, 1.232047923278981953E-16, 0.000000000000000000 ) ) ;
#39996 = VERTEX_POINT ( 'NONE', #36389 ) ;
#39997 = CARTESIAN_POINT ( 'NONE',  ( -51.04357394935764347, -25.24859992533754038, 4.940878074475977044 ) ) ;
#39998 = CARTESIAN_POINT ( 'NONE',  ( -37.59389932947581059, -24.15543982623907127, -0.2315651400026566831 ) ) ;
#39999 = DIRECTION ( 'NONE',  ( 0.000000000000000000, 1.000000000000000000, 0.000000000000000000 ) ) ;
#40000 = AXIS2_PLACEMENT_3D ( 'NONE', #24645, #7928, #55627 ) ;
#40001 = CARTESIAN_POINT ( 'NONE',  ( -75.62287095715005592, -23.47593901973091235, -1.443836447539004642 ) ) ;
#40002 = CARTESIAN_POINT ( 'NONE',  ( -100.5192865818111159, -25.11060891163327469, 2.833917758948478305 ) ) ;
#40003 = CARTESIAN_POINT ( 'NONE',  ( 18.45204572605500104, 6.281640480902235701, 11.49999999999998934 ) ) ;
#40004 = CARTESIAN_POINT ( 'NONE',  ( 9.091334071971768793, -19.38302982324925239, -1.500000000000002220 ) ) ;
#40005 = CARTESIAN_POINT ( 'NONE',  ( -85.52287095715006160, -24.14406661686761169, 10.28769366194077861 ) ) ;
#40006 = PLANE ( 'NONE',  #93314 ) ;
#40007 = CARTESIAN_POINT ( 'NONE',  ( -51.64512162636743398, -23.96119346886880663, -0.6495511937832119109 ) ) ;
#40008 = DIRECTION ( 'NONE',  ( -1.000000000000000000, -3.773278334444166432E-23, -8.201307841325785021E-29 ) ) ;
#40009 = CARTESIAN_POINT ( 'NONE',  ( 15.30562342774392093, -16.77826389816909725, -1.500000000000002220 ) ) ;
#40010 = CIRCLE ( 'NONE', #25443, 1.700000000000000178 ) ;
#40011 = AXIS2_PLACEMENT_3D ( 'NONE', #89011, #42847, #50447 ) ;
#40012 = CARTESIAN_POINT ( 'NONE',  ( -32.62287095715004881, -23.48786465467240347, 11.44779295918255535 ) ) ;
#40013 = CARTESIAN_POINT ( 'NONE',  ( 8.071512145086522594, -7.528487854913504584, 6.500000000000000888 ) ) ;
#40014 = CARTESIAN_POINT ( 'NONE',  ( 13.99221305778824487, -14.08248706038611964, 11.49999999999999645 ) ) ;
#40015 = CARTESIAN_POINT ( 'NONE',  ( -123.6234902540211493, -24.66019654487200441, 8.947790411086106843 ) ) ;
#40016 = VECTOR ( 'NONE', #27983, 1000.000000000000114 ) ;
#40017 = B_SPLINE_CURVE_WITH_KNOTS ( 'NONE', 3,
 ( #40488, #48614, #94260, #86651, #24743, #95269 ),
 .UNSPECIFIED., .F., .F.,
 ( 4, 2, 4 ),
 ( 0.000000000000000000, 0.001380764517854761713, 0.002761529035709523426 ),
 .UNSPECIFIED. ) ;
#40018 = CARTESIAN_POINT ( 'NONE',  ( -54.52287095715006870, -23.47596703998600631, 11.44779298504229104 ) ) ;
#40019 = B_SPLINE_CURVE_WITH_KNOTS ( 'NONE', 3,
 ( #48084, #55704, #79010, #9508 ),
 .UNSPECIFIED., .F., .F.,
 ( 4, 4 ),
 ( 0.000000000000000000, 9.999999999998900014E-05 ),
 .UNSPECIFIED. ) ;
#40020 = CARTESIAN_POINT ( 'NONE',  ( 33.69795529655567634, -6.475225279485573360, 20.86760796525322093 ) ) ;
#40021 = ORIENTED_EDGE ( 'NONE', *, *, #95038, .F. ) ;
#40022 = CARTESIAN_POINT ( 'NONE',  ( 18.72495633783376334, -0.5000000000000000000, -1.691563534834430227 ) ) ;
#40023 = CARTESIAN_POINT ( 'NONE',  ( -6.100820854657341918, -6.376774720514413630, 19.76359802465961124 ) ) ;
#40024 = CARTESIAN_POINT ( 'NONE',  ( -117.5895376238167387, -24.66019654487199730, 8.947790411086122830 ) ) ;
#40025 = CARTESIAN_POINT ( 'NONE',  ( -21.63489631200954122, -1.325961216813365429, -1.500000000000002220 ) ) ;
#40026 = CARTESIAN_POINT ( 'NONE',  ( 12.92500000000000249, 1.999999999999999556, 24.00000000000000000 ) ) ;
#40028 = VECTOR ( 'NONE', #76659, 1000.000000000000114 ) ;
#40027 = CARTESIAN_POINT ( 'NONE',  ( 0.2958748881272694198, 19.47992435465491212, -1.500000000000002220 ) ) ;
#40029 = CARTESIAN_POINT ( 'NONE',  ( -55.53421905444260176, -24.73531770709095312, 8.716586749053510275 ) ) ;
#40030 = ADVANCED_FACE ( 'NONE', ( #82557 ), #60243, .F. ) ;
#40031 = VERTEX_POINT ( 'NONE', #59233 ) ;
#40032 = CARTESIAN_POINT ( 'NONE',  ( -11.21218820807429140, -16.99972530465495169, 11.49999999999999645 ) ) ;
#40033 = DIRECTION ( 'NONE',  ( 0.000000000000000000, -1.000000000000000000, 1.478457507934778393E-16 ) ) ;
#40034 = CARTESIAN_POINT ( 'NONE',  ( -19.77875734969026311, 6.143225279485574397, 27.35402280011862430 ) ) ;
#40035 = ORIENTED_EDGE ( 'NONE', *, *, #37532, .F. ) ;
#40036 = CARTESIAN_POINT ( 'NONE',  ( -24.57525087998974200, 0.3587747205143967943, -15.45548830044932664 ) ) ;
#40037 = CARTESIAN_POINT ( 'NONE',  ( -29.62287095715005592, -23.40871900810292772, -1.443836166241315055 ) ) ;
#40038 = CARTESIAN_POINT ( 'NONE',  ( -39.49170631829002787, -25.27985531019455578, 5.433214399821440388 ) ) ;
#40039 = EDGE_CURVE ( 'NONE', #30746, #21858, #91170, .T. ) ;
#40040 = CARTESIAN_POINT ( 'NONE',  ( -40.47824818423304549, -24.73531770709094957, 8.716586749053510275 ) ) ;
#40041 = CARTESIAN_POINT ( 'NONE',  ( -0.9827876235267493099, -5.876774720514415407, 19.81240905262004404 ) ) ;
#40042 = CARTESIAN_POINT ( 'NONE',  ( 18.81927703376926786, -7.057843677351100631, 11.49999999999998934 ) ) ;
#40043 = FACE_OUTER_BOUND ( 'NONE', #92229, .T. ) ;
#40045 = VERTEX_POINT ( 'NONE', #91663 ) ;
#40044 = EDGE_CURVE ( 'NONE', #65926, #30754, #52614, .T. ) ;
#40046 = CARTESIAN_POINT ( 'NONE',  ( -66.65280601721215703, -23.48786465467241058, 11.44779295918254824 ) ) ;
#40047 = VECTOR ( 'NONE', #89268, 1000.000000000000114 ) ;
#40048 = EDGE_CURVE ( 'NONE', #63904, #9871, #14035, .T. ) ;
#40049 = CARTESIAN_POINT ( 'NONE',  ( 7.334040449947802465, -21.76207178258647090, 11.49999999999999645 ) ) ;
#40050 = B_SPLINE_CURVE_WITH_KNOTS ( 'NONE', 3,
 ( #11177, #49261, #26403, #80188 ),
 .UNSPECIFIED., .F., .F.,
 ( 4, 4 ),
 ( 0.3807718998933248833, 0.3897783311654404725 ),
 .UNSPECIFIED. ) ;
#40051 = CARTESIAN_POINT ( 'NONE',  ( -4.086358941109507370, -22.34742993483353146, 11.49999999999998934 ) ) ;
#40052 = ORIENTED_EDGE ( 'NONE', *, *, #8924, .F. ) ;
#40053 = CARTESIAN_POINT ( 'NONE',  ( -109.6228709571500133, -24.51283580621365132, 0.6167428607019883602 ) ) ;
#40054 = EDGE_CURVE ( 'NONE', #28486, #74103, #45785, .T. ) ;
#40055 = CARTESIAN_POINT ( 'NONE',  ( -98.52287095715000476, -24.51283580621364067, 0.6167428607019795894 ) ) ;
#40056 = CARTESIAN_POINT ( 'NONE',  ( -40.39538329754159918, -25.19528640796965036, 3.295757161197724550 ) ) ;
#40057 = AXIS2_PLACEMENT_3D ( 'NONE', #31257, #61234, #23635 ) ;
#40058 = ADVANCED_FACE ( 'NONE', ( #13535 ), #66365, .T. ) ;
#40059 = CARTESIAN_POINT ( 'NONE',  ( -61.59189125704997281, -25.08279362854488781, 7.371166896404004909 ) ) ;
#40060 = B_SPLINE_CURVE_WITH_KNOTS ( 'NONE', 3,
 ( #22273, #54261, #13666, #77065, #85190, #100392 ),
 .UNSPECIFIED., .F., .F.,
 ( 4, 2, 4 ),
 ( 6.384118678608373569E-06, 0.001386860460828372816, 0.002767336802978137555 ),
 .UNSPECIFIED. ) ;
#40061 = LINE ( 'NONE', #71015, #30000 ) ;
#40062 = CARTESIAN_POINT ( 'NONE',  ( -26.09636659181000695, -24.95932275238217102, 4.940287574183225061 ) ) ;
#40063 = CARTESIAN_POINT ( 'NONE',  ( -61.52287095715006870, -23.94994826722564696, -0.6494450866342758033 ) ) ;
#40064 = DIRECTION ( 'NONE',  ( -0.000000000000000000, 1.000000000000000000, -0.000000000000000000 ) ) ;
#40065 = ORIENTED_EDGE ( 'NONE', *, *, #1923, .F. ) ;
#40066 = CARTESIAN_POINT ( 'NONE',  ( 18.82465703714932204, -7.861812626244089053, -1.500000000000002220 ) ) ;
#40067 = EDGE_LOOP ( 'NONE', ( #51898, #4298 ) ) ;
#40068 = ADVANCED_FACE ( 'NONE', ( #51624, #43515, #35890, #13040, #90178, #54126, #15038 ), #68840, .T. ) ;
#40069 = CARTESIAN_POINT ( 'NONE',  ( -16.88208375265294237, -15.58181570610299715, 11.49999999999998934 ) ) ;
#40070 = CARTESIAN_POINT ( 'NONE',  ( -7.234140626586239797, -5.876774720514411854, 19.72789237585158162 ) ) ;
#40071 = ORIENTED_EDGE ( 'NONE', *, *, #11154, .F. ) ;
#40072 = DIRECTION ( 'NONE',  ( 1.000000000000000000, -0.000000000000000000, -0.000000000000000000 ) ) ;
#40073 = VECTOR ( 'NONE', #63986, 1000.000000000000000 ) ;
#40074 = CARTESIAN_POINT ( 'NONE',  ( -118.5228709571500758, -24.65952944569305316, 1.056160979905705899 ) ) ;
#40075 = FACE_BOUND ( 'NONE', #60851, .T. ) ;
#40077 = VERTEX_POINT ( 'NONE', #37887 ) ;
#40076 = CARTESIAN_POINT ( 'NONE',  ( 20.93798385506118365, 3.901641247904229282, 11.49999999999999645 ) ) ;
#40078 = VERTEX_POINT ( 'NONE', #6935 ) ;
#40079 = CARTESIAN_POINT ( 'NONE',  ( -21.14947813473477822, 6.846651710974520633, 11.49999999999998934 ) ) ;
#40080 = CARTESIAN_POINT ( 'NONE',  ( 18.87225196054570020, 8.368929400942139551, -1.500000000000002220 ) ) ;
#40081 = VECTOR ( 'NONE', #92110, 1000.000000000000114 ) ;
#40082 = ORIENTED_EDGE ( 'NONE', *, *, #11967, .T. ) ;
#40083 = CARTESIAN_POINT ( 'NONE',  ( 0.3910256410256394144, -6.376774720514411854, 19.63681891025641235 ) ) ;
#40084 = CARTESIAN_POINT ( 'NONE',  ( -70.79417929288042899, -25.11539253604531297, 2.804427796191110378 ) ) ;
#40085 = ORIENTED_EDGE ( 'NONE', *, *, #27114, .T. ) ;
#40086 = CARTESIAN_POINT ( 'NONE',  ( -127.5228709571500616, -24.64898659630368627, 1.056161002820834804 ) ) ;
#40087 = VERTEX_POINT ( 'NONE', #24153 ) ;
#40088 = CARTESIAN_POINT ( 'NONE',  ( -58.56687466182343371, -23.48786465467241413, 11.44779295918254647 ) ) ;
#40089 = DIRECTION ( 'NONE',  ( 0.000000000000000000, 0.9999999999976377785, 2.173523156925979975E-06 ) ) ;
#40090 = CARTESIAN_POINT ( 'NONE',  ( 2.550444227103870531, -20.70361394434535285, -1.500000000000002220 ) ) ;
#40092 = ADVANCED_FACE ( 'NONE', ( #92164, #39384 ), #7929, .F. ) ;
#40091 = CARTESIAN_POINT ( 'NONE',  ( -9.754611696910345131, 19.53525426502628548, 11.49999999999999645 ) ) ;
#40093 = CARTESIAN_POINT ( 'NONE',  ( -27.47736343186643637, -24.77993795937362975, 7.597050500966643583 ) ) ;
#40094 = CARTESIAN_POINT ( 'NONE',  ( 15.30859874843628354, 3.492299066144916697, -27.16052374892713317 ) ) ;
#40095 = CARTESIAN_POINT ( 'NONE',  ( 16.76845895467136671, -15.01613412638008782, 11.49999999999998934 ) ) ;
#40096 = CARTESIAN_POINT ( 'NONE',  ( -118.6258445754143338, -24.15620529776628800, 10.23563542870659582 ) ) ;
#40097 = EDGE_CURVE ( 'NONE', #3112, #34388, #320, .T. ) ;
#40098 = CARTESIAN_POINT ( 'NONE',  ( -4.568292318365942073, -5.965225279485572685, 30.06720597538392425 ) ) ;
#40099 = CARTESIAN_POINT ( 'NONE',  ( 22.33191539159815164, 2.682774720514426559, -16.26852658953823649 ) ) ;
#40100 = ORIENTED_EDGE ( 'NONE', *, *, #86072, .T. ) ;
#40101 = ORIENTED_EDGE ( 'NONE', *, *, #9948, .F. ) ;
#40102 = ORIENTED_EDGE ( 'NONE', *, *, #57614, .T. ) ;
#40103 = EDGE_CURVE ( 'NONE', #99816, #30369, #71443, .T. ) ;
#40104 = ORIENTED_EDGE ( 'NONE', *, *, #15983, .F. ) ;
#40105 = CARTESIAN_POINT ( 'NONE',  ( -15.65470850568805083, 14.63654280257262386, -1.500000000000002220 ) ) ;
#40107 = EDGE_CURVE ( 'NONE', #80389, #32056, #23138, .T. ) ;
#40106 = CARTESIAN_POINT ( 'NONE',  ( 19.44376294880228428, 11.01865886811674677, 11.49999999999999645 ) ) ;
#40108 = VERTEX_POINT ( 'NONE', #23646 ) ;
#40109 = LINE ( 'NONE', #22486, #34307 ) ;
#40110 = CARTESIAN_POINT ( 'NONE',  ( 17.02745815656931683, -12.38318283856952107, 11.49999999999998934 ) ) ;
#40111 = CARTESIAN_POINT ( 'NONE',  ( -30.58285055587994705, -25.15098267793663922, 7.291421475381018702 ) ) ;
#40112 = CARTESIAN_POINT ( 'NONE',  ( -19.59816365915598979, -3.832847594873297403, -1.500000000000002220 ) ) ;
#40113 = CARTESIAN_POINT ( 'NONE',  ( -117.6228709571500559, -23.48783264082479505, -1.443836473390058384 ) ) ;
#40114 = CARTESIAN_POINT ( 'NONE',  ( -11.64875734969026233, -0.3587747205144265483, 30.51402280011862089 ) ) ;
#40115 = CARTESIAN_POINT ( 'NONE',  ( 8.687672273659204691, 20.25853876245846408, -1.500000000000002220 ) ) ;
#40116 = CARTESIAN_POINT ( 'NONE',  ( -83.52287095715006160, -23.47593901973090524, -1.443836447538996648 ) ) ;
#40117 = ORIENTED_EDGE ( 'NONE', *, *, #89874, .T. ) ;
#40118 = DIRECTION ( 'NONE',  ( -1.000000000000000000, -3.773278334444167608E-23, -8.201307833595939069E-29 ) ) ;
#40119 = CARTESIAN_POINT ( 'NONE',  ( -126.6228709571500843, -23.47596703998600631, 11.44779298504227860 ) ) ;
#40120 = CARTESIAN_POINT ( 'NONE',  ( 15.14581745102402088, -14.33592658440916523, 11.49999999999999645 ) ) ;
#40121 = VECTOR ( 'NONE', #19001, 1000.000000000000000 ) ;
#40122 = CARTESIAN_POINT ( 'NONE',  ( 31.69157588112856061, -3.316774720514426456, 29.47507169338741662 ) ) ;
#40123 = CARTESIAN_POINT ( 'NONE',  ( -32.07722060962684196, -24.87479601683932984, 8.247789944617052171 ) ) ;
#40124 = VECTOR ( 'NONE', #98020, 1000.000000000000000 ) ;
#40125 = DIRECTION ( 'NONE',  ( 0.000000000000000000, 0.000000000000000000, 1.000000000000000000 ) ) ;
#40126 = CARTESIAN_POINT ( 'NONE',  ( -16.81368161134402683, 13.12552177539105358, 11.49999999999998934 ) ) ;
#40127 = LINE ( 'NONE', #48247, #93590 ) ;
#40128 = CARTESIAN_POINT ( 'NONE',  ( -10.34999999999997833, 22.00000000000000000, 2.100000000000000089 ) ) ;
#40129 = DIRECTION ( 'NONE',  ( 0.000000000000000000, -1.000000000000000000, 0.000000000000000000 ) ) ;
#40130 = CARTESIAN_POINT ( 'NONE',  ( 22.74089357256066535, 4.772774720514425972, -19.20396252371061863 ) ) ;
#40131 = CC_DESIGN_PERSON_AND_ORGANIZATION_ASSIGNMENT ( #99027, #6193, ( #63621 ) ) ;
#40132 = CARTESIAN_POINT ( 'NONE',  ( -22.39070119279581306, -2.479732019442284496, -1.500000000000002220 ) ) ;
#40133 = B_SPLINE_CURVE_WITH_KNOTS ( 'NONE', 3,
 ( #85896, #15876, #15373, #85387 ),
 .UNSPECIFIED., .F., .F.,
 ( 4, 4 ),
 ( 0.2989766979437447625, 0.2999774449845101221 ),
 .UNSPECIFIED. ) ;
#40134 = B_SPLINE_SURFACE_WITH_KNOTS ( 'NONE', 3, 3, ( 
 ( #33192, #25580, #56554, #72271 ),
 ( #29069, #4748, #59040, #20951 ),
 ( #44810, #36197, #13835, #67656 ),
 ( #75243, #97585, #12346, #5239 ),
 ( #35202, #42822, #27590, #13336 ),
 ( #83352, #28577, #58541, #90476 ),
 ( #67161, #98574, #90971, #59537 ),
 ( #43317, #66173, #60042, #74742 ),
 ( #73753, #21440, #11853, #52420 ),
 ( #98069, #81369, #75730, #97092 ) ),
 .UNSPECIFIED., .F., .F., .F.,
 ( 4, 3, 3, 4 ),
 ( 4, 4 ),
 ( 0.7022005934544807149, 0.7765311282028795059, 0.8508616629512784080, 0.9995227324480762121 ),
 ( 0.5995663561115596174, 0.6009364140660176101 ),
 .UNSPECIFIED. ) ;
#40135 = CARTESIAN_POINT ( 'NONE',  ( -89.06226385320381667, -25.23397913219354294, 6.409327625488849378 ) ) ;
#40136 = ORIENTED_EDGE ( 'NONE', *, *, #9303, .F. ) ;
#40137 = CYLINDRICAL_SURFACE ( 'NONE', #4517, 1.530000000000001359 ) ;
#40138 = CARTESIAN_POINT ( 'NONE',  ( -31.51235681150392409, -23.73791477778911130, 11.05961554403171299 ) ) ;
#40139 = CARTESIAN_POINT ( 'NONE',  ( -19.15055961920884542, -4.482958728538418924, 11.49999999999999645 ) ) ;
#40140 = LINE ( 'NONE', #33028, #65084 ) ;
#40141 = DIRECTION ( 'NONE',  ( 3.773278334444166432E-23, -1.000000000000000000, 0.000000000000000000 ) ) ;
#40142 = ORIENTED_EDGE ( 'NONE', *, *, #76912, .T. ) ;
#40143 = CARTESIAN_POINT ( 'NONE',  ( -99.50802952236794852, -24.65952944569304961, 1.056160979905703901 ) ) ;
#40144 = DIRECTION ( 'NONE',  ( -3.773278334453079618E-23, 0.9999999999976377785, 2.173523156925979975E-06 ) ) ;
#40145 = CARTESIAN_POINT ( 'NONE',  ( -124.5915517817484073, -23.48786465467241769, 11.44779295918253581 ) ) ;
#40146 = VECTOR ( 'NONE', #67, 1000.000000000000000 ) ;
#40147 = CARTESIAN_POINT ( 'NONE',  ( 16.30000000000000071, 21.89999999999999858, 0.000000000000000000 ) ) ;
#40148 = CARTESIAN_POINT ( 'NONE',  ( -3.970774856468506364, -19.35638658347046714, 11.49999999999998934 ) ) ;
#40149 = ORIENTED_EDGE ( 'NONE', *, *, #8302, .F. ) ;
#40150 = CARTESIAN_POINT ( 'NONE',  ( 17.48260522047220888, -10.12088315688240314, 11.49999999999999645 ) ) ;
#40151 = CARTESIAN_POINT ( 'NONE',  ( 5.771117285127500551, -5.876774720514418071, 20.39900056875960388 ) ) ;
#40152 = AXIS2_PLACEMENT_3D ( 'NONE', #4151, #21345, #81767 ) ;
#40153 = VERTEX_POINT ( 'NONE', #77924 ) ;
#40154 = CARTESIAN_POINT ( 'NONE',  ( -48.62287095715004881, -23.72773821059535493, 11.05748984161097503 ) ) ;
#40155 = FACE_OUTER_BOUND ( 'NONE', #24414, .T. ) ;
#40156 = CARTESIAN_POINT ( 'NONE',  ( -88.88918693012686845, -25.23397913219354649, 6.409327625488847602 ) ) ;
#40157 = LINE ( 'NONE', #71113, #69582 ) ;
#40158 = AXIS2_PLACEMENT_3D ( 'NONE', #87293, #79680, #18289 ) ;
#40159 = FACE_OUTER_BOUND ( 'NONE', #17485, .T. ) ;
#40160 = DIRECTION ( 'NONE',  ( -3.773278334444167608E-23, 1.000000000000000000, 0.000000000000000000 ) ) ;
#40162 = ADVANCED_FACE ( 'NONE', ( #61242 ), #38877, .F. ) ;
#40161 = CARTESIAN_POINT ( 'NONE',  ( -16.84340083857899018, -10.81494551495373457, 11.49999999999998934 ) ) ;
#40163 = CARTESIAN_POINT ( 'NONE',  ( -99.13021050592293193, -25.10935259592492841, 3.853445119336080804 ) ) ;
#40164 = PLANE ( 'NONE',  #69483 ) ;
#40165 = ORIENTED_EDGE ( 'NONE', *, *, #53692, .F. ) ;
#40166 = B_SPLINE_CURVE_WITH_KNOTS ( 'NONE', 3,
 ( #95532, #20386, #3695, #11296 ),
 .UNSPECIFIED., .F., .F.,
 ( 4, 4 ),
 ( 0.2106504203089220317, 0.2196568515810378708 ),
 .UNSPECIFIED. ) ;
#40167 = CARTESIAN_POINT ( 'NONE',  ( -79.60527230392054321, -23.48786465467241058, 11.44779295918254824 ) ) ;
#40168 = DIRECTION ( 'NONE',  ( 0.000000000000000000, -0.9999999999976377785, -2.173523156925979975E-06 ) ) ;
#40169 = EDGE_CURVE ( 'NONE', #59693, #9489, #76926, .T. ) ;
#40170 = CARTESIAN_POINT ( 'NONE',  ( -35.57119359481463050, -25.00158670708910336, 2.256160236439224143 ) ) ;
#40171 = DIRECTION ( 'NONE',  ( 1.000000000000000000, 0.000000000000000000, 5.238131417152343399E-15 ) ) ;
#40172 = B_SPLINE_CURVE_WITH_KNOTS ( 'NONE', 3,
 ( #17686, #95805, #65888, #58259 ),
 .UNSPECIFIED., .F., .F.,
 ( 4, 4 ),
 ( 0.000000000000000000, 9.999999999998897304E-05 ),
 .UNSPECIFIED. ) ;
#40173 = EDGE_CURVE ( 'NONE', #5690, #22913, #56894, .T. ) ;
#40174 = CARTESIAN_POINT ( 'NONE',  ( -38.58953762381672448, -23.48783264082477373, -1.443836473390072594 ) ) ;
#40175 = CARTESIAN_POINT ( 'NONE',  ( -83.62924783544907825, -24.34968618360933235, 0.1864209137778810865 ) ) ;
#40176 = CARTESIAN_POINT ( 'NONE',  ( -63.62287095715007723, -24.51387760970723662, 9.387446482453425389 ) ) ;
#40177 = CARTESIAN_POINT ( 'NONE',  ( -49.50841769935764347, -25.26288593538659910, 3.984447754961206734 ) ) ;
#40178 = ORIENTED_EDGE ( 'NONE', *, *, #61732, .T. ) ;
#40179 = CARTESIAN_POINT ( 'NONE',  ( -14.66855384320708033, -14.05595220846724835, -1.500000000000002220 ) ) ;
#40180 = ADVANCED_FACE ( 'NONE', ( #53629 ), #93155, .F. ) ;
#40181 = PLANE ( 'NONE',  #58265 ) ;
#40182 = CARTESIAN_POINT ( 'NONE',  ( -34.50430589304357909, -23.96119346886880663, -0.6495511937831991434 ) ) ;
#40183 = VECTOR ( 'NONE', #44487, 1000.000000000000000 ) ;
#40184 = DIRECTION ( 'NONE',  ( 0.000000000000000000, 0.9999999999976377785, 2.173523156925979975E-06 ) ) ;
#40185 = EDGE_LOOP ( 'NONE', ( #25462, #1038, #64743, #40222 ) ) ;
#40186 = CARTESIAN_POINT ( 'NONE',  ( 13.91401389203221406, -5.965225279485572685, 158.0376437107427137 ) ) ;
#40187 = CARTESIAN_POINT ( 'NONE',  ( 17.50376878386636292, -9.983289808088789741, -1.500000000000002220 ) ) ;
#40188 = CARTESIAN_POINT ( 'NONE',  ( -19.14942259116913092, -8.910193081567555851, 11.49999999999999645 ) ) ;
#40189 = CARTESIAN_POINT ( 'NONE',  ( 5.777647480883832287, 21.37485705712154171, 11.49999999999998934 ) ) ;
#40190 = CARTESIAN_POINT ( 'NONE',  ( -14.32454646668868747, 14.77526322620295929, -1.500000000000002220 ) ) ;
#40191 = CARTESIAN_POINT ( 'NONE',  ( 7.166040305186291093, -5.876774720514420736, 20.81030863372915718 ) ) ;
#40192 = ORIENTED_EDGE ( 'NONE', *, *, #10508, .T. ) ;
#40193 = CARTESIAN_POINT ( 'NONE',  ( 8.160000000000000142, 2.888964624466060727, -0.2527516539682188590 ) ) ;
#40194 = ORIENTED_EDGE ( 'NONE', *, *, #69613, .F. ) ;
#40195 = CARTESIAN_POINT ( 'NONE',  ( -0.3244794670026781014, -9.612687562450236811, -9.000000000000000000 ) ) ;
#40196 = CARTESIAN_POINT ( 'NONE',  ( -61.62287095715004881, -24.66019654487199020, 8.947790411086131712 ) ) ;
#40197 = VERTEX_POINT ( 'NONE', #8932 ) ;
#40198 = EDGE_LOOP ( 'NONE', ( #886, #82126, #38727, #85710 ) ) ;
#40199 = VERTEX_POINT ( 'NONE', #39883 ) ;
#40200 = CARTESIAN_POINT ( 'NONE',  ( -110.7960670365997373, -25.13317731662320398, 2.903215637379843894 ) ) ;
#40201 = CARTESIAN_POINT ( 'NONE',  ( -127.6228709571500275, -23.48786465467242124, 11.44779295918253403 ) ) ;
#40202 = FACE_OUTER_BOUND ( 'NONE', #13250, .T. ) ;
#40203 = CARTESIAN_POINT ( 'NONE',  ( -20.39401028033356766, -3.670942005906183692, -1.500000000000002220 ) ) ;
#40204 = EDGE_CURVE ( 'NONE', #67116, #3935, #86559, .T. ) ;
#40205 = CARTESIAN_POINT ( 'NONE',  ( 21.66353188042378974, 1.267531592894010739, 11.49999999999999645 ) ) ;
#40206 = ORIENTED_EDGE ( 'NONE', *, *, #2614, .T. ) ;
#40207 = DIRECTION ( 'NONE',  ( 0.000000000000000000, -1.000000000000000000, 0.000000000000000000 ) ) ;
#40208 = CARTESIAN_POINT ( 'NONE',  ( -110.5115395816853692, -25.11172157007268524, 2.839984004833783438 ) ) ;
#40209 = CARTESIAN_POINT ( 'NONE',  ( 8.126467401150291536, 20.86698325809501497, 11.49999999999998934 ) ) ;
#40210 = VECTOR ( 'NONE', #21646, 1000.000000000000114 ) ;
#40211 = FACE_OUTER_BOUND ( 'NONE', #14997, .T. ) ;
#40212 = CARTESIAN_POINT ( 'NONE',  ( -101.5228709571500616, -24.50321055353803956, 9.387540953477515160 ) ) ;
#40214 = ORIENTED_EDGE ( 'NONE', *, *, #23354, .F. ) ;
#40213 = EDGE_CURVE ( 'NONE', #76257, #96355, #87237, .T. ) ;
#40215 = CARTESIAN_POINT ( 'NONE',  ( 29.58888977143521970, 4.303425171653743497, 29.06172452911802750 ) ) ;
#40216 = CARTESIAN_POINT ( 'NONE',  ( -52.52287095715006870, -24.64965694238574656, 8.947790433994203596 ) ) ;
#40217 = ORIENTED_EDGE ( 'NONE', *, *, #83658, .F. ) ;
#40218 = ORIENTED_EDGE ( 'NONE', *, *, #56028, .F. ) ;
#40219 = EDGE_CURVE ( 'NONE', #86483, #59266, #20553, .T. ) ;
#40220 = CARTESIAN_POINT ( 'NONE',  ( -87.52287095715006160, -23.48786465467241058, 11.44779295918254292 ) ) ;
#40221 = AXIS2_PLACEMENT_3D ( 'NONE', #70879, #24679, #15075 ) ;
#40222 = ORIENTED_EDGE ( 'NONE', *, *, #80167, .F. ) ;
#40223 = EDGE_CURVE ( 'NONE', #47759, #50913, #53280, .T. ) ;
#40224 = CARTESIAN_POINT ( 'NONE',  ( -107.9228709571500673, -23.47593901973090169, -1.443836447538996648 ) ) ;
#40225 = CARTESIAN_POINT ( 'NONE',  ( -7.948041996521916452, 19.69052605537007850, -1.500000000000002220 ) ) ;
#40226 = ORIENTED_EDGE ( 'NONE', *, *, #55055, .T. ) ;
#40227 = CARTESIAN_POINT ( 'NONE',  ( -107.5228709571500758, -23.47596703998600631, 11.44779298504228038 ) ) ;
#40228 = CARTESIAN_POINT ( 'NONE',  ( 19.23208339725441007, -10.27600428404867827, 11.49999999999998934 ) ) ;
#40229 = CARTESIAN_POINT ( 'NONE',  ( -103.6308638581749051, -23.96169478059713498, 10.65365249895717881 ) ) ;
#40230 = AXIS2_PLACEMENT_3D ( 'NONE', #38538, #15200, #76092 ) ;
#40231 = PLANE ( 'NONE',  #85844 ) ;
#40232 = CARTESIAN_POINT ( 'NONE',  ( -116.6228709571500701, -23.48783264082478794, -1.443836473390058606 ) ) ;
#40233 = CARTESIAN_POINT ( 'NONE',  ( 19.81658424304261246, 9.080307684375437560, -1.500000000000002220 ) ) ;
#40234 = CARTESIAN_POINT ( 'NONE',  ( -1.292025413547811308, -6.376774720514411854, 19.72913074730690752 ) ) ;
#40235 = ORIENTED_EDGE ( 'NONE', *, *, #50357, .T. ) ;
#40236 = DIRECTION ( 'NONE',  ( 0.8246584009594636333, -1.974890369949422146E-15, 0.5656310827093757876 ) ) ;
#40237 = CARTESIAN_POINT ( 'NONE',  ( -48.95684766248727726, -25.12782611306136005, 6.634937016854919101 ) ) ;
#40238 = ORIENTED_EDGE ( 'NONE', *, *, #99246, .T. ) ;
#40239 = ORIENTED_EDGE ( 'NONE', *, *, #1446, .T. ) ;
#40240 = VECTOR ( 'NONE', #5345, 1000.000000000000114 ) ;
#40241 = VERTEX_POINT ( 'NONE', #64760 ) ;
#40242 = FACE_OUTER_BOUND ( 'NONE', #48708, .T. ) ;
#40243 = CARTESIAN_POINT ( 'NONE',  ( -82.63662045704941761, -23.96119346886881019, -0.6495511937831922600 ) ) ;
#40244 = CARTESIAN_POINT ( 'NONE',  ( -14.73150212448299357, 15.28860238833873808, -1.500000000000002220 ) ) ;
#40245 = CARTESIAN_POINT ( 'NONE',  ( -94.62287095715005592, -23.48783264082478794, -1.443836473390063491 ) ) ;
#40246 = CARTESIAN_POINT ( 'NONE',  ( -130.5728709571500588, -24.43626637953623515, 0.1835287498755961699 ) ) ;
#40247 = DIRECTION ( 'NONE',  ( 0.000000000000000000, 0.000000000000000000, -1.000000000000000000 ) ) ;
#40249 = CARTESIAN_POINT ( 'NONE',  ( -99.52287095715006160, -24.64898659630529565, 1.056161002820829697 ) ) ;
#40248 = B_SPLINE_CURVE_WITH_KNOTS ( 'NONE', 3,
 ( #47966, #85511, #78890, #70803, #47464, #40348 ),
 .UNSPECIFIED., .F., .F.,
 ( 4, 2, 4 ),
 ( 0.000000000000000000, 0.001380901958385396351, 0.002761803916770792702 ),
 .UNSPECIFIED. ) ;
#40250 = EDGE_CURVE ( 'NONE', #73517, #99512, #79441, .T. ) ;
#40251 = CARTESIAN_POINT ( 'NONE',  ( -1.608633542659107629, -19.34071428503001755, -1.500000000000002220 ) ) ;
#40252 = CARTESIAN_POINT ( 'NONE',  ( -80.52287095715006160, -23.48786465467241769, 11.44779295918254469 ) ) ;
#40253 = VERTEX_POINT ( 'NONE', #27168 ) ;
#40254 = CARTESIAN_POINT ( 'NONE',  ( -10.96721834449554933, 16.09610527815933168, 11.49999999999999645 ) ) ;
#40255 = CARTESIAN_POINT ( 'NONE',  ( -5.574014511416001127, -5.876774720514413630, 20.24089781925592391 ) ) ;
#40256 = EDGE_CURVE ( 'NONE', #77563, #51201, #39980, .T. ) ;
#40257 = LINE ( 'NONE', #47370, #85211 ) ;
#40258 = ORIENTED_EDGE ( 'NONE', *, *, #90940, .T. ) ;
#40259 = CARTESIAN_POINT ( 'NONE',  ( -93.62287095715004170, -23.72747288104442376, -1.053458166803661999 ) ) ;
#40260 = EDGE_CURVE ( 'NONE', #99388, #64065, #4938, .T. ) ;
#40261 = CARTESIAN_POINT ( 'NONE',  ( -89.51816582126249955, -23.73766607897671221, -1.055555164236434473 ) ) ;
#40262 = EDGE_CURVE ( 'NONE', #35959, #64113, #95176, .T. ) ;
#40263 = FACE_OUTER_BOUND ( 'NONE', #34629, .T. ) ;
#40264 = CARTESIAN_POINT ( 'NONE',  ( -19.61143073682725202, -1.510137823221562092, 11.49999999999998934 ) ) ;
#40265 = B_SPLINE_SURFACE_WITH_KNOTS ( 'NONE', 3, 3, ( 
 ( #42760, #20887, #81307, #42276 ),
 ( #75178, #88927, #51863, #82794 ),
 ( #82299, #5673, #19398, #13275 ),
 ( #36623, #12778, #89917, #11790 ),
 ( #67591, #73206, #74683, #66112 ),
 ( #67101, #34641, #98008, #89420 ),
 ( #73695, #98508, #29006, #59978 ),
 ( #90912, #35639, #27528, #21379 ),
 ( #3694, #4189, #58484, #80811 ),
 ( #20385, #19893, #50866, #81804 ) ),
 .UNSPECIFIED., .F., .F., .F.,
 ( 4, 3, 3, 4 ),
 ( 4, 4 ),
 ( 0.0004766839783813265198, 0.1491231665100168635, 0.2234464077758346323, 0.2977696490416523734 ),
 ( 0.4495482928597397398, 0.4508289012804921891 ),
 .UNSPECIFIED. ) ;
#40266 = VERTEX_POINT ( 'NONE', #3348 ) ;
#40267 = CARTESIAN_POINT ( 'NONE',  ( -8.750087785235610482, 19.73178376063210138, 11.49999999999998934 ) ) ;
#40268 = CARTESIAN_POINT ( 'NONE',  ( -65.52287095715006160, -25.00182538069144655, 7.747789668545101982 ) ) ;
#40269 = CARTESIAN_POINT ( 'NONE',  ( -46.55620429048340014, -23.47593901973091235, -1.443836447539009749 ) ) ;
#40270 = COORDINATED_UNIVERSAL_TIME_OFFSET ( 0, 0, .AHEAD. ) ;
#40271 = CARTESIAN_POINT ( 'NONE',  ( -93.54470913934721921, -24.65952944569305316, 1.056160979905699904 ) ) ;
#40272 = CARTESIAN_POINT ( 'NONE',  ( -105.6228709571500559, -23.84081130438201157, 10.88220057463249013 ) ) ;
#40273 = CARTESIAN_POINT ( 'NONE',  ( -97.59120377316065742, -24.15620529776629155, 10.23563542870660115 ) ) ;
#40274 = CARTESIAN_POINT ( 'NONE',  ( -100.6365410905178379, -25.04435010277327933, 7.557279746904548290 ) ) ;
#40275 = CARTESIAN_POINT ( 'NONE',  ( 5.727631217150810805, -5.876774720514421624, 21.11407618546790133 ) ) ;
#40276 = DIRECTION ( 'NONE',  ( 0.000000000000000000, -0.9999999999976377785, -2.173523156925979128E-06 ) ) ;
#40277 = CARTESIAN_POINT ( 'NONE',  ( -114.5192661640313503, -23.96169478059714564, 10.65365249895717170 ) ) ;
#40279 = EDGE_CURVE ( 'NONE', #50558, #36016, #96182, .T. ) ;
#40278 = CARTESIAN_POINT ( 'NONE',  ( -5.841000908416043913, -19.03464889989004050, -1.500000000000002220 ) ) ;
#40280 = CARTESIAN_POINT ( 'NONE',  ( -75.61136356471840259, -23.48786465467241058, 11.44779295918254824 ) ) ;
#40281 = CARTESIAN_POINT ( 'NONE',  ( 19.41305359857673096, 4.112862643401165919, -1.500000000000002220 ) ) ;
#40282 = EDGE_LOOP ( 'NONE', ( #5312, #48442, #99080, #8548 ) ) ;
#40283 = AXIS2_PLACEMENT_3D ( 'NONE', #88589, #40908, #25174 ) ;
#40284 = CARTESIAN_POINT ( 'NONE',  ( 22.81105451610979173, -1.477225279485574028, -18.46691820600746681 ) ) ;
#40285 = B_SPLINE_CURVE_WITH_KNOTS ( 'NONE', 3,
 ( #19564, #73859, #43909, #27691, #12940, #3863, #19063, #34303, #96204, #49539, #66771, #74840, #72869, #65775, #33798, #26690, #10962, #57649, #41928, #97689, #50038, #88590, #82461 ),
 .UNSPECIFIED., .F., .F.,
 ( 4, 1, 1, 1, 1, 1, 1, 1, 1, 1, 1, 1, 1, 1, 1, 1, 1, 1, 1, 1, 4 ),
 ( 0.000000000000000000, 0.06568119799063895647, 0.1284864641740642022, 0.1881751303280073950, 0.2451061306699852116, 0.2994484245294744551, 0.3508229360093824134, 0.3999416805337764336, 0.4466717436323716650, 0.4912545333734980035, 0.5333763442704358981, 0.5738527549682231887, 0.6125263117194529316, 0.6495971364453292374, 0.6855320415538496137, 0.7201057860682000822, 0.7538376629736500689, 0.8189254160467134280, 0.8804934616501639555, 0.9403113338460573623, 1.000000000000000000 ),
 .UNSPECIFIED. ) ;
#40286 = CARTESIAN_POINT ( 'NONE',  ( -50.40445135320378967, -25.13313949306887451, 7.101635536975466678 ) ) ;
#40287 = DIRECTION ( 'NONE',  ( -1.252131230780251939E-15, -0.000000000000000000, -1.000000000000000000 ) ) ;
#40288 = CARTESIAN_POINT ( 'NONE',  ( -2.856624844580134770, 20.53689577262001364, 11.49999999999999645 ) ) ;
#40289 = DIRECTION ( 'NONE',  ( 0.000000000000000000, 0.000000000000000000, -1.000000000000000000 ) ) ;
#40290 = ADVANCED_FACE ( 'NONE', ( #49515 ), #41907, .F. ) ;
#40291 = CARTESIAN_POINT ( 'NONE',  ( -62.62287095715004881, -29.50248528299804818, 1.056150453629034924 ) ) ;
#40292 = CARTESIAN_POINT ( 'NONE',  ( -13.85039312988123150, 18.09399583546626289, 11.49999999999999645 ) ) ;
#40293 = ORIENTED_EDGE ( 'NONE', *, *, #34333, .F. ) ;
#40294 = CARTESIAN_POINT ( 'NONE',  ( -57.62287095715007013, -23.96127896941631619, -0.6493128931037834839 ) ) ;
#40295 = EDGE_CURVE ( 'NONE', #69965, #96767, #60586, .T. ) ;
#40296 = CARTESIAN_POINT ( 'NONE',  ( -38.52287095715006870, -24.65952944569303895, 1.056160979905691910 ) ) ;
#40297 = VERTEX_POINT ( 'NONE', #57134 ) ;
#40298 = AXIS2_PLACEMENT_3D ( 'NONE', #21557, #45424, #59150 ) ;
#40299 = CARTESIAN_POINT ( 'NONE',  ( 4.066846734877469949, -19.79409818376439389, -1.500000000000002220 ) ) ;
#40300 = LINE ( 'NONE', #71251, #90562 ) ;
#40301 = ADVANCED_FACE ( 'NONE', ( #88069 ), #72848, .F. ) ;
#40302 = CARTESIAN_POINT ( 'NONE',  ( -114.5228709571500190, -24.66019654487200441, 8.947790411086110396 ) ) ;
#40303 = EDGE_CURVE ( 'NONE', #51581, #99250, #9783, .T. ) ;
#40304 = VERTEX_POINT ( 'NONE', #3838 ) ;
#40305 = CARTESIAN_POINT ( 'NONE',  ( -10.30982817980528132, -21.98926139291980064, 11.50200000000000422 ) ) ;
#40306 = CARTESIAN_POINT ( 'NONE',  ( -10.62949710387652758, 20.32685691788189075, -1.500000000000002220 ) ) ;
#40307 = CARTESIAN_POINT ( 'NONE',  ( -10.22992732494356005, 5.749436596009021017, 29.32115093811272288 ) ) ;
#40308 = CARTESIAN_POINT ( 'NONE',  ( 18.82558416981596139, 6.732768832687442639, -1.500000000000002220 ) ) ;
#40309 = CYLINDRICAL_SURFACE ( 'NONE', #86934, 251.4258649670780699 ) ;
#40310 = CARTESIAN_POINT ( 'NONE',  ( 17.09260067683297635, -12.12037977771017871, 11.49999999999999645 ) ) ;
#40311 = CARTESIAN_POINT ( 'NONE',  ( -59.90086283640256681, -25.29841105421058955, 4.072422571224184829 ) ) ;
#40312 = DIRECTION ( 'NONE',  ( 0.8246584009594635223, 0.5656310827093757876, 2.309263891220325920E-14 ) ) ;
#40313 = CARTESIAN_POINT ( 'NONE',  ( -3.902479932019291553, -21.71820464621639246, -1.500000000000002220 ) ) ;
#40314 = CARTESIAN_POINT ( 'NONE',  ( 0.3000000000000007661, 0.000000000000000000, 0.000000000000000000 ) ) ;
#40315 = ORIENTED_EDGE ( 'NONE', *, *, #46226, .F. ) ;
#40316 = CARTESIAN_POINT ( 'NONE',  ( -28.84663072490566194, 5.965225279485572685, 28.73989617533406715 ) ) ;
#40317 = CARTESIAN_POINT ( 'NONE',  ( -49.63711845704647629, -25.18440172823959955, 3.620155769584360694 ) ) ;
#40318 = DIRECTION ( 'NONE',  ( 0.000000000000000000, 1.000000000000000000, 0.000000000000000000 ) ) ;
#40319 = ORIENTED_EDGE ( 'NONE', *, *, #77466, .F. ) ;
#40320 = CARTESIAN_POINT ( 'NONE',  ( -103.6228709571500559, -29.50250786944525672, 11.44777988621623166 ) ) ;
#40321 = B_SPLINE_CURVE_WITH_KNOTS ( 'NONE', 3,
 ( #16415, #83942, #77804, #92547 ),
 .UNSPECIFIED., .F., .F.,
 ( 4, 4 ),
 ( 0.7410291507779422915, 0.7500355820500579362 ),
 .UNSPECIFIED. ) ;
#40322 = VERTEX_POINT ( 'NONE', #63752 ) ;
#40323 = ORIENTED_EDGE ( 'NONE', *, *, #15080, .F. ) ;
#40324 = CARTESIAN_POINT ( 'NONE',  ( -99.62287095715005592, -23.48783264082478794, -1.443836473390061936 ) ) ;
#40325 = CARTESIAN_POINT ( 'NONE',  ( -85.22287095715010707, -23.47593901973090524, -1.443836447538997314 ) ) ;
#40326 = CARTESIAN_POINT ( 'NONE',  ( -36.63503066435342248, -24.34968618360933590, 0.1864209137778783110 ) ) ;
#40327 = CARTESIAN_POINT ( 'NONE',  ( -14.38416181709762043, 14.64695106392160895, -1.500000000000002220 ) ) ;
#40328 = ORIENTED_EDGE ( 'NONE', *, *, #61767, .T. ) ;
#40329 = LINE ( 'NONE', #2281, #96375 ) ;
#40330 = DIRECTION ( 'NONE',  ( 0.000000000000000000, -1.000000000000000000, 0.000000000000000000 ) ) ;
#40331 = CARTESIAN_POINT ( 'NONE',  ( -41.52287095715006870, -23.72773821059536203, 11.05748984161097326 ) ) ;
#40332 = CARTESIAN_POINT ( 'NONE',  ( -21.62769966018443313, 5.350386031573528989, 11.49999999999998934 ) ) ;
#40333 = CARTESIAN_POINT ( 'NONE',  ( -27.25988310792305214, -5.965225279485572685, 30.32664379231667695 ) ) ;
#40335 = EDGE_CURVE ( 'NONE', #35854, #24351, #34285, .T. ) ;
#40334 = CARTESIAN_POINT ( 'NONE',  ( -11.16000000000000014, -9.652339641703484574, -1.621096496867199033 ) ) ;
#40336 = ORIENTED_EDGE ( 'NONE', *, *, #31661, .T. ) ;
#40337 = CARTESIAN_POINT ( 'NONE',  ( -96.62287095715009855, -23.96127896941631619, -0.6493128931037810414 ) ) ;
#40338 = DIRECTION ( 'NONE',  ( -0.000000000000000000, 1.000000000000000000, -0.000000000000000000 ) ) ;
#40339 = CARTESIAN_POINT ( 'NONE',  ( -18.77111393065419875, 9.022841878967760465, -1.500000000000002220 ) ) ;
#40340 = VERTEX_POINT ( 'NONE', #26667 ) ;
#40341 = B_SPLINE_CURVE_WITH_KNOTS ( 'NONE', 3,
 ( #10785, #57975, #66098, #50352, #58963, #97015 ),
 .UNSPECIFIED., .F., .F.,
 ( 4, 2, 4 ),
 ( 1.570755371634131319E-05, 0.001396183895866089054, 0.002776660238015836880 ),
 .UNSPECIFIED. ) ;
#40343 = VERTEX_POINT ( 'NONE', #71847 ) ;
#40342 = CARTESIAN_POINT ( 'NONE',  ( -0.005606649364735081555, -6.376774720514410077, 19.25713806424188235 ) ) ;
#40344 = ORIENTED_EDGE ( 'NONE', *, *, #94816, .T. ) ;
#40345 = CARTESIAN_POINT ( 'NONE',  ( -69.11592688286732766, -25.25935203297461484, 6.884840302703743475 ) ) ;
#40346 = CARTESIAN_POINT ( 'NONE',  ( -3.838044578953509145, 20.63102806057878880, -1.500000000000002220 ) ) ;
#40347 = VERTEX_POINT ( 'NONE', #50017 ) ;
#40348 = CARTESIAN_POINT ( 'NONE',  ( -118.5228709571500758, -23.47596703998600631, 11.44779298504227860 ) ) ;
#40349 = AXIS2_PLACEMENT_3D ( 'NONE', #37809, #61167, #99681 ) ;
#40350 = CARTESIAN_POINT ( 'NONE',  ( 6.499999999999992895, -5.174132726397561390E-16, 4.499999999999999112 ) ) ;
#40351 = CARTESIAN_POINT ( 'NONE',  ( 9.464509667904351886, -3.316774720514128028, -27.03659963365196717 ) ) ;
#40352 = CIRCLE ( 'NONE', #3063, 0.8160000000000007248 ) ;
#40353 = CARTESIAN_POINT ( 'NONE',  ( -101.7635726060833434, -25.03152285269965915, 6.809096594898544907 ) ) ;
#40354 = CARTESIAN_POINT ( 'NONE',  ( -59.58754539228643665, -24.34968618360933235, 0.1864209137778795600 ) ) ;
#40355 = CARTESIAN_POINT ( 'NONE',  ( -108.9857487368351627, -25.30480944508042640, 4.484590831594999827 ) ) ;
#40356 = DIRECTION ( 'NONE',  ( -3.773278334453079030E-23, 0.9999999999976377785, 2.173523156925979128E-06 ) ) ;
#40358 = EDGE_LOOP ( 'NONE', ( #66506, #32979, #35070, #64486 ) ) ;
#40357 = CARTESIAN_POINT ( 'NONE',  ( -22.22723998432330106, 0.1330083165726352878, 11.49999999999999645 ) ) ;
#40359 = CARTESIAN_POINT ( 'NONE',  ( 17.51792015816173986, 5.965225279485572685, 29.01255224319336889 ) ) ;
#40360 = LINE ( 'NONE', #26132, #60246 ) ;
#40361 = ORIENTED_EDGE ( 'NONE', *, *, #67711, .T. ) ;
#40362 = CARTESIAN_POINT ( 'NONE',  ( -2.225104987405961854, -22.55768739424384606, 11.49999999999998934 ) ) ;
#40363 = AXIS2_PLACEMENT_3D ( 'NONE', #54561, #76872, #7879 ) ;
#40365 = ORIENTED_EDGE ( 'NONE', *, *, #99608, .T. ) ;
#40364 = CARTESIAN_POINT ( 'NONE',  ( -5.912814555383966386, -6.376774720514418959, 20.28973052848695602 ) ) ;
#40366 = ORIENTED_EDGE ( 'NONE', *, *, #22221, .T. ) ;
#40367 = VECTOR ( 'NONE', #5211, 1000.000000000000114 ) ;
#40368 = CARTESIAN_POINT ( 'NONE',  ( 7.160000000000000142, -5.907068460905240411E-16, 5.788828319098143105 ) ) ;
#40369 = EDGE_CURVE ( 'NONE', #52307, #21700, #78, .T. ) ;
#40370 = CARTESIAN_POINT ( 'NONE',  ( 9.931738293602487389, -17.53800358597336384, 11.49999999999998934 ) ) ;
#40371 = CARTESIAN_POINT ( 'NONE',  ( -32.62287095715007013, -24.51283580621364777, 0.6167428607019671549 ) ) ;
#40372 = VERTEX_POINT ( 'NONE', #33266 ) ;
#40373 = CARTESIAN_POINT ( 'NONE',  ( -58.55620429048338593, -23.48783264082478439, -1.443836473390070596 ) ) ;
#40374 = CARTESIAN_POINT ( 'NONE',  ( 22.37589550080693712, 1.095942408959037273, -1.500000000000002220 ) ) ;
#40375 = ORIENTED_EDGE ( 'NONE', *, *, #60326, .T. ) ;
#40376 = VERTEX_POINT ( 'NONE', #58618 ) ;
#40377 = PLANE ( 'NONE',  #19059 ) ;
#40378 = CARTESIAN_POINT ( 'NONE',  ( -69.52287095715006160, -24.64965694238407323, 8.947790433994200043 ) ) ;
#40379 = DIRECTION ( 'NONE',  ( 3.773278334444166432E-23, -1.000000000000000000, 0.000000000000000000 ) ) ;
#40380 = EDGE_CURVE ( 'NONE', #57758, #13348, #69084, .T. ) ;
#40381 = ADVANCED_FACE ( 'NONE', ( #43397 ), #36279, .F. ) ;
#40382 = LINE ( 'NONE', #3829, #35200 ) ;
#40383 = EDGE_CURVE ( 'NONE', #41593, #95277, #35779, .T. ) ;
#40384 = CARTESIAN_POINT ( 'NONE',  ( -130.5728709571500588, -23.47593901973090524, -1.443836447538995760 ) ) ;
#40385 = CARTESIAN_POINT ( 'NONE',  ( -19.37596289572233488, 2.755671585415585767, -1.500000000000002220 ) ) ;
#40386 = DIRECTION ( 'NONE',  ( -1.000000000000000000, -3.491481338843133355E-15, -2.352173255807796056E-16 ) ) ;
#40388 = EDGE_CURVE ( 'NONE', #87273, #20975, #28659, .T. ) ;
#40387 = VERTEX_POINT ( 'NONE', #89561 ) ;
#40389 = CARTESIAN_POINT ( 'NONE',  ( 20.90071823198991297, 5.034746273075951351, -1.500000000000002220 ) ) ;
#40390 = CARTESIAN_POINT ( 'NONE',  ( -36.52287095715006870, -23.48783264082477018, -1.443836473390097019 ) ) ;
#40391 = CARTESIAN_POINT ( 'NONE',  ( 33.96422015159436114, -5.965225279485572685, -7.233236000911337449 ) ) ;
#40392 = DIRECTION ( 'NONE',  ( -1.104558621438292892E-14, 0.000000000000000000, -1.000000000000000000 ) ) ;
#40393 = DIRECTION ( 'NONE',  ( 0.000000000000000000, -2.173523156925979552E-06, 0.9999999999976378895 ) ) ;
#40394 = CARTESIAN_POINT ( 'NONE',  ( -22.88579126497628025, -1.409509213828211927, -1.500000000000002220 ) ) ;
#40395 = VECTOR ( 'NONE', #46508, 1000.000000000000000 ) ;
#40396 = SECURITY_CLASSIFICATION_LEVEL ( 'unclassified' ) ;
#40397 = DIRECTION ( 'NONE',  ( 0.7071067811865476838, 0.000000000000000000, -0.7071067811865474617 ) ) ;
#40398 = CARTESIAN_POINT ( 'NONE',  ( -42.52287095715005449, -24.34917612407031839, 0.1852690917477345378 ) ) ;
#40399 = CARTESIAN_POINT ( 'NONE',  ( -18.86779840422491716, -6.689013621249945807, 11.49999999999999645 ) ) ;
#40400 = CARTESIAN_POINT ( 'NONE',  ( -78.94637683104262749, -25.31594602001839078, 5.821637659726635938 ) ) ;
#40401 = DIRECTION ( 'NONE',  ( -3.773278334453079618E-23, 0.9999999999976377785, 2.173523156925979975E-06 ) ) ;
#40402 = CARTESIAN_POINT ( 'NONE',  ( 4.821763668436347849, -5.876774720514406525, 18.93074869776452829 ) ) ;
#40403 = CARTESIAN_POINT ( 'NONE',  ( -39.62287095715005592, -23.47596703998600276, 11.44779298504227505 ) ) ;
#40404 = LINE ( 'NONE', #39397, #83426 ) ;
#40405 = EDGE_CURVE ( 'NONE', #76194, #99483, #34648, .T. ) ;
#40406 = CARTESIAN_POINT ( 'NONE',  ( 1.937016913031804455, -21.67664703184077268, 11.49999999999998934 ) ) ;
#40407 = LINE ( 'NONE', #1848, #67461 ) ;
#40408 = CARTESIAN_POINT ( 'NONE',  ( 16.09843989366402539, -11.26760994518913428, -1.500000000000002220 ) ) ;
#40409 = DIRECTION ( 'NONE',  ( -0.000000000000000000, 2.173523156925979552E-06, -0.9999999999976378895 ) ) ;
#40410 = EDGE_CURVE ( 'NONE', #623, #27902, #20531, .T. ) ;
#40411 = PLANE ( 'NONE',  #45094 ) ;
#40412 = CALENDAR_DATE ( 2026, 9, 10 ) ;
#40413 = CARTESIAN_POINT ( 'NONE',  ( -91.63415563865659408, -23.96169478059713498, 10.65365249895717881 ) ) ;
#40414 = DIRECTION ( 'NONE',  ( 0.000000000000000000, 0.000000000000000000, 1.000000000000000000 ) ) ;
#40415 = CARTESIAN_POINT ( 'NONE',  ( -12.99546161633903552, -15.93940442571882876, 11.49999999999999645 ) ) ;
#40416 = CARTESIAN_POINT ( 'NONE',  ( 4.547994309883463870, -6.376774720514422512, 20.87593061325451416 ) ) ;
#40417 = EDGE_CURVE ( 'NONE', #48044, #98355, #19541, .T. ) ;
#40418 = CARTESIAN_POINT ( 'NONE',  ( -120.6238000549733727, -24.92564183028979485, 1.928384488918253092 ) ) ;
#40419 = CARTESIAN_POINT ( 'NONE',  ( 19.13181028273733375, 12.02906595412573232, 11.49999999999999645 ) ) ;
#40420 = ORIENTED_EDGE ( 'NONE', *, *, #15180, .T. ) ;
#40421 = CARTESIAN_POINT ( 'NONE',  ( -100.6258216950799778, -25.26387453630955449, 4.735305889788031131 ) ) ;
#40422 = PLANE ( 'NONE',  #31525 ) ;
#40423 = CARTESIAN_POINT ( 'NONE',  ( -97.59120735429435456, -24.15543982623907837, -0.2315651400026600415 ) ) ;
#40424 = CARTESIAN_POINT ( 'NONE',  ( -72.62287095715004170, -23.72773821059535848, 11.05748984161097681 ) ) ;
#40425 = VECTOR ( 'NONE', #27206, 1000.000000000000000 ) ;
#40426 = CARTESIAN_POINT ( 'NONE',  ( -25.68888630310901178, -24.93063242766984544, 6.447529969727213484 ) ) ;
#40427 = EDGE_CURVE ( 'NONE', #42580, #86491, #30256, .T. ) ;
#40428 = PLANE ( 'NONE',  #80361 ) ;
#40429 = VECTOR ( 'NONE', #25986, 1000.000000000000000 ) ;
#40430 = EDGE_CURVE ( 'NONE', #92347, #13191, #91051, .T. ) ;
#40431 = ORIENTED_EDGE ( 'NONE', *, *, #52164, .T. ) ;
#40432 = CARTESIAN_POINT ( 'NONE',  ( -80.31352994281894553, -25.26749876826690056, 4.969670918755285882 ) ) ;
#40433 = CARTESIAN_POINT ( 'NONE',  ( 4.459850365305920938, 22.40387240153798487, 11.49999999999998934 ) ) ;
#40434 = CARTESIAN_POINT ( 'NONE',  ( -110.5228709571500616, -24.99156044556120548, 7.747789690856173195 ) ) ;
#40435 = AXIS2_PLACEMENT_3D ( 'NONE', #9218, #71634, #48808 ) ;
#40436 = CARTESIAN_POINT ( 'NONE',  ( -72.58953762381671027, -24.66019654487198665, 8.947790411086131712 ) ) ;
#40437 = CARTESIAN_POINT ( 'NONE',  ( -82.62631727302549223, -24.51419770103156281, 9.386484678747187615 ) ) ;
#40438 = CARTESIAN_POINT ( 'NONE',  ( -15.54266751046811557, -16.22994250641250957, 11.49999999999999645 ) ) ;
#40439 = ORIENTED_EDGE ( 'NONE', *, *, #25531, .T. ) ;
#40440 = AXIS2_PLACEMENT_3D ( 'NONE', #85846, #92943, #93443 ) ;
#40441 = CARTESIAN_POINT ( 'NONE',  ( 8.160000000000000142, 0.000000000000000000, 0.000000000000000000 ) ) ;
#40442 = CARTESIAN_POINT ( 'NONE',  ( -21.18249553426131015, -5.656070447573528170, -1.500000000000002220 ) ) ;
#40443 = CARTESIAN_POINT ( 'NONE',  ( 32.29806486058159010, 4.575840390334028562, -4.131869215359018632 ) ) ;
#40445 = DIRECTION ( 'NONE',  ( 0.000000000000000000, 1.000000000000000000, 0.000000000000000000 ) ) ;
#40444 = AXIS2_PLACEMENT_3D ( 'NONE', #41757, #72701, #3197 ) ;
#40446 = CARTESIAN_POINT ( 'NONE',  ( -24.90875734969025501, -3.316774720514426456, 27.45402280011862572 ) ) ;
#40447 = VERTEX_POINT ( 'NONE', #6317 ) ;
#40448 = CARTESIAN_POINT ( 'NONE',  ( 22.02124265030973760, -4.543225279485573864, 16.20402280011862217 ) ) ;
#40449 = CARTESIAN_POINT ( 'NONE',  ( -9.940598223437573822, -6.376774720514426953, 18.21871304725684837 ) ) ;
#40450 = VERTEX_POINT ( 'NONE', #52501 ) ;
#40451 = CARTESIAN_POINT ( 'NONE',  ( -20.44062828730913139, -1.133067592104922694, 11.49999999999998934 ) ) ;
#40452 = EDGE_LOOP ( 'NONE', ( #64155, #97961, #36442, #99264 ) ) ;
#40453 = EDGE_LOOP ( 'NONE', ( #91618, #21712, #32615, #11414 ) ) ;
#40454 = ORIENTED_EDGE ( 'NONE', *, *, #30636, .T. ) ;
#40455 = ORIENTED_EDGE ( 'NONE', *, *, #69335, .F. ) ;
#40456 = B_SPLINE_CURVE_WITH_KNOTS ( 'NONE', 3,
 ( #20368, #4171, #51343, #43731 ),
 .UNSPECIFIED., .F., .F.,
 ( 4, 4 ),
 ( 1.387778780781445521E-17, 9.999999999997510880E-05 ),
 .UNSPECIFIED. ) ;
#40457 = CARTESIAN_POINT ( 'NONE',  ( 21.72910700495702230, 7.846448622349001312, -1.500000000000002220 ) ) ;
#40458 = CARTESIAN_POINT ( 'NONE',  ( -112.5228709571500616, -24.66019654487200441, 8.947790411086108620 ) ) ;
#40459 = CARTESIAN_POINT ( 'NONE',  ( -6.692510123977180925, 19.25193956699996178, -1.500000000000002220 ) ) ;
#40460 = ORIENTED_EDGE ( 'NONE', *, *, #64392, .F. ) ;
#40461 = CARTESIAN_POINT ( 'NONE',  ( 29.73612274945269718, 5.099749465620300626, 27.18845636319765191 ) ) ;
#40462 = DIRECTION ( 'NONE',  ( 0.000000000000000000, 0.000000000000000000, -1.000000000000000000 ) ) ;
#40463 = CARTESIAN_POINT ( 'NONE',  ( -116.6228709571500559, -29.50248528299804818, 1.056150453629045360 ) ) ;
#40464 = CARTESIAN_POINT ( 'NONE',  ( -70.57802201159600486, -25.00158670708910691, 2.256160236439221034 ) ) ;
#40466 = ORIENTED_EDGE ( 'NONE', *, *, #99934, .F. ) ;
#40465 = CARTESIAN_POINT ( 'NONE',  ( -5.607854029519995898, -20.77141283803394955, 11.49999999999999645 ) ) ;
#40467 = CARTESIAN_POINT ( 'NONE',  ( -75.58921274596343665, -24.52300882791530512, 0.6510814631126415897 ) ) ;
#40468 = CARTESIAN_POINT ( 'NONE',  ( -48.55620429048338593, -24.64898659630528144, 1.056161002820819927 ) ) ;
#40469 = VERTEX_POINT ( 'NONE', #37272 ) ;
#40470 = CARTESIAN_POINT ( 'NONE',  ( 3.485566553294195291, 20.44204155273375889, 11.49999999999998934 ) ) ;
#40471 = ORIENTED_EDGE ( 'NONE', *, *, #68820, .T. ) ;
#40473 = ORIENTED_EDGE ( 'NONE', *, *, #72382, .T. ) ;
#40472 = CARTESIAN_POINT ( 'NONE',  ( -125.5887523808240047, -25.00158670708911046, 2.256160236439218369 ) ) ;
#40474 = DIRECTION ( 'NONE',  ( 0.000000000000000000, 0.000000000000000000, -1.000000000000000000 ) ) ;
#40475 = CARTESIAN_POINT ( 'NONE',  ( -53.52287095715004739, -24.34917612406836440, 0.1852690917426514372 ) ) ;
#40476 = EDGE_LOOP ( 'NONE', ( #18672, #4509, #77188, #59034 ) ) ;
#40477 = ORIENTED_EDGE ( 'NONE', *, *, #84910, .T. ) ;
#40478 = CARTESIAN_POINT ( 'NONE',  ( -40.52287095715006160, -23.85196035786899671, -0.8779234886475247857 ) ) ;
#40479 = FACE_OUTER_BOUND ( 'NONE', #28985, .T. ) ;
#40480 = DIRECTION ( 'NONE',  ( 3.773278334444166432E-23, -1.000000000000000000, 0.000000000000000000 ) ) ;
#40482 = VERTEX_POINT ( 'NONE', #28165 ) ;
#40481 = CARTESIAN_POINT ( 'NONE',  ( 21.39010012190943755, 5.354582491813655309, 11.49999999999999645 ) ) ;
#40483 = CARTESIAN_POINT ( 'NONE',  ( -103.6332059738791003, -23.73766607897670156, -1.055555164236454901 ) ) ;
#40484 = CARTESIAN_POINT ( 'NONE',  ( -10.21242994381667657, -20.12718729479640700, -1.500000000000002220 ) ) ;
#40485 = CARTESIAN_POINT ( 'NONE',  ( 20.48634023128459347, 4.603634630958829632, -1.500000000000002220 ) ) ;
#40486 = B_SPLINE_CURVE_WITH_KNOTS ( 'NONE', 3,
 ( #59105, #96647, #51483, #35265, #96159, #12404 ),
 .UNSPECIFIED., .F., .F.,
 ( 4, 2, 4 ),
 ( 0.000000000000000000, 0.001380901958385393966, 0.002761803916770787931 ),
 .UNSPECIFIED. ) ;
#40487 = B_SPLINE_CURVE_WITH_KNOTS ( 'NONE', 3,
 ( #87441, #50392, #96060, #89445 ),
 .UNSPECIFIED., .F., .F.,
 ( 4, 4 ),
 ( 0.7010005673463182152, 0.7100069986184336379 ),
 .UNSPECIFIED. ) ;
#40489 = ORIENTED_EDGE ( 'NONE', *, *, #66521, .F. ) ;
#40488 = CARTESIAN_POINT ( 'NONE',  ( -62.52287095715006160, -24.64898659630367561, 1.056161002820822592 ) ) ;
#40490 = ORIENTED_EDGE ( 'NONE', *, *, #26053, .F. ) ;
#40491 = CARTESIAN_POINT ( 'NONE',  ( 33.10875634548599322, 5.965225279485572685, -11.42349945801155719 ) ) ;
#40492 = VECTOR ( 'NONE', #42019, 1000.000000000000000 ) ;
#40493 = CARTESIAN_POINT ( 'NONE',  ( -28.98875734969026396, -0.3587747205144262708, 7.870022800118625206 ) ) ;
#40494 = ORIENTED_EDGE ( 'NONE', *, *, #69839, .F. ) ;
#40495 = CARTESIAN_POINT ( 'NONE',  ( 8.100108036306837178, -19.54698220168213041, -1.500000000000002220 ) ) ;
#40496 = DIRECTION ( 'NONE',  ( -0.000000000000000000, -1.000000000000000000, -0.000000000000000000 ) ) ;
#40497 = EDGE_CURVE ( 'NONE', #9106, #48044, #16775, .T. ) ;
#40498 = CARTESIAN_POINT ( 'NONE',  ( -51.20402663469029392, -25.26041081037891445, 7.397223726173897340 ) ) ;
#40500 = CARTESIAN_POINT ( 'NONE',  ( -75.62287095715008434, -24.14321612903114556, -0.2833117244521566325 ) ) ;
#40499 = AXIS2_PLACEMENT_3D ( 'NONE', #64692, #26094, #86492 ) ;
#40501 = CARTESIAN_POINT ( 'NONE',  ( -125.6228709571500559, -24.99132157543083821, 2.256160258750667502 ) ) ;
#40502 = CARTESIAN_POINT ( 'NONE',  ( -47.62287095715004170, -23.72773821059535493, 11.05748984161097503 ) ) ;
#40503 = CARTESIAN_POINT ( 'NONE',  ( 22.17158117043571863, -1.905908075979310334, -1.500000000000002220 ) ) ;
#40504 = EDGE_CURVE ( 'NONE', #99512, #25851, #95499, .T. ) ;
#40505 = CARTESIAN_POINT ( 'NONE',  ( -49.87826110250815503, -25.13941482721087084, 7.497148031602994145 ) ) ;
#40506 = ADVANCED_FACE ( 'NONE', ( #74335 ), #5815, .T. ) ;
#40507 = ORIENTED_EDGE ( 'NONE', *, *, #44976, .F. ) ;
#40508 = DIRECTION ( 'NONE',  ( 1.000000000000000000, 0.000000000000000000, -0.000000000000000000 ) ) ;
#40509 = CARTESIAN_POINT ( 'NONE',  ( -37.62900166493126619, -24.51314013834315375, 0.6176544820404124003 ) ) ;
#40510 = DIRECTION ( 'NONE',  ( -1.097118550003962868E-17, -2.020641003924594591E-17, -1.000000000000000000 ) ) ;
#40511 = AXIS2_PLACEMENT_3D ( 'NONE', #68690, #22484, #29117 ) ;
#40512 = ADVANCED_FACE ( 'NONE', ( #67738 ), #22421, .T. ) ;
#40513 = ADVANCED_FACE ( 'NONE', ( #54999 ), #100129, .T. ) ;
#40514 = DIRECTION ( 'NONE',  ( -0.000000000000000000, -0.000000000000000000, -1.000000000000000000 ) ) ;
#40515 = CARTESIAN_POINT ( 'NONE',  ( 6.600000000000001421, 0.000000000000000000, 0.000000000000000000 ) ) ;
#40516 = AXIS2_PLACEMENT_3D ( 'NONE', #88996, #18972, #19468 ) ;
#40517 = CARTESIAN_POINT ( 'NONE',  ( 18.70946937610417038, -5.484834493922766896, -1.500000000000002220 ) ) ;
#40518 = CIRCLE ( 'NONE', #1617, 28.45799999999999486 ) ;
#40519 = CARTESIAN_POINT ( 'NONE',  ( 14.52366289275476419, -15.72616519631134580, 11.49999999999998934 ) ) ;
#40520 = LINE ( 'NONE', #26280, #32040 ) ;
#40521 = FACE_OUTER_BOUND ( 'NONE', #87916, .T. ) ;
#40522 = CARTESIAN_POINT ( 'NONE',  ( -100.6228709571500701, -24.83620972994592790, 8.398175272781362111 ) ) ;
#40523 = CARTESIAN_POINT ( 'NONE',  ( 29.70220533433691301, -3.316774720514426456, 28.20564067601639735 ) ) ;
#40524 = CARTESIAN_POINT ( 'NONE',  ( -22.07869367785253090, -5.390224856484156390, -1.500000000000002220 ) ) ;
#40525 = AXIS2_PLACEMENT_3D ( 'NONE', #99380, #15147, #30877 ) ;
#40526 = CARTESIAN_POINT ( 'NONE',  ( -98.59116248804129157, -24.15543982623907837, -0.2315651400026625395 ) ) ;
#40527 = FACE_OUTER_BOUND ( 'NONE', #29292, .T. ) ;
#40528 = CARTESIAN_POINT ( 'NONE',  ( 1.822157996128044299, -19.77364354024053839, 11.49999999999999645 ) ) ;
#40529 = DIRECTION ( 'NONE',  ( -1.000000000000000000, 0.000000000000000000, 0.000000000000000000 ) ) ;
#40530 = B_SPLINE_CURVE_WITH_KNOTS ( 'NONE', 3,
 ( #39626, #1074, #64001, #48256, #53864, #39122, #54866, #15279, #87811, #89309, #35530, #65002, #73587, #74088 ),
 .UNSPECIFIED., .F., .F.,
 ( 4, 2, 2, 2, 2, 2, 4 ),
 ( 0.000000000000000000, 0.0002088823906780594799, 0.0004177647813561189598, 0.0008355295627122259934, 0.001253294344068333135, 0.001462176734746396247, 0.001671059125424459143 ),
 .UNSPECIFIED. ) ;
#40531 = CARTESIAN_POINT ( 'NONE',  ( -88.55620429048339304, -24.64898659630529210, 1.056161002820829919 ) ) ;
#40532 = DIRECTION ( 'NONE',  ( 1.000000000000000000, 0.000000000000000000, 0.000000000000000000 ) ) ;
#40533 = ORIENTED_EDGE ( 'NONE', *, *, #99252, .T. ) ;
#40534 = CARTESIAN_POINT ( 'NONE',  ( -49.31756476722683402, -25.22308043492110485, 6.418058605870250233 ) ) ;
#40535 = CARTESIAN_POINT ( 'NONE',  ( -6.275748223059703257, -6.376774720514411854, 19.59984006504824805 ) ) ;
#40536 = CARTESIAN_POINT ( 'NONE',  ( -75.62287095715004170, -24.99132157543084176, 2.256160258750667502 ) ) ;
#40537 = CARTESIAN_POINT ( 'NONE',  ( -17.53059066697263546, 12.75712217820542627, -1.500000000000002220 ) ) ;
#40538 = CARTESIAN_POINT ( 'NONE',  ( -56.52206863758583921, -23.48786465467241058, 11.44779295918254647 ) ) ;
#40539 = CARTESIAN_POINT ( 'NONE',  ( 10.22484414329051994, 16.58839404647166660, -1.500000000000002220 ) ) ;
#40540 = DIRECTION ( 'NONE',  ( 1.000000000000000000, 3.773278334444167608E-23, 8.201307833595939069E-29 ) ) ;
#40541 = EDGE_CURVE ( 'NONE', #49066, #53606, #50873, .T. ) ;
#40542 = VERTEX_POINT ( 'NONE', #77800 ) ;
#40543 = CARTESIAN_POINT ( 'NONE',  ( -10.90597124047809530, 17.21661415904998904, 11.49999999999999645 ) ) ;
#40544 = CARTESIAN_POINT ( 'NONE',  ( -110.5228709571500616, -23.48783264082477018, -1.443836473390086583 ) ) ;
#40545 = CARTESIAN_POINT ( 'NONE',  ( -41.55620429048340014, -23.47593901973091235, -1.443836447539011525 ) ) ;
#40546 = ORIENTED_EDGE ( 'NONE', *, *, #45547, .T. ) ;
#40547 = CARTESIAN_POINT ( 'NONE',  ( -41.46036410897617941, -25.27941668849123147, 4.063043375333840856 ) ) ;
#40548 = CARTESIAN_POINT ( 'NONE',  ( 33.47959399259596580, 3.475369878553063341, -12.33463419434873032 ) ) ;
#40549 = CARTESIAN_POINT ( 'NONE',  ( -34.52287095715006160, -24.65952944569303895, 1.056160979905690134 ) ) ;
#40550 = CARTESIAN_POINT ( 'NONE',  ( -49.32129151558435609, -25.25138820444266230, 5.877611043602244401 ) ) ;
#40551 = CARTESIAN_POINT ( 'NONE',  ( -86.52287095715006160, -24.65952944569304606, 1.056160979905700570 ) ) ;
#40552 = CARTESIAN_POINT ( 'NONE',  ( 18.22116949570664701, -8.484823103377051368, 11.49999999999998934 ) ) ;
#40553 = DIRECTION ( 'NONE',  ( 0.000000000000000000, 0.000000000000000000, -1.000000000000000000 ) ) ;
#40554 = EDGE_LOOP ( 'NONE', ( #7234, #74612, #94034, #63349 ) ) ;
#40555 = CARTESIAN_POINT ( 'NONE',  ( -102.5228709571500758, -29.50248528299804818, 1.056150453629042030 ) ) ;
#40556 = EDGE_CURVE ( 'NONE', #52078, #66467, #8817, .T. ) ;
#40557 = CARTESIAN_POINT ( 'NONE',  ( -0.4961427919413599064, 22.93664481792237453, 11.49999999999999645 ) ) ;
#40558 = CARTESIAN_POINT ( 'NONE',  ( 19.62911079104473444, -11.51699945595908758, 11.49999999999998934 ) ) ;
#40559 = ORIENTED_EDGE ( 'NONE', *, *, #40410, .T. ) ;
#40560 = CARTESIAN_POINT ( 'NONE',  ( -78.62287095715005592, -23.47596703998600631, 11.44779298504227860 ) ) ;
#40561 = DIRECTION ( 'NONE',  ( -3.773278334453079030E-23, 0.9999999999976377785, 2.173523156925979128E-06 ) ) ;
#40562 = CARTESIAN_POINT ( 'NONE',  ( -90.54438304270964011, -24.73486907724917927, 1.287355809206966573 ) ) ;
#40563 = CARTESIAN_POINT ( 'NONE',  ( -30.57287095715007652, -25.15787655275395807, 6.970815268604743764 ) ) ;
#40565 = EDGE_CURVE ( 'NONE', #30069, #20120, #83938, .T. ) ;
#40564 = AXIS2_PLACEMENT_3D ( 'NONE', #87370, #85874, #55434 ) ;
#40566 = CARTESIAN_POINT ( 'NONE',  ( -69.64549865058073408, -23.73791477778911840, 11.05961554403170766 ) ) ;
#40567 = CARTESIAN_POINT ( 'NONE',  ( -53.01255352321339842, 4.132774720514426292, 35.59556822165056644 ) ) ;
#40568 = CARTESIAN_POINT ( 'NONE',  ( -122.5545149021958906, -24.34968618360934300, 0.1864209137778895797 ) ) ;
#40569 = CARTESIAN_POINT ( 'NONE',  ( -81.62287095715005592, -23.47593901973091235, -1.443836447539004642 ) ) ;
#40570 = ORIENTED_EDGE ( 'NONE', *, *, #20905, .F. ) ;
#40571 = CARTESIAN_POINT ( 'NONE',  ( -5.191926799570463658, 19.71030214607805675, 11.49999999999998934 ) ) ;
#40572 = VERTEX_POINT ( 'NONE', #32142 ) ;
#40573 = EDGE_LOOP ( 'NONE', ( #82117, #28997, #68433, #13964 ) ) ;
#40574 = CARTESIAN_POINT ( 'NONE',  ( -15.77545706029219730, -16.76941864122914083, -1.500000000000002220 ) ) ;
#40575 = CARTESIAN_POINT ( 'NONE',  ( -6.905879715866854340, -5.876774720514411854, 19.48240003225459560 ) ) ;
#40576 = ORIENTED_EDGE ( 'NONE', *, *, #34884, .F. ) ;
#40577 = CARTESIAN_POINT ( 'NONE',  ( -108.5571773441287888, -23.73791477778912196, 11.05961554403169878 ) ) ;
#40578 = CARTESIAN_POINT ( 'NONE',  ( -99.52287095715006160, -24.64965694238407323, 8.947790433994194714 ) ) ;
#40580 = CARTESIAN_POINT ( 'NONE',  ( -95.55787989783573266, -23.85016227208581441, -0.8807180028928280890 ) ) ;
#40579 = CIRCLE ( 'NONE', #63260, 251.4258649670780699 ) ;
#40581 = DIRECTION ( 'NONE',  ( 0.000000000000000000, 0.000000000000000000, 1.000000000000000000 ) ) ;
#40583 = EDGE_LOOP ( 'NONE', ( #15324, #31367, #58809, #82845 ) ) ;
#40582 = CARTESIAN_POINT ( 'NONE',  ( -1.376967878889499897, 21.29249089469206524, 11.49999999999999645 ) ) ;
#40584 = VECTOR ( 'NONE', #36945, 1000.000000000000000 ) ;
#40585 = VERTEX_POINT ( 'NONE', #91546 ) ;
#40586 = CARTESIAN_POINT ( 'NONE',  ( -19.03210976516136554, 11.49075778266564107, 11.49999999999998934 ) ) ;
#40587 = CARTESIAN_POINT ( 'NONE',  ( 20.28538307770854487, 3.844468116359331944, 11.49999999999998934 ) ) ;
#40588 = VECTOR ( 'NONE', #84551, 1000.000000000000227 ) ;
#40589 = VERTEX_POINT ( 'NONE', #54002 ) ;
#40590 = CARTESIAN_POINT ( 'NONE',  ( -41.46611000704998418, -25.28830591450888932, 4.188173661249235735 ) ) ;
#40591 = DIRECTION ( 'NONE',  ( 0.000000000000000000, 0.000000000000000000, -1.000000000000000000 ) ) ;
#40592 = AXIS2_PLACEMENT_3D ( 'NONE', #45063, #14588, #21692 ) ;
#40593 = ORIENTED_EDGE ( 'NONE', *, *, #3104, .T. ) ;
#40594 = DIRECTION ( 'NONE',  ( -3.773278334453079618E-23, 0.9999999999976377785, 2.173523156925979975E-06 ) ) ;
#40595 = ORIENTED_EDGE ( 'NONE', *, *, #10468, .F. ) ;
#40596 = LINE ( 'NONE', #54323, #94965 ) ;
#40597 = DIRECTION ( 'NONE',  ( 0.7863974287229266169, 0.000000000000000000, -0.6177208787939496570 ) ) ;
#40598 = CARTESIAN_POINT ( 'NONE',  ( -18.00717387566553995, 10.56535500573724740, -1.500000000000002220 ) ) ;
#40599 = CARTESIAN_POINT ( 'NONE',  ( 3.337383349182757364, -21.60657791699550856, 11.49999999999999645 ) ) ;
#40600 = PLANE ( 'NONE',  #60954 ) ;
#40601 = CARTESIAN_POINT ( 'NONE',  ( -65.05438548721848235, -6.376774720514426953, 30.51402280011862089 ) ) ;
#40602 = CARTESIAN_POINT ( 'NONE',  ( 9.993301969596378953, 20.15287186522775542, 11.49999999999998934 ) ) ;
#40603 = CARTESIAN_POINT ( 'NONE',  ( -118.5893566070612621, -24.35071581493543746, 9.817618358456019934 ) ) ;
#40604 = CARTESIAN_POINT ( 'NONE',  ( -72.52287095715007581, -23.48786465467241058, 11.44779295918254647 ) ) ;
#40605 = DIRECTION ( 'NONE',  ( 1.000000000000000000, -0.000000000000000000, -0.000000000000000000 ) ) ;
#40606 = VERTEX_POINT ( 'NONE', #68722 ) ;
#40607 = ORIENTED_EDGE ( 'NONE', *, *, #63427, .T. ) ;
#40608 = VERTEX_POINT ( 'NONE', #22019 ) ;
#40609 = CARTESIAN_POINT ( 'NONE',  ( -100.3181550757389147, -25.12215674754353856, 7.099295233261272209 ) ) ;
#40610 = ORIENTED_EDGE ( 'NONE', *, *, #43495, .F. ) ;
#40611 = CARTESIAN_POINT ( 'NONE',  ( -19.04320821261859464, -9.809917703373946196, -1.500000000000002220 ) ) ;
#40612 = CARTESIAN_POINT ( 'NONE',  ( 10.24050353823403192, -19.87907451059620456, 11.49999999999999645 ) ) ;
#40613 = ORIENTED_EDGE ( 'NONE', *, *, #40295, .T. ) ;
#40614 = CARTESIAN_POINT ( 'NONE',  ( 32.48849721025742099, -4.168223360657076881, -0.9137309853436130780 ) ) ;
#40615 = CARTESIAN_POINT ( 'NONE',  ( 3.661087877195506213, -20.73962600213626217, -1.500000000000002220 ) ) ;
#40616 = CARTESIAN_POINT ( 'NONE',  ( -30.63484830301900175, -23.79244928165773842, 10.97490056816818971 ) ) ;
#40617 = EDGE_CURVE ( 'NONE', #15460, #42617, #53008, .T. ) ;
#40618 = CARTESIAN_POINT ( 'NONE',  ( -17.52048005523606022, -9.576713672051738513, -1.500000000000002220 ) ) ;
#40619 = FACE_OUTER_BOUND ( 'NONE', #26273, .T. ) ;
#40620 = CARTESIAN_POINT ( 'NONE',  ( -43.52287095715008292, -23.96177878511307924, 10.65340807706330573 ) ) ;
#40621 = CARTESIAN_POINT ( 'NONE',  ( -10.85839155550747392, 19.17434714687634667, -1.500000000000002220 ) ) ;
#40622 = EDGE_LOOP ( 'NONE', ( #40749, #6014, #2419, #24701 ) ) ;
#40623 = CARTESIAN_POINT ( 'NONE',  ( -65.66192790180473082, -23.48786465467241058, 11.44779295918254824 ) ) ;
#40624 = EDGE_CURVE ( 'NONE', #47721, #56484, #2128, .T. ) ;
#40625 = CARTESIAN_POINT ( 'NONE',  ( 0.000000000000000000, -16.94322527948557422, 0.000000000000000000 ) ) ;
#40626 = CARTESIAN_POINT ( 'NONE',  ( 11.47802407633690258, -17.41396394059345454, 11.49999999999999645 ) ) ;
#40627 = EDGE_CURVE ( 'NONE', #57808, #23980, #31145, .T. ) ;
#40628 = CARTESIAN_POINT ( 'NONE',  ( 31.68813401132623397, -4.191046033661507408, 29.35543347196376729 ) ) ;
#40629 = EDGE_CURVE ( 'NONE', #73668, #66916, #55620, .T. ) ;
#40630 = LINE ( 'NONE', #93900, #97561 ) ;
#40631 = CARTESIAN_POINT ( 'NONE',  ( -61.52287095715006160, -24.65952944569304606, 1.056160979905695463 ) ) ;
#40632 = CARTESIAN_POINT ( 'NONE',  ( -1.376967878889499897, 21.29249089469206524, 11.49999999999998934 ) ) ;
#40633 = CARTESIAN_POINT ( 'NONE',  ( -19.80875734969026425, 5.965225279485572685, 30.51402280011862089 ) ) ;
#40634 = EDGE_CURVE ( 'NONE', #90027, #53562, #84433, .T. ) ;
#40635 = CARTESIAN_POINT ( 'NONE',  ( -110.2093792378191921, -25.29160350784524880, 5.585409231008217290 ) ) ;
#40636 = CIRCLE ( 'NONE', #16281, 84.48086791635431325 ) ;
#40637 = CARTESIAN_POINT ( 'NONE',  ( -32.52287095715006160, -23.47596703998600631, 11.44779298504229459 ) ) ;
#40638 = CARTESIAN_POINT ( 'NONE',  ( -69.33422667675866080, -25.12112739299269037, 7.112216829152949948 ) ) ;
#40639 = CARTESIAN_POINT ( 'NONE',  ( 21.37280783159109276, 7.349196219051140844, -1.500000000000002220 ) ) ;
#40640 = CARTESIAN_POINT ( 'NONE',  ( -88.88918693012686845, -25.23397913219354649, 6.409327625488847602 ) ) ;
#40641 = ORIENTED_EDGE ( 'NONE', *, *, #21357, .T. ) ;
#40642 = CARTESIAN_POINT ( 'NONE',  ( -79.62713573843802806, -25.30166916552286693, 4.689104876704957015 ) ) ;
#40643 = CARTESIAN_POINT ( 'NONE',  ( -31.48242477323742605, -24.51419770103156637, 9.386484678747187615 ) ) ;
#40644 = CARTESIAN_POINT ( 'NONE',  ( 6.578723047037327909, -18.57437435983987584, 11.49999999999999645 ) ) ;
#40645 = CARTESIAN_POINT ( 'NONE',  ( -93.55620429048339304, -23.48786465467241413, 11.44779295918253936 ) ) ;
#40646 = FACE_OUTER_BOUND ( 'NONE', #29937, .T. ) ;
#40647 = EDGE_CURVE ( 'NONE', #43715, #28435, #91195, .T. ) ;
#40648 = B_SPLINE_CURVE_WITH_KNOTS ( 'NONE', 3,
 ( #89, #49290, #78689, #87323 ),
 .UNSPECIFIED., .F., .F.,
 ( 4, 4 ),
 ( 0.1088347601982936758, 0.1098355072390591741 ),
 .UNSPECIFIED. ) ;
#40649 = ORIENTED_EDGE ( 'NONE', *, *, #60323, .T. ) ;
#40650 = CARTESIAN_POINT ( 'NONE',  ( -89.52287095715006160, -24.64965694238407323, 8.947790433994196491 ) ) ;
#40651 = DIRECTION ( 'NONE',  ( 0.7512896232465891000, 0.000000000000000000, 0.6599726524652351767 ) ) ;
#40652 = DIRECTION ( 'NONE',  ( 0.000000000000000000, -0.9999999999976377785, -2.173523156925979128E-06 ) ) ;
#40653 = CARTESIAN_POINT ( 'NONE',  ( -120.6228709571500417, -24.99132157543166954, 2.256160258750667502 ) ) ;
#40654 = FACE_OUTER_BOUND ( 'NONE', #41221, .T. ) ;
#40655 = CARTESIAN_POINT ( 'NONE',  ( 2.412641546452875208, 19.58572291230954221, 11.49999999999998934 ) ) ;
#40656 = AXIS2_PLACEMENT_3D ( 'NONE', #3092, #71596, #56884 ) ;
#40657 = ORIENTED_EDGE ( 'NONE', *, *, #93416, .T. ) ;
#40658 = AXIS2_PLACEMENT_3D ( 'NONE', #37697, #68657, #62544 ) ;
#40659 = CARTESIAN_POINT ( 'NONE',  ( -19.21899500656021331, -6.280627263257740900, 11.49999999999999645 ) ) ;
#40660 = CARTESIAN_POINT ( 'NONE',  ( -72.62287095715005592, -24.64898659630367916, 1.056161002820824368 ) ) ;
#40661 = ORIENTED_EDGE ( 'NONE', *, *, #81996, .F. ) ;
#40662 = CARTESIAN_POINT ( 'NONE',  ( -110.6228709571500417, -24.52232992886363760, 0.6492154411906180256 ) ) ;
#40663 = CARTESIAN_POINT ( 'NONE',  ( -69.48291834206632700, -25.28410036694619123, 5.733557524135145300 ) ) ;
#40664 = DIRECTION ( 'NONE',  ( -0.000000000000000000, -0.000000000000000000, -1.000000000000000000 ) ) ;
#40665 = DIRECTION ( 'NONE',  ( -1.000000000000000000, -3.773278334444167608E-23, -8.201307833595939069E-29 ) ) ;
#40666 = CARTESIAN_POINT ( 'NONE',  ( -95.62287095715005592, -29.50250786944525672, 11.44777988621623166 ) ) ;
#40667 = DIRECTION ( 'NONE',  ( 0.000000000000000000, -0.000000000000000000, -1.000000000000000000 ) ) ;
#40668 = CARTESIAN_POINT ( 'NONE',  ( 14.90458806734895703, -13.33898509196910886, -1.500000000000002220 ) ) ;
#40669 = EDGE_CURVE ( 'NONE', #13572, #47484, #96434, .T. ) ;
#40670 = DIRECTION ( 'NONE',  ( -0.000000000000000000, 2.173523156925979552E-06, -0.9999999999976378895 ) ) ;
#40671 = CARTESIAN_POINT ( 'NONE',  ( -116.6251858524873342, -24.35071581493544102, 9.817618358456021710 ) ) ;
#40672 = EDGE_LOOP ( 'NONE', ( #24833, #91755, #1154, #17614 ) ) ;
#40673 = B_SPLINE_CURVE_WITH_KNOTS ( 'NONE', 3,
 ( #56750, #57743, #82060, #25776 ),
 .UNSPECIFIED., .F., .F.,
 ( 4, 4 ),
 ( 0.000000000000000000, 9.999999999998898659E-05 ),
 .UNSPECIFIED. ) ;
#40674 = CARTESIAN_POINT ( 'NONE',  ( -69.86226847989213695, -25.12049686670126292, 2.832401160916445004 ) ) ;
#40675 = CARTESIAN_POINT ( 'NONE',  ( -33.62287095715005592, -24.65952944569304250, 1.056160979905690356 ) ) ;
#40676 = CARTESIAN_POINT ( 'NONE',  ( -92.62287095715005592, -24.64965695001469115, 8.947790433994180503 ) ) ;
#40677 = CARTESIAN_POINT ( 'NONE',  ( -124.5895376238167103, -24.65952944569304961, 1.056160979905701902 ) ) ;
#40678 = CARTESIAN_POINT ( 'NONE',  ( -51.69903695958453227, -25.31574265807444846, 4.034228563096281306 ) ) ;
#40679 = DIRECTION ( 'NONE',  ( -1.000000000000000000, 0.000000000000000000, 0.000000000000000000 ) ) ;
#40680 = EDGE_CURVE ( 'NONE', #24252, #58964, #68901, .T. ) ;
#40681 = CARTESIAN_POINT ( 'NONE',  ( -49.54527677626192883, -25.24403278070153789, 3.779632570335008435 ) ) ;
#40682 = ORIENTED_EDGE ( 'NONE', *, *, #92475, .T. ) ;
#40683 = CARTESIAN_POINT ( 'NONE',  ( -6.898722100468609675, -19.10483383855023476, -1.500000000000002220 ) ) ;
#40684 = EDGE_CURVE ( 'NONE', #68689, #79343, #16922, .T. ) ;
#40685 = CARTESIAN_POINT ( 'NONE',  ( -114.9228709571500673, -23.47593901973090169, -1.443836447538996426 ) ) ;
#40686 = CARTESIAN_POINT ( 'NONE',  ( 0.000000000000000000, 4.132774720514426292, 0.000000000000000000 ) ) ;
#40687 = CARTESIAN_POINT ( 'NONE',  ( -107.5228709571500900, -24.35013146730204170, 9.818937971375099494 ) ) ;
#40688 = ORIENTED_EDGE ( 'NONE', *, *, #93811, .F. ) ;
#40689 = CARTESIAN_POINT ( 'NONE',  ( 31.02038118199824268, -5.152774720514427642, -4.893189986691015569 ) ) ;
#40690 = CARTESIAN_POINT ( 'NONE',  ( -21.11812214938331422, 0.5215410354952813021, 11.49999999999999645 ) ) ;
#40691 = CARTESIAN_POINT ( 'NONE',  ( -0.9539927174334467130, 22.11892580961223587, 11.49999999999998934 ) ) ;
#40692 = AXIS2_PLACEMENT_3D ( 'NONE', #63885, #41526, #30016 ) ;
#40693 = CARTESIAN_POINT ( 'NONE',  ( -19.32567751138619982, -7.045664331180771178, 11.49999999999998934 ) ) ;
#40694 = ORIENTED_EDGE ( 'NONE', *, *, #61725, .T. ) ;
#40695 = FACE_OUTER_BOUND ( 'NONE', #88882, .T. ) ;
#40696 = ORIENTED_EDGE ( 'NONE', *, *, #49680, .F. ) ;
#40697 = CARTESIAN_POINT ( 'NONE',  ( 7.153659783701941777, -6.376774720514422512, 20.92502190304499265 ) ) ;
#40698 = CARTESIAN_POINT ( 'NONE',  ( -70.52287095715007581, -23.47596703998600631, 11.44779298504228748 ) ) ;
#40699 = EDGE_LOOP ( 'NONE', ( #80530, #85924, #1017, #4872 ) ) ;
#40700 = ORIENTED_EDGE ( 'NONE', *, *, #39535, .T. ) ;
#40701 = ORIENTED_EDGE ( 'NONE', *, *, #71603, .F. ) ;
#40702 = CARTESIAN_POINT ( 'NONE',  ( -100.5228709571500616, -24.82558206586143612, 1.605769216559450152 ) ) ;
#40703 = CARTESIAN_POINT ( 'NONE',  ( 6.457852148677970305, -5.876774720514415407, 20.09052163342618158 ) ) ;
#40704 = CARTESIAN_POINT ( 'NONE',  ( 5.873458226074941280, -5.876774720514413630, 19.84669099281175164 ) ) ;
#40705 = CARTESIAN_POINT ( 'NONE',  ( 3.345817365282868217, 20.41450801592841557, -1.500000000000002220 ) ) ;
#40706 = CARTESIAN_POINT ( 'NONE',  ( -18.45943378446990835, 11.37049804852326140, 11.49999999999999645 ) ) ;
#40707 = VERTEX_POINT ( 'NONE', #89817 ) ;
#40708 = LINE ( 'NONE', #44213, #54793 ) ;
#40709 = CARTESIAN_POINT ( 'NONE',  ( -110.9770695239891012, -25.13602867479627179, 2.978790624164922018 ) ) ;
#40710 = CARTESIAN_POINT ( 'NONE',  ( 20.53814608839396527, -8.957171556794316203, -1.500000000000002220 ) ) ;
#40711 = CARTESIAN_POINT ( 'NONE',  ( -92.62287095715005592, -23.47593901973091235, -1.443836447539002865 ) ) ;
#40712 = CARTESIAN_POINT ( 'NONE',  ( -101.5228709571500758, -23.72773821059536203, 11.05748984161097148 ) ) ;
#40713 = VERTEX_POINT ( 'NONE', #73601 ) ;
#40714 = CARTESIAN_POINT ( 'NONE',  ( -54.62287095715005592, -29.50250786944525672, 11.44777988621624054 ) ) ;
#40715 = AXIS2_PLACEMENT_3D ( 'NONE', #18302, #24901, #1585 ) ;
#40716 = CARTESIAN_POINT ( 'NONE',  ( -120.6228709571500417, -23.85229601348997619, 10.88205029486208275 ) ) ;
#40717 = EDGE_LOOP ( 'NONE', ( #88449, #84113, #26394, #60311 ) ) ;
#40718 = ORIENTED_EDGE ( 'NONE', *, *, #28753, .F. ) ;
#40719 = CARTESIAN_POINT ( 'NONE',  ( -59.52287095715006160, -29.50250243563736774, 8.947779886222145151 ) ) ;
#40720 = VERTEX_POINT ( 'NONE', #88832 ) ;
#40721 = CARTESIAN_POINT ( 'NONE',  ( 1.600000000000000755, 0.000000000000000000, 19.30000000000000071 ) ) ;
#40722 = CARTESIAN_POINT ( 'NONE',  ( 4.903939382885006637, -20.63555827282145572, -1.500000000000002220 ) ) ;
#40723 = EDGE_LOOP ( 'NONE', ( #16447, #79436, #96440, #12720 ) ) ;
#40724 = CARTESIAN_POINT ( 'NONE',  ( -50.47485263706386149, -25.00158670708910691, 2.256160236439223254 ) ) ;
#40725 = CARTESIAN_POINT ( 'NONE',  ( -20.50126671893153940, -7.481214725051755110, 11.49999999999998934 ) ) ;
#40726 = CARTESIAN_POINT ( 'NONE',  ( -52.48645163059850915, -24.66019654487198665, 8.947790411086131712 ) ) ;
#40727 = CARTESIAN_POINT ( 'NONE',  ( 3.180076745125948179, -5.965225279485592225, -28.87659520466657526 ) ) ;
#40728 = CARTESIAN_POINT ( 'NONE',  ( 29.80070917940689768, -3.316774720514426456, 27.39560796525317343 ) ) ;
#40729 = CARTESIAN_POINT ( 'NONE',  ( 21.83365961380331655, 0.8745889840297637052, -1.500000000000002220 ) ) ;
#40730 = CARTESIAN_POINT ( 'NONE',  ( -30.57287095715005520, -25.30541082164580757, 5.278019199569442321 ) ) ;
#40731 = ORIENTED_EDGE ( 'NONE', *, *, #90892, .T. ) ;
#40732 = CARTESIAN_POINT ( 'NONE',  ( 25.20856462023905564, 4.845009571353474875, -10.39575909395317943 ) ) ;
#40733 = CARTESIAN_POINT ( 'NONE',  ( -85.63004653390532894, -24.63419186844611275, 9.035850630976915099 ) ) ;
#40734 = ORIENTED_EDGE ( 'NONE', *, *, #21257, .F. ) ;
#40735 = ORIENTED_EDGE ( 'NONE', *, *, #41684, .F. ) ;
#40736 = ORIENTED_EDGE ( 'NONE', *, *, #45034, .F. ) ;
#40737 = ADVANCED_FACE ( 'NONE', ( #19300 ), #3106, .F. ) ;
#40738 = CARTESIAN_POINT ( 'NONE',  ( -79.11611000704996854, -25.20074463982482982, 3.409327697717700278 ) ) ;
#40739 = CARTESIAN_POINT ( 'NONE',  ( -82.54135565317993439, -24.65952944569304606, 1.056160979905703012 ) ) ;
#40740 = B_SPLINE_CURVE_WITH_KNOTS ( 'NONE', 3,
 ( #82857, #13842, #97097, #29572 ),
 .UNSPECIFIED., .F., .F.,
 ( 4, 4 ),
 ( 0.000000000000000000, 9.999999999998897304E-05 ),
 .UNSPECIFIED. ) ;
#40741 = CARTESIAN_POINT ( 'NONE',  ( -21.08860491664495029, 2.407354197416772035, -1.500000000000002220 ) ) ;
#40742 = CARTESIAN_POINT ( 'NONE',  ( -125.5562042904833930, -25.00182538069145721, 7.747789668545099317 ) ) ;
#40743 = EDGE_CURVE ( 'NONE', #36540, #52940, #85795, .T. ) ;
#40744 = CARTESIAN_POINT ( 'NONE',  ( -81.62287095715005592, -29.50250786944525672, 11.44777988621623521 ) ) ;
#40745 = DIRECTION ( 'NONE',  ( -1.000000000000000000, 0.000000000000000000, 2.000709955812756815E-15 ) ) ;
#40746 = CARTESIAN_POINT ( 'NONE',  ( -128.5895376238167103, -23.47593901973091235, -1.443836447538995760 ) ) ;
#40747 = CARTESIAN_POINT ( 'NONE',  ( 11.07193147992585835, -15.93265361536492364, -1.500000000000002220 ) ) ;
#40748 = CARTESIAN_POINT ( 'NONE',  ( -45.55047939234961518, -24.15503026093915651, -0.2815557561904415418 ) ) ;
#40749 = ORIENTED_EDGE ( 'NONE', *, *, #90444, .F. ) ;
#40750 = CARTESIAN_POINT ( 'NONE',  ( -13.24781383850973349, 14.34467480260970795, 11.49999999999999645 ) ) ;
#40751 = CARTESIAN_POINT ( 'NONE',  ( -5.154768636056045850, -5.876774720514411854, 19.48351902941045921 ) ) ;
#40752 = PLANE ( 'NONE',  #91725 ) ;
#40753 = EDGE_CURVE ( 'NONE', #61052, #65701, #53103, .T. ) ;
#40754 = EDGE_LOOP ( 'NONE', ( #43609, #36179, #81914, #61526 ) ) ;
#40755 = CARTESIAN_POINT ( 'NONE',  ( -99.52287095715006160, -23.47596703998600631, 11.44779298504228215 ) ) ;
#40756 = CARTESIAN_POINT ( 'NONE',  ( -32.62287095715004881, -23.48786465467240347, 11.44779295918255535 ) ) ;
#40757 = B_SPLINE_CURVE_WITH_KNOTS ( 'NONE', 3,
 ( #34331, #72399, #42951, #10988 ),
 .UNSPECIFIED., .F., .F.,
 ( 4, 4 ),
 ( 0.000000000000000000, 9.999999999994735322E-05 ),
 .UNSPECIFIED. ) ;
#40758 = CYLINDRICAL_SURFACE ( 'NONE', #77970, 3.500000000000000000 ) ;
#40759 = CARTESIAN_POINT ( 'NONE',  ( -80.89908437845683409, -25.24813981080061609, 7.516074972019308298 ) ) ;
#40760 = CARTESIAN_POINT ( 'NONE',  ( -18.24527198174902765, 7.358211898524878336, 11.49999999999998934 ) ) ;
#40761 = ORIENTED_EDGE ( 'NONE', *, *, #100121, .T. ) ;
#40762 = AXIS2_PLACEMENT_3D ( 'NONE', #87069, #31277, #832 ) ;
#40763 = CARTESIAN_POINT ( 'NONE',  ( -63.62287095715004881, -29.50250786944525672, 11.44777988621623876 ) ) ;
#40764 = CARTESIAN_POINT ( 'NONE',  ( 14.65057173600216345, 17.85730367728733725, -1.500000000000002220 ) ) ;
#40765 = CALENDAR_DATE ( 2026, 9, 10 ) ;
#40766 = CARTESIAN_POINT ( 'NONE',  ( 3.206569032998081603, -5.876774720514423400, 21.19686455982786200 ) ) ;
#40767 = CARTESIAN_POINT ( 'NONE',  ( -90.52287095715009002, -24.51254535375846544, 9.355368624242132114 ) ) ;
#40768 = CARTESIAN_POINT ( 'NONE',  ( -114.6228709571500559, -24.64898659630528854, 1.056161002820831474 ) ) ;
#40769 = CARTESIAN_POINT ( 'NONE',  ( -76.52287095715011844, -23.48783264082477373, -1.443836473390087694 ) ) ;
#40770 = CARTESIAN_POINT ( 'NONE',  ( -119.5228709571500900, -23.94994826722565406, -0.6494450866342709183 ) ) ;
#40771 = APPLICATION_CONTEXT ( 'configuration controlled 3d designs of mechanical parts and assemblies' ) ;
#40772 = DIRECTION ( 'NONE',  ( 0.9921023176230513441, 0.000000000000000000, -0.1254312216594016538 ) ) ;
#40773 = CARTESIAN_POINT ( 'NONE',  ( -73.52287095715006160, -23.73934037231756733, 11.05740245334329153 ) ) ;
#40774 = CARTESIAN_POINT ( 'NONE',  ( -111.3439979973304332, -25.29779330784409552, 4.101024009883487587 ) ) ;
#40775 = CARTESIAN_POINT ( 'NONE',  ( -18.10700488460823721, -8.296952762055457953, 11.49999999999998934 ) ) ;
#40776 = CARTESIAN_POINT ( 'NONE',  ( -75.62935365942843191, -24.73531770709095312, 8.716586749053512051 ) ) ;
#40777 = CARTESIAN_POINT ( 'NONE',  ( 16.83370257367741019, -10.51912618480096206, -1.500000000000002220 ) ) ;
#40778 = ORIENTED_EDGE ( 'NONE', *, *, #19841, .T. ) ;
#40779 = DIRECTION ( 'NONE',  ( -0.000000000000000000, -1.000000000000000000, -0.000000000000000000 ) ) ;
#40780 = EDGE_CURVE ( 'NONE', #39121, #43756, #42667, .T. ) ;
#40781 = AXIS2_PLACEMENT_3D ( 'NONE', #48668, #55775, #86700 ) ;
#40782 = SECURITY_CLASSIFICATION ( '', '', #36392 ) ;
#40783 = CARTESIAN_POINT ( 'NONE',  ( -125.5228709571500616, -24.51163499207176244, 0.6490370598554348058 ) ) ;
#40784 = CARTESIAN_POINT ( 'NONE',  ( -92.62287095715005592, -29.50247984919015209, -1.443849546365051806 ) ) ;
#40785 = CARTESIAN_POINT ( 'NONE',  ( 11.56195852851363526, -17.29799701895051811, 11.49999999999999645 ) ) ;
#40786 = FACE_OUTER_BOUND ( 'NONE', #67409, .T. ) ;
#40787 = EDGE_CURVE ( 'NONE', #12406, #84010, #89323, .T. ) ;
#40788 = CARTESIAN_POINT ( 'NONE',  ( -106.6264179404533508, -24.34968618360933945, 0.1864209137778878034 ) ) ;
#40789 = CARTESIAN_POINT ( 'NONE',  ( -4.374245501123523283, 22.36648047097513725, 11.49999999999999645 ) ) ;
#40790 = ORIENTED_EDGE ( 'NONE', *, *, #36513, .F. ) ;
#40791 = CARTESIAN_POINT ( 'NONE',  ( -69.54085705957912467, -24.51314013834315375, 0.6176544820404143987 ) ) ;
#40792 = CARTESIAN_POINT ( 'NONE',  ( -92.52287095715006160, -23.72773821059536914, 11.05748984161097326 ) ) ;
#40793 = VERTEX_POINT ( 'NONE', #18803 ) ;
#40794 = CARTESIAN_POINT ( 'NONE',  ( -10.81679630089563915, -17.07601267366916886, -1.500000000000002220 ) ) ;
#40795 = CARTESIAN_POINT ( 'NONE',  ( -33.62287095715005592, -29.50248528299804818, 1.056150453629029817 ) ) ;
#40796 = CARTESIAN_POINT ( 'NONE',  ( -53.01255352321339842, 4.772774720514425972, 35.59556822165056644 ) ) ;
#40797 = ORIENTED_EDGE ( 'NONE', *, *, #68506, .T. ) ;
#40798 = CARTESIAN_POINT ( 'NONE',  ( -105.5228709571500616, -29.50248789122583659, 2.256150453626215580 ) ) ;
#40799 = LINE ( 'NONE', #24565, #95625 ) ;
#40800 = CARTESIAN_POINT ( 'NONE',  ( 4.555139465550277933, 19.45931829295258453, -1.500000000000002220 ) ) ;
#40801 = CARTESIAN_POINT ( 'NONE',  ( -29.49975734969026320, -6.475225279485573360, 13.17908622612278613 ) ) ;
#40802 = CARTESIAN_POINT ( 'NONE',  ( 19.98859412959824411, 6.261702723725245612, 11.49999999999999645 ) ) ;
#40803 = CARTESIAN_POINT ( 'NONE',  ( 5.399550031317769339, 5.965225279485594001, -28.54570968858208246 ) ) ;
#40804 = CARTESIAN_POINT ( 'NONE',  ( -79.55620429048340725, -24.64965694238574656, 8.947790433994196491 ) ) ;
#40805 = CARTESIAN_POINT ( 'NONE',  ( 20.91424602935089894, 6.983905699820807556, 11.49999999999998934 ) ) ;
#40806 = EDGE_CURVE ( 'NONE', #22913, #79917, #49779, .T. ) ;
#40807 = CARTESIAN_POINT ( 'NONE',  ( 30.00738719773715601, -4.772774720514425972, -9.049252915307082645 ) ) ;
#40808 = EDGE_LOOP ( 'NONE', ( #10312, #53689, #75135, #27266 ) ) ;
#40809 = VECTOR ( 'NONE', #60095, 1000.000000000000000 ) ;
#40810 = LINE ( 'NONE', #18970, #69465 ) ;
#40811 = DIRECTION ( 'NONE',  ( -1.000000000000000000, -3.773278334444166432E-23, -8.201307841325785021E-29 ) ) ;
#40812 = CARTESIAN_POINT ( 'NONE',  ( -72.50263257038113807, -24.34968618360933590, 0.1864209137778795600 ) ) ;
#40813 = ORIENTED_EDGE ( 'NONE', *, *, #24780, .T. ) ;
#40814 = CARTESIAN_POINT ( 'NONE',  ( 3.475076759263674209, -6.376774720514401196, 18.20843037655054530 ) ) ;
#40815 = EDGE_LOOP ( 'NONE', ( #71339, #95386, #82385, #88747 ) ) ;
#40816 = ORIENTED_EDGE ( 'NONE', *, *, #24330, .F. ) ;
#40817 = CARTESIAN_POINT ( 'NONE',  ( -79.22287095715010707, -23.47593901973090524, -1.443836447538997536 ) ) ;
#40818 = CARTESIAN_POINT ( 'NONE',  ( -85.52287095715009002, -23.47593901973090524, -1.443836447538996648 ) ) ;
#40819 = CARTESIAN_POINT ( 'NONE',  ( -122.5895376238167387, -23.48786465467242124, 11.44779295918253759 ) ) ;
#40820 = CARTESIAN_POINT ( 'NONE',  ( 16.43461662053371697, -12.34185696772103391, -1.500000000000002220 ) ) ;
#40821 = ORIENTED_EDGE ( 'NONE', *, *, #86545, .T. ) ;
#40822 = CARTESIAN_POINT ( 'NONE',  ( -99.35299720551914504, -25.27660924118455910, 5.844709891833338666 ) ) ;
#40823 = EDGE_CURVE ( 'NONE', #25493, #85607, #14435, .T. ) ;
#40824 = DIRECTION ( 'NONE',  ( 0.000000000000000000, 0.000000000000000000, 1.000000000000000000 ) ) ;
#40825 = CARTESIAN_POINT ( 'NONE',  ( -96.62287095715005592, -24.66019654487199730, 8.947790411086124607 ) ) ;
#40826 = CARTESIAN_POINT ( 'NONE',  ( -7.907391756136429528, -20.87048397725295956, 11.49999999999998934 ) ) ;
#40827 = CARTESIAN_POINT ( 'NONE',  ( -81.62287095715005592, -24.50216790748099882, 0.6166512839513619282 ) ) ;
#40828 = DIRECTION ( 'NONE',  ( -3.773278334444166432E-23, 1.000000000000000000, 0.000000000000000000 ) ) ;
#40829 = VERTEX_POINT ( 'NONE', #80713 ) ;
#40830 = FACE_OUTER_BOUND ( 'NONE', #77226, .T. ) ;
#40831 = CARTESIAN_POINT ( 'NONE',  ( -65.62287095715005592, -24.99132157543084176, 2.256160258750667502 ) ) ;
#40832 = CARTESIAN_POINT ( 'NONE',  ( -9.832896139050584239, -18.40278743011522877, -1.500000000000002220 ) ) ;
#40833 = AXIS2_PLACEMENT_3D ( 'NONE', #34668, #4216, #57519 ) ;
#40834 = ORIENTED_EDGE ( 'NONE', *, *, #76930, .T. ) ;
#40836 = ORIENTED_EDGE ( 'NONE', *, *, #13274, .T. ) ;
#40835 = DIRECTION ( 'NONE',  ( -0.000000000000000000, 1.000000000000000000, -0.000000000000000000 ) ) ;
#40837 = ORIENTED_EDGE ( 'NONE', *, *, #97082, .T. ) ;
#40838 = CARTESIAN_POINT ( 'NONE',  ( -58.87764846858842560, -29.50248939449842922, 2.947779886236309377 ) ) ;
#40839 = CARTESIAN_POINT ( 'NONE',  ( -2.129267666952235682, 20.92775224702969439, -1.500000000000002220 ) ) ;
#40840 = ORIENTED_EDGE ( 'NONE', *, *, #75642, .T. ) ;
#40841 = DIRECTION ( 'NONE',  ( 0.000000000000000000, -0.9999999999976377785, -2.173523156925979128E-06 ) ) ;
#40842 = CARTESIAN_POINT ( 'NONE',  ( 6.660000000000001030, -10.97586050609889519, -0.8902240841051127784 ) ) ;
#40843 = CARTESIAN_POINT ( 'NONE',  ( -111.6228709571500559, -23.47593901973091235, -1.443836447538999312 ) ) ;
#40844 = CARTESIAN_POINT ( 'NONE',  ( -86.55119192925248228, -24.15620529776628445, 10.23563542870660292 ) ) ;
#40845 = ADVANCED_FACE ( 'NONE', ( #27428 ), #43159, .T. ) ;
#40846 = CARTESIAN_POINT ( 'NONE',  ( -49.62287095715005592, -24.64898659630528499, 1.056161002820821038 ) ) ;
#40847 = CARTESIAN_POINT ( 'NONE',  ( 3.708801897538985148, -21.39311272803122321, -1.500000000000002220 ) ) ;
#40848 = DIRECTION ( 'NONE',  ( -0.000000000000000000, 1.000000000000000000, -0.000000000000000000 ) ) ;
#40849 = EDGE_CURVE ( 'NONE', #87869, #22875, #20788, .T. ) ;
#40851 = ORIENTED_EDGE ( 'NONE', *, *, #6924, .F. ) ;
#40850 = CARTESIAN_POINT ( 'NONE',  ( -10.57539506955483333, 19.50334513348995813, 11.49999999999999645 ) ) ;
#40852 = DIRECTION ( 'NONE',  ( 0.000000000000000000, -1.478457507934778393E-16, -1.000000000000000000 ) ) ;
#40853 = CARTESIAN_POINT ( 'NONE',  ( -71.30260502180048832, -25.25163510122737165, 6.148193815974848597 ) ) ;
#40854 = VERTEX_POINT ( 'NONE', #36028 ) ;
#40855 = CARTESIAN_POINT ( 'NONE',  ( 14.05383982582471170, -17.77673030755399708, -1.500000000000002220 ) ) ;
#40856 = B_SPLINE_CURVE_WITH_KNOTS ( 'NONE', 3,
 ( #22292, #85715, #8088, #69985, #84704, #46662 ),
 .UNSPECIFIED., .F., .F.,
 ( 4, 2, 4 ),
 ( 1.570755371634052715E-05, 0.001396183895866088187, 0.002776660238015835579 ),
 .UNSPECIFIED. ) ;
#40858 = ORIENTED_EDGE ( 'NONE', *, *, #53564, .F. ) ;
#40857 = CARTESIAN_POINT ( 'NONE',  ( -5.903826827417286260, -6.376774720514418959, 20.39230070883895252 ) ) ;
#40859 = B_SPLINE_CURVE_WITH_KNOTS ( 'NONE', 3,
 ( #5213, #12313, #98046, #28541 ),
 .UNSPECIFIED., .F., .F.,
 ( 4, 4 ),
 ( 0.000000000000000000, 9.999999999998897304E-05 ),
 .UNSPECIFIED. ) ;
#40860 = AXIS2_PLACEMENT_3D ( 'NONE', #13809, #97560, #28060 ) ;
#40861 = ORIENTED_EDGE ( 'NONE', *, *, #51327, .T. ) ;
#40862 = CC_DESIGN_SECURITY_CLASSIFICATION ( #68385, ( #16510 ) ) ;
#40863 = CARTESIAN_POINT ( 'NONE',  ( -101.5228709571500758, -23.48786465467241769, 11.44779295918254114 ) ) ;
#40864 = EDGE_CURVE ( 'NONE', #24496, #48489, #99061, .T. ) ;
#40865 = CARTESIAN_POINT ( 'NONE',  ( 13.10547390533899836, 15.29217475743441312, 11.49999999999998934 ) ) ;
#40866 = EDGE_CURVE ( 'NONE', #4006, #69692, #75078, .T. ) ;
#40867 = CARTESIAN_POINT ( 'NONE',  ( -105.5228709571501042, -23.48783264082477018, -1.443836473390085917 ) ) ;
#40868 = ORIENTED_EDGE ( 'NONE', *, *, #51844, .F. ) ;
#40869 = CARTESIAN_POINT ( 'NONE',  ( -130.5728709571500588, -24.64113408559786933, 0.7260449476895605159 ) ) ;
#40870 = CARTESIAN_POINT ( 'NONE',  ( 1.438201247614206757, 22.34484416265529916, -1.500000000000002220 ) ) ;
#40871 = EDGE_CURVE ( 'NONE', #21106, #25496, #21620, .T. ) ;
#40872 = ORIENTED_EDGE ( 'NONE', *, *, #42483, .T. ) ;
#40873 = ORIENTED_EDGE ( 'NONE', *, *, #83577, .F. ) ;
#40874 = CARTESIAN_POINT ( 'NONE',  ( -89.40841769935767047, -25.06732983082694943, 7.447789526168953955 ) ) ;
#40875 = CARTESIAN_POINT ( 'NONE',  ( -94.52217260166209201, -23.48786465467241058, 11.44779295918254469 ) ) ;
#40876 = CARTESIAN_POINT ( 'NONE',  ( -16.22218391600152643, 6.475225279485573360, -54.85883559227303863 ) ) ;
#40877 = DIRECTION ( 'NONE',  ( 0.000000000000000000, 0.000000000000000000, 1.000000000000000000 ) ) ;
#40878 = EDGE_CURVE ( 'NONE', #26965, #18629, #76616, .T. ) ;
#40879 = CARTESIAN_POINT ( 'NONE',  ( -97.24912498359577739, -24.57143472585066490, 0.8294870405985540485 ) ) ;
#40880 = CARTESIAN_POINT ( 'NONE',  ( -6.365771329251782795, -18.49506561991874065, 11.49999999999998934 ) ) ;
#40881 = B_SPLINE_SURFACE_WITH_KNOTS ( 'NONE', 3, 1, ( 
 ( #51908, #29052 ),
 ( #61016, #12822 ),
 ( #91949, #43793 ),
 ( #83838, #5223 ),
 ( #6712, #98054 ),
 ( #59519, #98555 ),
 ( #37665, #5719 ),
 ( #90456, #36668 ),
 ( #83337, #13817 ),
 ( #40678, #2126 ),
 ( #93440, #16325 ) ),
 .UNSPECIFIED., .F., .F., .F.,
 ( 4, 1, 1, 1, 1, 1, 1, 1, 4 ),
 ( 2, 2 ),
 ( 0.000000000000000000, 0.1458600603916643534, 0.2824259030758165534, 0.4108504003575531582, 0.5350294213479291905, 0.6547010781259405832, 0.7701334325965021321, 0.8845558441988605747, 1.000000000000000000 ),
 ( 0.000000000000000000, 1.000000000000000000 ),
 .UNSPECIFIED. ) ;
#40882 = CARTESIAN_POINT ( 'NONE',  ( -46.59984531427831911, -23.96119346886879953, -0.6495511937832144644 ) ) ;
#40883 = VERTEX_POINT ( 'NONE', #13675 ) ;
#40884 = CARTESIAN_POINT ( 'NONE',  ( 21.22668844964908885, 3.412186807495566132, -1.500000000000002220 ) ) ;
#40885 = CARTESIAN_POINT ( 'NONE',  ( -128.5561025698958701, -23.73766607897671932, -1.055555164236423149 ) ) ;
#40886 = CARTESIAN_POINT ( 'NONE',  ( 20.07151214508649772, 3.809612236891415094E-15, -1.699999999999999956 ) ) ;
#40887 = CARTESIAN_POINT ( 'NONE',  ( 282.9764569301858046, -0.3587747205144265483, 20.79159422840526616 ) ) ;
#40888 = DIRECTION ( 'NONE',  ( 0.000000000000000000, 0.000000000000000000, -1.000000000000000000 ) ) ;
#40889 = CARTESIAN_POINT ( 'NONE',  ( 12.20170062390598709, -19.39347807479101249, -1.500000000000002220 ) ) ;
#40890 = COORDINATED_UNIVERSAL_TIME_OFFSET ( 0, 0, .AHEAD. ) ;
#40891 = CARTESIAN_POINT ( 'NONE',  ( -31.55620429048339304, -24.66019654487198309, 8.947790411086138818 ) ) ;
#40892 = CARTESIAN_POINT ( 'NONE',  ( -2.791950601096355733, -5.876774720514417183, 20.17732409774492552 ) ) ;
#40893 = CARTESIAN_POINT ( 'NONE',  ( -17.82723130383223165, -9.322377578706960932, 11.49999999999999645 ) ) ;
#40894 = CARTESIAN_POINT ( 'NONE',  ( 3.787259615384621636, -5.876774720514405637, 18.51923076923076650 ) ) ;
#40895 = LINE ( 'NONE', #1843, #48434 ) ;
#40896 = PRODUCT_DEFINITION_SHAPE ( 'NONE', 'NONE',  #100428 ) ;
#40897 = PLANE ( 'NONE',  #84648 ) ;
#40898 = CARTESIAN_POINT ( 'NONE',  ( -129.5228709571500758, -29.50247984919015209, -1.443849546365044922 ) ) ;
#40899 = DIRECTION ( 'NONE',  ( -0.8246584009594635223, 0.5656310827093757876, 0.000000000000000000 ) ) ;
#40900 = CARTESIAN_POINT ( 'NONE',  ( -11.71124675921804403, 15.99993322257668282, -1.500000000000002220 ) ) ;
#40901 = CARTESIAN_POINT ( 'NONE',  ( 20.57166443188586769, -7.073620337204646447, -1.500000000000002220 ) ) ;
#40902 = DIRECTION ( 'NONE',  ( 0.000000000000000000, 0.000000000000000000, 1.000000000000000000 ) ) ;
#40903 = CARTESIAN_POINT ( 'NONE',  ( 16.84789977498956404, 10.09486508543780481, -1.500000000000002220 ) ) ;
#40904 = CARTESIAN_POINT ( 'NONE',  ( 15.77315497053730020, -4.795106742339615202, -28.11009842133895731 ) ) ;
#40905 = CARTESIAN_POINT ( 'NONE',  ( 0.000000000000000000, -4.132774720514426292, 0.000000000000000000 ) ) ;
#40906 = APPROVAL_ROLE ( '' ) ;
#40907 = AXIS2_PLACEMENT_3D ( 'NONE', #94677, #25670, #3360 ) ;
#40908 = DIRECTION ( 'NONE',  ( -1.000000000000000000, -3.773278334444166432E-23, -8.201307841325785021E-29 ) ) ;
#40909 = FACE_OUTER_BOUND ( 'NONE', #83145, .T. ) ;
#40910 = CARTESIAN_POINT ( 'NONE',  ( 19.85418835109896563, -5.301297255791479479, 11.49999999999999645 ) ) ;
#40911 = DIRECTION ( 'NONE',  ( 0.000000000000000000, -1.000000000000000000, 0.000000000000000000 ) ) ;
#40912 = FACE_OUTER_BOUND ( 'NONE', #3646, .T. ) ;
#40914 = EDGE_CURVE ( 'NONE', #67734, #88430, #67990, .T. ) ;
#40913 = CARTESIAN_POINT ( 'NONE',  ( -22.62345309801473547, -0.4825844212548152656, 11.49999999999999645 ) ) ;
#40915 = ORIENTED_EDGE ( 'NONE', *, *, #92835, .T. ) ;
#40916 = CARTESIAN_POINT ( 'NONE',  ( -115.5228709571500758, -25.00182538069145721, 7.747789668545101094 ) ) ;
#40918 = EDGE_CURVE ( 'NONE', #43471, #50604, #44147, .T. ) ;
#40917 = DIRECTION ( 'NONE',  ( 0.000000000000000000, 0.000000000000000000, 1.000000000000000000 ) ) ;
#40919 = CARTESIAN_POINT ( 'NONE',  ( -56.52287095715004739, -23.73907113216989018, -1.053371485793253459 ) ) ;
#40920 = CARTESIAN_POINT ( 'NONE',  ( -39.62287095715005592, -23.47593901973091235, -1.443836447539011525 ) ) ;
#40921 = B_SPLINE_CURVE_WITH_KNOTS ( 'NONE', 3,
 ( #84603, #70893, #47056, #94207, #70383, #38928 ),
 .UNSPECIFIED., .F., .F.,
 ( 4, 2, 4 ),
 ( 0.000000000000000000, 0.001380901958385379220, 0.002761803916770758441 ),
 .UNSPECIFIED. ) ;
#40922 = CARTESIAN_POINT ( 'NONE',  ( -26.59548113855183615, -24.61460036469634005, 7.895922928448310785 ) ) ;
#40923 = CARTESIAN_POINT ( 'NONE',  ( -28.52287095715006515, -23.57592831105002773, 11.05752276746862073 ) ) ;
#40924 = ORIENTED_EDGE ( 'NONE', *, *, #97141, .T. ) ;
#40925 = CIRCLE ( 'NONE', #6880, 2.350000000000000089 ) ;
#40926 = CARTESIAN_POINT ( 'NONE',  ( -79.80213995901898727, -25.31596255503136916, 5.120505554222577693 ) ) ;
#40927 = CARTESIAN_POINT ( 'NONE',  ( -12.33899560737860313, 19.21699747222852395, 11.49999999999998934 ) ) ;
#40928 = CARTESIAN_POINT ( 'NONE',  ( -110.8640811366819179, -25.20146121768474501, 3.413985529804576480 ) ) ;
#40929 = DIRECTION ( 'NONE',  ( -1.000000000000000000, 0.000000000000000000, 0.000000000000000000 ) ) ;
#40930 = CARTESIAN_POINT ( 'NONE',  ( -63.53934691136210944, -24.51419770103156992, 9.386484678747175181 ) ) ;
#40931 = LOCAL_TIME ( 0, 54, 15.00000000000000000, #27551 ) ;
#40932 = CARTESIAN_POINT ( 'NONE',  ( 17.90692129536829924, 13.62026984716248101, 11.49999999999999645 ) ) ;
#40933 = ORIENTED_EDGE ( 'NONE', *, *, #1046, .F. ) ;
#40934 = CARTESIAN_POINT ( 'NONE',  ( -33.55620429048340014, -23.48786465467240347, 11.44779295918255713 ) ) ;
#40935 = CARTESIAN_POINT ( 'NONE',  ( -16.59477544326466969, -14.39948450415919723, -1.500000000000002220 ) ) ;
#40936 = CARTESIAN_POINT ( 'NONE',  ( -127.1722404401672577, -25.37154127157531391, 4.079011290487088992 ) ) ;
#40937 = EDGE_CURVE ( 'NONE', #49847, #3669, #76077, .T. ) ;
#40938 = DIRECTION ( 'NONE',  ( 0.000000000000000000, -1.000000000000000000, 0.000000000000000000 ) ) ;
#40939 = CARTESIAN_POINT ( 'NONE',  ( -56.52287095715006870, -23.48786465467241058, 11.44779295918254824 ) ) ;
#40940 = VECTOR ( 'NONE', #14538, 1000.000000000000114 ) ;
#40941 = ORIENTED_EDGE ( 'NONE', *, *, #99918, .F. ) ;
#40942 = DIRECTION ( 'NONE',  ( -0.000000000000000000, 2.173523156925979552E-06, -0.9999999999976378895 ) ) ;
#40943 = DIRECTION ( 'NONE',  ( 0.000000000000000000, -0.000000000000000000, -1.000000000000000000 ) ) ;
#40944 = ORIENTED_EDGE ( 'NONE', *, *, #52810, .F. ) ;
#40945 = CARTESIAN_POINT ( 'NONE',  ( 18.57849760351508195, 8.651319581928444080, 11.49999999999998934 ) ) ;
#40946 = ORIENTED_EDGE ( 'NONE', *, *, #41009, .F. ) ;
#40947 = ORIENTED_EDGE ( 'NONE', *, *, #74359, .T. ) ;
#40948 = ORIENTED_EDGE ( 'NONE', *, *, #90786, .T. ) ;
#40949 = ORIENTED_EDGE ( 'NONE', *, *, #83388, .F. ) ;
#40950 = LINE ( 'NONE', #10999, #43675 ) ;
#40951 = CARTESIAN_POINT ( 'NONE',  ( -0.07435467474217070938, 23.09247799282200475, 11.49999999999998934 ) ) ;
#40952 = CARTESIAN_POINT ( 'NONE',  ( 27.53860345374808105, -1.682774720514426114, -1.272392034746785860 ) ) ;
#40953 = CARTESIAN_POINT ( 'NONE',  ( 9.809556900635294951, 17.81656380412256269, -1.500000000000002220 ) ) ;
#40954 = ORIENTED_EDGE ( 'NONE', *, *, #4427, .T. ) ;
#40955 = EDGE_CURVE ( 'NONE', #2649, #28831, #94231, .T. ) ;
#40956 = DIRECTION ( 'NONE',  ( -3.773278334453079618E-23, 0.9999999999976377785, 2.173523156925979975E-06 ) ) ;
#40957 = ADVANCED_FACE ( 'NONE', ( #30410 ), #83188, .T. ) ;
#40958 = CARTESIAN_POINT ( 'NONE',  ( -29.62375005554824980, -24.58464305241082215, 8.947790440257527678 ) ) ;
#40959 = ADVANCED_FACE ( 'NONE', ( #61379 ), #97914, .F. ) ;
#40960 = CARTESIAN_POINT ( 'NONE',  ( -101.4685450411434573, -25.22743938310598466, 6.465526456246802667 ) ) ;
#40961 = CARTESIAN_POINT ( 'NONE',  ( 4.593956459244529889, -5.876774720514410966, 19.29001220640957115 ) ) ;
#40963 = EDGE_LOOP ( 'NONE', ( #72929, #72274, #41363, #88597 ) ) ;
#40962 = CARTESIAN_POINT ( 'NONE',  ( -2.508422780830330989, 21.39056295969660582, 11.49999999999999645 ) ) ;
#40964 = CARTESIAN_POINT ( 'NONE',  ( -29.13856514152708499, -24.76881155732394646, 3.662309959797942049 ) ) ;
#40965 = CARTESIAN_POINT ( 'NONE',  ( -49.74369414166532977, -25.26385844215123910, 4.940878041311237645 ) ) ;
#40966 = EDGE_CURVE ( 'NONE', #84539, #93818, #93149, .T. ) ;
#40967 = ORIENTED_EDGE ( 'NONE', *, *, #58050, .F. ) ;
#40968 = CARTESIAN_POINT ( 'NONE',  ( -15.22196369898608737, 14.14466773073655581, -1.500000000000002220 ) ) ;
#40969 = VERTEX_POINT ( 'NONE', #53764 ) ;
#40971 = ORIENTED_EDGE ( 'NONE', *, *, #93990, .F. ) ;
#40970 = CARTESIAN_POINT ( 'NONE',  ( -91.55620429048340725, -24.64898659630528854, 1.056161002820825034 ) ) ;
#40972 = VECTOR ( 'NONE', #29267, 1000.000000000000114 ) ;
#40973 = B_SPLINE_SURFACE_WITH_KNOTS ( 'NONE', 3, 1, ( 
 ( #55635, #17050 ),
 ( #62752, #9437 ),
 ( #16539, #85058 ),
 ( #23653, #76935 ),
 ( #328, #55131 ),
 ( #39890, #78942 ),
 ( #93669, #38388 ),
 ( #48017, #86065 ),
 ( #24161, #47515 ),
 ( #7433, #69341 ),
 ( #85560, #78440 ),
 ( #54133, #71353 ),
 ( #15044, #92667 ),
 ( #8941, #30778 ),
 ( #15545, #100260 ),
 ( #1842, #54626 ),
 ( #40400, #70850 ),
 ( #16043, #61748 ),
 ( #47011, #59875 ) ),
 .UNSPECIFIED., .F., .F., .F.,
 ( 4, 1, 1, 1, 1, 1, 1, 1, 1, 1, 1, 1, 1, 1, 1, 1, 4 ),
 ( 2, 2 ),
 ( 0.000000000000000000, 0.06580764581069505070, 0.1293942736680568084, 0.1908940606321889999, 0.2512810689298332067, 0.3108149644652716814, 0.3703709874482468689, 0.4307682625897272244, 0.4928812506175027641, 0.5551039481552511035, 0.6160670509938424022, 0.6772560331746547702, 0.7382598051991177135, 0.8007621343762953980, 0.8647775815744849215, 0.9310452949994038052, 1.000000000000000000 ),
 ( 0.000000000000000000, 1.000000000000000000 ),
 .UNSPECIFIED. ) ;
#40974 = CARTESIAN_POINT ( 'NONE',  ( 5.641025641025643189, -6.376774720514420736, 20.78665865384615330 ) ) ;
#40975 = CARTESIAN_POINT ( 'NONE',  ( -51.92629526020853348, -25.26139929061960387, 6.040166309471107553 ) ) ;
#40976 = ORIENTED_EDGE ( 'NONE', *, *, #16638, .F. ) ;
#40977 = ORIENTED_EDGE ( 'NONE', *, *, #66812, .F. ) ;
#40978 = PLANE ( 'NONE',  #91515 ) ;
#40979 = CARTESIAN_POINT ( 'NONE',  ( -68.62287095715004170, -24.66019654487199020, 8.947790411086131712 ) ) ;
#40981 = ADVANCED_FACE ( 'NONE', ( #45152 ), #6575, .F. ) ;
#40980 = CARTESIAN_POINT ( 'NONE',  ( -29.76928132860276577, -25.21455316847251282, 4.017376845980065170 ) ) ;
#40982 = ADVANCED_FACE ( 'NONE', ( #60876 ), #59883, .T. ) ;
#40984 = EDGE_LOOP ( 'NONE', ( #76149, #23204, #41205, #1515 ) ) ;
#40983 = CARTESIAN_POINT ( 'NONE',  ( 12.33731239738771102, -18.22686410513083288, 11.49999999999999645 ) ) ;
#40985 = CARTESIAN_POINT ( 'NONE',  ( -103.5131199472542676, -24.34968618360933945, 0.1864209137778842229 ) ) ;
#40986 = CIRCLE ( 'NONE', #2099, 2.499999999999998668 ) ;
#40987 = CARTESIAN_POINT ( 'NONE',  ( -21.83012794225054165, -5.757306806698124113, 11.49999999999998934 ) ) ;
#40989 = ORIENTED_EDGE ( 'NONE', *, *, #39273, .F. ) ;
#40988 = PLANE ( 'NONE',  #55511 ) ;
#40990 = VECTOR ( 'NONE', #26552, 1000.000000000000114 ) ;
#40991 = EDGE_LOOP ( 'NONE', ( #30248, #55890, #19408, #46474 ) ) ;
#40992 = FACE_OUTER_BOUND ( 'NONE', #33764, .T. ) ;
#40993 = EDGE_CURVE ( 'NONE', #93421, #5378, #85704, .T. ) ;
#40994 = ADVANCED_FACE ( 'NONE', ( #9577 ), #9075, .T. ) ;
#40995 = LINE ( 'NONE', #71952, #95937 ) ;
#40996 = ORIENTED_EDGE ( 'NONE', *, *, #42191, .F. ) ;
#40997 = CARTESIAN_POINT ( 'NONE',  ( -0.2625952501129409367, 21.13516572482953748, -1.500000000000002220 ) ) ;
#40998 = CARTESIAN_POINT ( 'NONE',  ( -34.62287095715006302, -24.51387760970723662, 9.387446482453425389 ) ) ;
#40999 = CARTESIAN_POINT ( 'NONE',  ( -51.93149462243456327, -25.26040815178494725, 6.174051125736514045 ) ) ;
#41000 = CARTESIAN_POINT ( 'NONE',  ( -7.304748120944324796, -5.876774720514417183, 19.95463486386180563 ) ) ;
#41001 = CARTESIAN_POINT ( 'NONE',  ( -80.62287095715004170, -25.00182538069145721, 7.747789668545097541 ) ) ;
#41002 = CARTESIAN_POINT ( 'NONE',  ( -21.98633505697190671, -3.258044352128648846, -1.500000000000002220 ) ) ;
#41003 = DIRECTION ( 'NONE',  ( 0.000000000000000000, -0.7071067811865513475, 0.7071067811865437980 ) ) ;
#41004 = ADVANCED_FACE ( 'NONE', ( #78068 ), #17689, .F. ) ;
#41005 = ORIENTED_EDGE ( 'NONE', *, *, #66400, .F. ) ;
#41006 = CARTESIAN_POINT ( 'NONE',  ( -29.49875734969025842, -5.965225279485572685, 23.37402280011862743 ) ) ;
#41007 = CARTESIAN_POINT ( 'NONE',  ( 8.160000000000000142, -10.65233964170348635, -1.621096496867198589 ) ) ;
#41008 = CARTESIAN_POINT ( 'NONE',  ( 18.72033823704212097, 5.060218808788302880, 11.49999999999999645 ) ) ;
#41009 = EDGE_CURVE ( 'NONE', #36561, #6243, #37458, .T. ) ;
#41010 = CARTESIAN_POINT ( 'NONE',  ( -40.89642461179924737, -25.12242866868528068, 2.899885291263534892 ) ) ;
#41011 = CARTESIAN_POINT ( 'NONE',  ( -33.62287095715005592, -23.72773821059535493, 11.05748984161097503 ) ) ;
#41012 = VECTOR ( 'NONE', #64025, 1000.000000000000000 ) ;
#41013 = ADVANCED_FACE ( 'NONE', ( #55771 ), #16683, .F. ) ;
#41014 = CARTESIAN_POINT ( 'NONE',  ( -16.97169330436246781, 9.548981535075045102, -1.500000000000002220 ) ) ;
#41015 = CC_DESIGN_SECURITY_CLASSIFICATION ( #66951, ( #100428 ) ) ;
#41016 = CARTESIAN_POINT ( 'NONE',  ( 21.20698605602738951, -2.876969938318672870, 11.49999999999998934 ) ) ;
#41017 = CARTESIAN_POINT ( 'NONE',  ( -56.62287095715005592, -23.47593901973091235, -1.443836447539007972 ) ) ;
#41018 = CARTESIAN_POINT ( 'NONE',  ( -60.54474933874992360, -24.40133493613624083, 9.663955038888266458 ) ) ;
#41019 = CARTESIAN_POINT ( 'NONE',  ( -51.54738905035295460, -24.15543982623907127, -0.2315651400026664530 ) ) ;
#41020 = CARTESIAN_POINT ( 'NONE',  ( -77.59611061849884095, -23.96119346886880663, -0.6495511937832126881 ) ) ;
#41021 = CARTESIAN_POINT ( 'NONE',  ( -21.15473383059569557, 8.456223909384457116, -1.500000000000002220 ) ) ;
#41022 = VECTOR ( 'NONE', #92047, 1000.000000000000114 ) ;
#41023 = EDGE_CURVE ( 'NONE', #73483, #71054, #47168, .T. ) ;
#41024 = CARTESIAN_POINT ( 'NONE',  ( -106.5500282929658482, -24.51419770103158768, 9.386484678747164523 ) ) ;
#41025 = CARTESIAN_POINT ( 'NONE',  ( -20.27875734969026311, 7.743225279485574042, 24.00402280011862288 ) ) ;
#41026 = CARTESIAN_POINT ( 'NONE',  ( 1.158388978951967463, 19.79969207489630634, 11.49999999999999645 ) ) ;
#41027 = CARTESIAN_POINT ( 'NONE',  ( -123.5890674397278985, -24.51419770103158768, 9.386484678747160970 ) ) ;
#41028 = VECTOR ( 'NONE', #51727, 1000.000000000000114 ) ;
#41029 = CARTESIAN_POINT ( 'NONE',  ( -128.5228709571500758, -24.64965694238575722, 8.947790433994189385 ) ) ;
#41030 = CARTESIAN_POINT ( 'NONE',  ( -100.4326965455114902, -25.19502912051678578, 3.293943094755625633 ) ) ;
#41031 = VERTEX_POINT ( 'NONE', #24302 ) ;
#41032 = DIRECTION ( 'NONE',  ( 0.000000000000000000, 0.9999999999976377785, 2.173523156925979128E-06 ) ) ;
#41033 = CARTESIAN_POINT ( 'NONE',  ( -31.80982380344445204, -25.31558585043574183, 4.997857581739419075 ) ) ;
#41034 = FACE_OUTER_BOUND ( 'NONE', #56848, .T. ) ;
#41035 = CARTESIAN_POINT ( 'NONE',  ( 7.679218611123722837, 20.28660689097963399, 11.49999999999998934 ) ) ;
#41036 = CARTESIAN_POINT ( 'NONE',  ( -124.6228709571500559, -29.50247984919015209, -1.443849546365046699 ) ) ;
#41037 = CARTESIAN_POINT ( 'NONE',  ( -2.678125609936932605, 19.29598960679622976, -1.500000000000002220 ) ) ;
#41038 = FACE_OUTER_BOUND ( 'NONE', #30245, .T. ) ;
#41039 = VERTEX_POINT ( 'NONE', #48664 ) ;
#41040 = CARTESIAN_POINT ( 'NONE',  ( -15.93830457579706739, -12.76012858937699335, 11.49999999999999645 ) ) ;
#41041 = CARTESIAN_POINT ( 'NONE',  ( -49.55620429048338593, -23.47596703998600276, 11.44779298504227505 ) ) ;
#41042 = DIRECTION ( 'NONE',  ( -0.000000000000000000, -1.000000000000000000, -0.000000000000000000 ) ) ;
#41043 = ORIENTED_EDGE ( 'NONE', *, *, #4427, .F. ) ;
#41044 = CARTESIAN_POINT ( 'NONE',  ( -37.52287095715006870, -23.48786465467240347, 11.44779295918255180 ) ) ;
#41045 = CARTESIAN_POINT ( 'NONE',  ( 32.98371819488264833, 4.742969794006914874, -11.67826368001470172 ) ) ;
#41046 = CARTESIAN_POINT ( 'NONE',  ( 7.370931459274800090, -6.376774720514417183, 20.26286690110499578 ) ) ;
#41047 = PLANE ( 'NONE',  #24672 ) ;
#41048 = CARTESIAN_POINT ( 'NONE',  ( 2.100208336950355914, 0.000000000000000000, 0.000000000000000000 ) ) ;
#41049 = CARTESIAN_POINT ( 'NONE',  ( -93.62287095715005592, -29.50247984919015209, -1.443849546365051806 ) ) ;
#41050 = CIRCLE ( 'NONE', #39373, 4.450000000000000178 ) ;
#41051 = ORIENTED_EDGE ( 'NONE', *, *, #33075, .F. ) ;
#41052 = CARTESIAN_POINT ( 'NONE',  ( -66.63617261146598025, -24.15620529776628089, 10.23563542870660470 ) ) ;
#41053 = CARTESIAN_POINT ( 'NONE',  ( -22.63010559926462051, 4.001702944626347680, 11.49999999999999645 ) ) ;
#41054 = CARTESIAN_POINT ( 'NONE',  ( -7.854035805165779927, 21.33931789143995417, 11.49999999999998934 ) ) ;
#41055 = CARTESIAN_POINT ( 'NONE',  ( -110.5509673167211560, -24.63419186844610920, 9.035850630976920428 ) ) ;
#41056 = AXIS2_PLACEMENT_3D ( 'NONE', #9704, #71613, #2109 ) ;
#41057 = CARTESIAN_POINT ( 'NONE',  ( 33.61456970919605425, 3.316774720514426900, -11.35828564741663449 ) ) ;
#41058 = DIRECTION ( 'NONE',  ( -5.782411586589363555E-16, -1.000000000000000000, 0.000000000000000000 ) ) ;
#41059 = CARTESIAN_POINT ( 'NONE',  ( -82.52287095715001897, -23.48783264083388289, -1.443836473375923690 ) ) ;
#41060 = CARTESIAN_POINT ( 'NONE',  ( -11.13288495942205536, 18.84158392345546318, 11.49999999999998934 ) ) ;
#41061 = FACE_OUTER_BOUND ( 'NONE', #14131, .T. ) ;
#41062 = EDGE_CURVE ( 'NONE', #36448, #48203, #32921, .T. ) ;
#41063 = CARTESIAN_POINT ( 'NONE',  ( -49.68550546162367709, -25.31558437716839904, 4.971218732387883144 ) ) ;
#41064 = LINE ( 'NONE', #2506, #75987 ) ;
#41065 = CARTESIAN_POINT ( 'NONE',  ( -39.92287095715006018, -23.47593901973090169, -1.443836447538997980 ) ) ;
#41066 = ORIENTED_EDGE ( 'NONE', *, *, #32972, .T. ) ;
#41067 = ADVANCED_FACE ( 'NONE', ( #23794 ), #87892, .T. ) ;
#41068 = CARTESIAN_POINT ( 'NONE',  ( -20.33632446988539400, 1.880062042347348195, -1.500000000000002220 ) ) ;
#41069 = VERTEX_POINT ( 'NONE', #64399 ) ;
#41070 = EDGE_LOOP ( 'NONE', ( #57401, #7595, #15319, #60491 ) ) ;
#41071 = CARTESIAN_POINT ( 'NONE',  ( 22.26416322464526232, -5.798680748638591176, -1.500000000000002220 ) ) ;
#41072 = CARTESIAN_POINT ( 'NONE',  ( -8.160000000000000142, -0.4583917923827245389, 5.886156785137588443 ) ) ;
#41073 = EDGE_CURVE ( 'NONE', #74873, #71622, #23165, .T. ) ;
#41074 = VERTEX_POINT ( 'NONE', #49162 ) ;
#41075 = DIRECTION ( 'NONE',  ( 0.000000000000000000, 0.000000000000000000, 1.000000000000000000 ) ) ;
#41076 = ADVANCED_FACE ( 'NONE', ( #81592 ), #50148, .T. ) ;
#41077 = CARTESIAN_POINT ( 'NONE',  ( 26.73860345374794534, -5.356774720514427379, -3.111611894936215705 ) ) ;
#41078 = ADVANCED_FACE ( 'NONE', ( #41038 ), #89702, .F. ) ;
#41079 = B_SPLINE_CURVE_WITH_KNOTS ( 'NONE', 3,
 ( #959, #31911, #71985, #17177, #62884, #93803 ),
 .UNSPECIFIED., .F., .F.,
 ( 4, 2, 4 ),
 ( 0.005040430490715508416, 0.005640264188159228517, 0.006240097885602948619 ),
 .UNSPECIFIED. ) ;
#41080 = AXIS2_PLACEMENT_3D ( 'NONE', #11465, #18571, #89093 ) ;
#41081 = CARTESIAN_POINT ( 'NONE',  ( -35.52287095715006870, -24.99156044556120193, 7.747789690856173195 ) ) ;
#41082 = CARTESIAN_POINT ( 'NONE',  ( -27.96875734969026084, 6.376774720514426953, 0.7300228001186309656 ) ) ;
#41084 = ORIENTED_EDGE ( 'NONE', *, *, #29196, .F. ) ;
#41083 = CARTESIAN_POINT ( 'NONE',  ( -16.81368161134402683, 13.12552177539105358, 11.49999999999999645 ) ) ;
#41085 = ADVANCED_FACE ( 'NONE', ( #11077 ), #12063, .F. ) ;
#41086 = ORIENTED_EDGE ( 'NONE', *, *, #14028, .T. ) ;
#41087 = CARTESIAN_POINT ( 'NONE',  ( -11.95080204275630464, 18.75100984808165094, 11.49999999999998934 ) ) ;
#41088 = CARTESIAN_POINT ( 'NONE',  ( 18.87225196054570020, 8.368929400942139551, 11.49999999999998934 ) ) ;
#41090 = ORIENTED_EDGE ( 'NONE', *, *, #72506, .F. ) ;
#41089 = VECTOR ( 'NONE', #44288, 1000.000000000000000 ) ;
#41091 = CARTESIAN_POINT ( 'NONE',  ( -6.636054160061366503, -5.876774720514411854, 19.15289935703627933 ) ) ;
#41092 = CARTESIAN_POINT ( 'NONE',  ( -95.56281998239499842, -23.48786465467241058, 11.44779295918254469 ) ) ;
#41093 = VERTEX_POINT ( 'NONE', #42543 ) ;
#41094 = CARTESIAN_POINT ( 'NONE',  ( -79.58953762381672448, -23.48786465467241058, 11.44779295918254469 ) ) ;
#41095 = ORIENTED_EDGE ( 'NONE', *, *, #53140, .F. ) ;
#41096 = AXIS2_PLACEMENT_3D ( 'NONE', #54976, #48871, #9284 ) ;
#41097 = CARTESIAN_POINT ( 'NONE',  ( -58.52207410937929666, -23.48786465467241413, 11.44779295918254647 ) ) ;
#41098 = FACE_OUTER_BOUND ( 'NONE', #82768, .T. ) ;
#41099 = CARTESIAN_POINT ( 'NONE',  ( 8.688630223215852766, -18.96179456382524364, -1.500000000000002220 ) ) ;
#41100 = EDGE_CURVE ( 'NONE', #15238, #47938, #79586, .T. ) ;
#41101 = CARTESIAN_POINT ( 'NONE',  ( -21.47987282208850601, -4.139150239982721580, 11.49999999999999645 ) ) ;
#41102 = CARTESIAN_POINT ( 'NONE',  ( -26.64126777428346315, -24.89279892862556665, 7.094643926469543338 ) ) ;
#41103 = LINE ( 'NONE', #72058, #27269 ) ;
#41104 = CARTESIAN_POINT ( 'NONE',  ( 21.70358988458699301, 5.938112137899119070, -1.500000000000002220 ) ) ;
#41105 = CARTESIAN_POINT ( 'NONE',  ( 0.8369575198195864374, -20.89415947959451003, 11.49999999999998934 ) ) ;
#41106 = CARTESIAN_POINT ( 'NONE',  ( -38.54597331675388716, -24.15543982623907127, -0.2315651400026569606 ) ) ;
#41107 = CARTESIAN_POINT ( 'NONE',  ( -44.52287095715006160, -23.47596703998600631, 11.44779298504229281 ) ) ;
#41108 = DIRECTION ( 'NONE',  ( -7.960204194457801640E-17, -1.000000000000000000, 0.000000000000000000 ) ) ;
#41110 = VERTEX_POINT ( 'NONE', #65891 ) ;
#41109 = EDGE_CURVE ( 'NONE', #18484, #67714, #87946, .T. ) ;
#41111 = EDGE_LOOP ( 'NONE', ( #54200, #68771, #92714, #34950 ) ) ;
#41112 = ORIENTED_EDGE ( 'NONE', *, *, #13517, .T. ) ;
#41113 = CARTESIAN_POINT ( 'NONE',  ( -99.29687923781919778, -25.26221111348665005, 6.149712179509984722 ) ) ;
#41114 = ORIENTED_EDGE ( 'NONE', *, *, #64057, .T. ) ;
#41115 = CARTESIAN_POINT ( 'NONE',  ( 20.27498964588844643, 6.839650151297337999, -1.500000000000002220 ) ) ;
#41116 = CARTESIAN_POINT ( 'NONE',  ( 8.126467401150291536, 20.86698325809501497, 11.49999999999999645 ) ) ;
#41117 = EDGE_LOOP ( 'NONE', ( #14715, #8006, #11003, #46558 ) ) ;
#41118 = CARTESIAN_POINT ( 'NONE',  ( -59.52287095715004028, -24.34917612406836795, 0.1852690917426535466 ) ) ;
#41119 = CARTESIAN_POINT ( 'NONE',  ( -17.44821286160079410, -11.81026508430653088, 11.49999999999998934 ) ) ;
#41120 = CARTESIAN_POINT ( 'NONE',  ( -61.52287095715007581, -23.47593901973090169, -1.443836447538997092 ) ) ;
#41121 = CARTESIAN_POINT ( 'NONE',  ( -1.646307629438301667, 19.86461321233117872, -1.500000000000002220 ) ) ;
#41122 = CARTESIAN_POINT ( 'NONE',  ( -50.62889347931399442, -24.83644354573578283, 8.397322867130100121 ) ) ;
#41123 = B_SPLINE_CURVE_WITH_KNOTS ( 'NONE', 3,
 ( #9690, #93917, #64008, #56388, #24409, #17808, #55376, #86311 ),
 .UNSPECIFIED., .F., .F.,
 ( 4, 2, 2, 4 ),
 ( 0.000000000000000000, 0.002001098010032691023, 0.003001647015049036318, 0.004002196020065382047 ),
 .UNSPECIFIED. ) ;
#41124 = CARTESIAN_POINT ( 'NONE',  ( -80.39981004835770761, -25.29534345565997100, 4.506608245854094363 ) ) ;
#41125 = CARTESIAN_POINT ( 'NONE',  ( -20.87105610827876134, -7.033761084331515256, -1.500000000000002220 ) ) ;
#41126 = ORIENTED_EDGE ( 'NONE', *, *, #44790, .F. ) ;
#41127 = CARTESIAN_POINT ( 'NONE',  ( -116.6298663670893632, -23.48783264082478439, -1.443836473390061936 ) ) ;
#41128 = TOROIDAL_SURFACE ( 'NONE', #31332, 80.18232118519038920, 8.160000000000000142 ) ;
#41129 = FACE_OUTER_BOUND ( 'NONE', #42581, .T. ) ;
#41130 = CARTESIAN_POINT ( 'NONE',  ( -78.62287095715007013, -24.51387760970723662, 9.387446482453411178 ) ) ;
#41131 = EDGE_CURVE ( 'NONE', #37466, #75118, #49508, .T. ) ;
#41132 = CARTESIAN_POINT ( 'NONE',  ( -26.95579990879923926, -24.88473778148743065, 7.214475432169975555 ) ) ;
#41133 = B_SPLINE_CURVE_WITH_KNOTS ( 'NONE', 3,
 ( #2355, #87584, #18066, #10449 ),
 .UNSPECIFIED., .F., .F.,
 ( 4, 4 ),
 ( 0.000000000000000000, 9.999999999998900014E-05 ),
 .UNSPECIFIED. ) ;
#41134 = VECTOR ( 'NONE', #62290, 1000.000000000000114 ) ;
#41135 = CARTESIAN_POINT ( 'NONE',  ( 0.3244565263465140070, -1.558659884777350513, 8.999999999999978684 ) ) ;
#41136 = CARTESIAN_POINT ( 'NONE',  ( -117.5228709571500758, -23.48783264082477729, -1.443836473390083697 ) ) ;
#41137 = CARTESIAN_POINT ( 'NONE',  ( -20.89022842043660688, 4.291957016416017900, -1.500000000000002220 ) ) ;
#41138 = CARTESIAN_POINT ( 'NONE',  ( -70.27422298781921484, -25.31465149953924865, 4.851635142449610250 ) ) ;
#41139 = PLANE ( 'NONE',  #36764 ) ;
#41140 = EDGE_CURVE ( 'NONE', #80103, #1680, #89204, .T. ) ;
#41141 = CARTESIAN_POINT ( 'NONE',  ( -85.62287095715004170, -29.50248789122583659, 2.256150453626215580 ) ) ;
#41142 = CARTESIAN_POINT ( 'NONE',  ( -80.60605223983722567, -25.12374756684099353, 7.097317179231969142 ) ) ;
#41143 = CARTESIAN_POINT ( 'NONE',  ( -13.16310354753345990, -18.33534949228788236, -1.500000000000002220 ) ) ;
#41144 = CARTESIAN_POINT ( 'NONE',  ( -40.94687764114259920, -25.04307374350000259, 7.563175304812659761 ) ) ;
#41145 = ORIENTED_EDGE ( 'NONE', *, *, #96959, .F. ) ;
#41146 = FACE_OUTER_BOUND ( 'NONE', #83174, .T. ) ;
#41147 = CARTESIAN_POINT ( 'NONE',  ( 7.981902603654314809, -10.32819234916652640, 1.310587897985987738 ) ) ;
#41148 = CARTESIAN_POINT ( 'NONE',  ( -19.67010641940559168, 0.002901314006966619011, 11.49999999999999645 ) ) ;
#41149 = DIRECTION ( 'NONE',  ( 0.000000000000000000, 0.000000000000000000, 1.000000000000000000 ) ) ;
#41150 = CARTESIAN_POINT ( 'NONE',  ( 14.67302116299744519, -4.477500275188337930, -27.99481486150953558 ) ) ;
#41151 = VERTEX_POINT ( 'NONE', #2982 ) ;
#41152 = CARTESIAN_POINT ( 'NONE',  ( -99.52218633031425554, -23.48783264082478439, -1.443836473390063047 ) ) ;
#41153 = DIRECTION ( 'NONE',  ( -0.000000000000000000, 1.000000000000000000, -0.000000000000000000 ) ) ;
#41154 = CARTESIAN_POINT ( 'NONE',  ( -124.5899953110402549, -24.15620529776629510, 10.23563542870659404 ) ) ;
#41155 = CARTESIAN_POINT ( 'NONE',  ( -88.55620429048339304, -23.47593901973091235, -1.443836447539002865 ) ) ;
#41156 = CARTESIAN_POINT ( 'NONE',  ( 22.02124265030973760, 6.143225279485574397, 16.20402280011862217 ) ) ;
#41157 = CARTESIAN_POINT ( 'NONE',  ( -64.62287095715005592, -29.50248528299804818, 1.056150453629034924 ) ) ;
#41158 = CARTESIAN_POINT ( 'NONE',  ( -9.637476322613308000, -17.25261889746210997, 11.49999999999998934 ) ) ;
#41159 = ORIENTED_EDGE ( 'NONE', *, *, #35756, .T. ) ;
#41160 = CARTESIAN_POINT ( 'NONE',  ( 12.02422309597069017, 16.21794576832014556, 11.49999999999999645 ) ) ;
#41161 = CARTESIAN_POINT ( 'NONE',  ( -112.6228709571501128, -23.96177878511308634, 10.65340807706329684 ) ) ;
#41162 = ORIENTED_EDGE ( 'NONE', *, *, #62866, .T. ) ;
#41163 = DIRECTION ( 'NONE',  ( -0.02119372647572909107, 0.000000000000000000, -0.9997753877537054468 ) ) ;
#41164 = FACE_OUTER_BOUND ( 'NONE', #5155, .T. ) ;
#41165 = CARTESIAN_POINT ( 'NONE',  ( -100.3784397666924804, -25.26638541110039426, 7.561116734059481814 ) ) ;
#41166 = DIRECTION ( 'NONE',  ( -3.773278334453079618E-23, 0.9999999999976377785, 2.173523156925979975E-06 ) ) ;
#41167 = FACE_OUTER_BOUND ( 'NONE', #65565, .T. ) ;
#41168 = CARTESIAN_POINT ( 'NONE',  ( -33.58953762381672448, -23.48783264082477373, -1.443836473390074371 ) ) ;
#41169 = CARTESIAN_POINT ( 'NONE',  ( -17.62595516807937557, -9.487554784798948759, -1.500000000000002220 ) ) ;
#41170 = B_SPLINE_CURVE_WITH_KNOTS ( 'NONE', 3,
 ( #54871, #79192, #85811, #41150, #79692, #8691, #16291, #39631, #48260, #70 ),
 .UNSPECIFIED., .F., .F.,
 ( 4, 2, 2, 2, 4 ),
 ( 0.000000000000000000, 0.0004686948575969757699, 0.0009373897151939515398, 0.001406084572790927256, 0.001874779430387901779 ),
 .UNSPECIFIED. ) ;
#41171 = CARTESIAN_POINT ( 'NONE',  ( -58.62287095715002039, -23.94994826722515668, -0.6494450866351725304 ) ) ;
#41172 = EDGE_LOOP ( 'NONE', ( #57851, #80506, #91230, #25000 ) ) ;
#41173 = B_SPLINE_CURVE_WITH_KNOTS ( 'NONE', 3,
 ( #74481, #35920, #59774, #43543, #20685, #45046 ),
 .UNSPECIFIED., .F., .F.,
 ( 4, 2, 4 ),
 ( 0.000000000000000000, 0.001380764517853250335, 0.002761529035706500670 ),
 .UNSPECIFIED. ) ;
#41174 = CARTESIAN_POINT ( 'NONE',  ( -24.90875734969025501, 6.475225279485573360, 30.00402280011862288 ) ) ;
#41175 = CARTESIAN_POINT ( 'NONE',  ( -52.62287095715005592, -29.50248528299804818, 1.056150453629033370 ) ) ;
#41176 = CARTESIAN_POINT ( 'NONE',  ( -63.52287095715006160, -24.64965694238575011, 8.947790433994201820 ) ) ;
#41177 = CARTESIAN_POINT ( 'NONE',  ( -124.6228709571500417, -24.65952944569304606, 1.056160979905705011 ) ) ;
#41178 = CARTESIAN_POINT ( 'NONE',  ( -73.49610432738134591, -24.65952944569304606, 1.056160979905700126 ) ) ;
#41179 = CARTESIAN_POINT ( 'NONE',  ( -45.62287095715004881, -23.47596703998600276, 11.44779298504227505 ) ) ;
#41180 = ADVANCED_FACE ( 'NONE', ( #33916 ), #57279, .T. ) ;
#41181 = CARTESIAN_POINT ( 'NONE',  ( -100.9369564999036157, -25.31392319263090229, 5.203681702801227438 ) ) ;
#41182 = ORIENTED_EDGE ( 'NONE', *, *, #83324, .T. ) ;
#41183 = ADVANCED_FACE ( 'NONE', ( #49653 ), #80586, .F. ) ;
#41184 = CARTESIAN_POINT ( 'NONE',  ( 9.670762957215185196, 17.83519281925787325, 11.49999999999998934 ) ) ;
#41185 = VERTEX_POINT ( 'NONE', #96314 ) ;
#41186 = CARTESIAN_POINT ( 'NONE',  ( 31.63910543787539709, 6.180494461685818841, 27.51903215948834358 ) ) ;
#41187 = CIRCLE ( 'NONE', #83255, 1.000000000000000222 ) ;
#41188 = EDGE_CURVE ( 'NONE', #22271, #69136, #96056, .T. ) ;
#41189 = CARTESIAN_POINT ( 'NONE',  ( -127.5219658841072174, -23.73791477778912551, 11.05961554403169167 ) ) ;
#41190 = CARTESIAN_POINT ( 'NONE',  ( -105.6228709571501128, -24.52232992886363760, 0.6492154411906164713 ) ) ;
#41191 = EDGE_CURVE ( 'NONE', #88647, #34088, #45033, .T. ) ;
#41192 = DIRECTION ( 'NONE',  ( -0.000000000000000000, 1.000000000000000000, -0.000000000000000000 ) ) ;
#41194 = DIRECTION ( 'NONE',  ( 0.000000000000000000, 0.000000000000000000, -1.000000000000000000 ) ) ;
#41193 = AXIS2_PLACEMENT_3D ( 'NONE', #68648, #84857, #15337 ) ;
#41195 = EDGE_CURVE ( 'NONE', #77364, #24634, #60475, .T. ) ;
#41196 = CARTESIAN_POINT ( 'NONE',  ( -13.65698368949537311, 16.12507722524849996, 11.49999999999999645 ) ) ;
#41197 = CARTESIAN_POINT ( 'NONE',  ( 8.970247382295582383, 20.24485829007567617, -1.500000000000002220 ) ) ;
#41198 = EDGE_CURVE ( 'NONE', #65732, #94122, #84744, .T. ) ;
#41199 = CARTESIAN_POINT ( 'NONE',  ( -9.016818060619870678, -18.48156098877705844, -1.500000000000002220 ) ) ;
#41200 = ORIENTED_EDGE ( 'NONE', *, *, #3031, .T. ) ;
#41201 = FACE_OUTER_BOUND ( 'NONE', #35337, .T. ) ;
#41202 = ORIENTED_EDGE ( 'NONE', *, *, #90589, .F. ) ;
#41203 = CARTESIAN_POINT ( 'NONE',  ( 4.784292611718076849, -5.356774720514425603, -25.54547254883186014 ) ) ;
#41204 = DIRECTION ( 'NONE',  ( 1.000000000000000000, 3.773278334444166432E-23, 8.201307841325785021E-29 ) ) ;
#41205 = ORIENTED_EDGE ( 'NONE', *, *, #49916, .T. ) ;
#41206 = B_SPLINE_CURVE_WITH_KNOTS ( 'NONE', 3,
 ( #86131, #78503, #9507, #16607 ),
 .UNSPECIFIED., .F., .F.,
 ( 4, 4 ),
 ( 0.000000000000000000, 9.999999999998897304E-05 ),
 .UNSPECIFIED. ) ;
#41207 = ORIENTED_EDGE ( 'NONE', *, *, #9367, .F. ) ;
#41208 = ORIENTED_EDGE ( 'NONE', *, *, #26970, .T. ) ;
#41209 = CARTESIAN_POINT ( 'NONE',  ( -111.5947439173848466, -25.23257392120766340, 3.581186434512583450 ) ) ;
#41210 = CARTESIAN_POINT ( 'NONE',  ( 6.792576760808763936, -5.876774720514415407, 20.16775508794004779 ) ) ;
#41211 = CARTESIAN_POINT ( 'NONE',  ( 5.443272695963705665, -6.376774720514417183, 20.27301970143225418 ) ) ;
#41212 = CARTESIAN_POINT ( 'NONE',  ( -0.2510023010970363067, -20.70922355669356563, -1.500000000000002220 ) ) ;
#41213 = B_SPLINE_CURVE_WITH_KNOTS ( 'NONE', 3,
 ( #20644, #59732, #48751, #82549, #72582, #36380, #52112, #42144, #98766, #29260, #80184, #96408, #13527, #90663, #2569, #13029, #74924, #87289, #56868, #80682, #73084, #49258 ),
 .UNSPECIFIED., .F., .F.,
 ( 4, 2, 2, 2, 2, 2, 2, 2, 2, 2, 4 ),
 ( 2.168404344971008627E-19, 0.0002785781587267594124, 0.0005571563174535186080, 0.001114312634907036999, 0.001392890793633791858, 0.001671468952360546717, 0.002228625269814061421, 0.002785781587267576343, 0.003342937904721091265, 0.003900094222174607054, 0.004457250539628123710 ),
 .UNSPECIFIED. ) ;
#41214 = CARTESIAN_POINT ( 'NONE',  ( -5.395268184683536639, 21.00466093859614958, 11.49999999999999645 ) ) ;
#41215 = ORIENTED_EDGE ( 'NONE', *, *, #37057, .F. ) ;
#41216 = CARTESIAN_POINT ( 'NONE',  ( -60.52287095715002607, -24.63345952396938898, 9.038047939281669940 ) ) ;
#41217 = CARTESIAN_POINT ( 'NONE',  ( 9.315600972258346602, -5.965225279485572685, 28.35070303307545458 ) ) ;
#41218 = CARTESIAN_POINT ( 'NONE',  ( 14.42577177192597482, -17.14957960503723911, 11.49999999999998934 ) ) ;
#41219 = CARTESIAN_POINT ( 'NONE',  ( -15.87499999999997868, 0.000000000000000000, 0.000000000000000000 ) ) ;
#41220 = FACE_OUTER_BOUND ( 'NONE', #48579, .T. ) ;
#41221 = EDGE_LOOP ( 'NONE', ( #78123, #23543 ) ) ;
#41222 = CARTESIAN_POINT ( 'NONE',  ( 29.64418490232317893, 5.621712738193696879, 28.18100406333994457 ) ) ;
#41223 = CARTESIAN_POINT ( 'NONE',  ( -35.50851531642891956, -23.85049219812685095, 10.88485053497527488 ) ) ;
#41224 = ORIENTED_EDGE ( 'NONE', *, *, #84330, .T. ) ;
#41225 = VERTEX_POINT ( 'NONE', #44525 ) ;
#41226 = CARTESIAN_POINT ( 'NONE',  ( -67.52209873245003280, -23.48786465467241058, 11.44779295918254824 ) ) ;
#41227 = ORIENTED_EDGE ( 'NONE', *, *, #74619, .F. ) ;
#41228 = CARTESIAN_POINT ( 'NONE',  ( -80.52287095715006160, -29.50250243563736774, 8.947779886222141599 ) ) ;
#41229 = CARTESIAN_POINT ( 'NONE',  ( 7.950249384483326409, 19.69624408967213469, -1.500000000000002220 ) ) ;
#41230 = ORIENTED_EDGE ( 'NONE', *, *, #20946, .T. ) ;
#41231 = CARTESIAN_POINT ( 'NONE',  ( -68.62287095715008434, -23.96127896941632329, -0.6493128931037843721 ) ) ;
#41232 = CARTESIAN_POINT ( 'NONE',  ( -18.37375256118794553, 11.78967355450649457, -1.500000000000002220 ) ) ;
#41233 = CARTESIAN_POINT ( 'NONE',  ( -103.5888923157342276, -24.35071581493543391, 9.817618358456027039 ) ) ;
#41234 = FACE_OUTER_BOUND ( 'NONE', #13225, .T. ) ;
#41235 = CARTESIAN_POINT ( 'NONE',  ( -128.6228709571500417, -29.50248528299804818, 1.056150453629047137 ) ) ;
#41236 = CARTESIAN_POINT ( 'NONE',  ( -4.983756199382824548, -21.29032736245130053, -1.500000000000002220 ) ) ;
#41237 = CARTESIAN_POINT ( 'NONE',  ( 6.944081373883786767, -5.876774720514423400, 21.27829155525578031 ) ) ;
#41238 = ORIENTED_EDGE ( 'NONE', *, *, #93985, .T. ) ;
#41239 = LINE ( 'NONE', #87912, #56748 ) ;
#41240 = CARTESIAN_POINT ( 'NONE',  ( -48.89385731722059347, -25.12782558666062371, 6.392749237613702284 ) ) ;
#41241 = VERTEX_POINT ( 'NONE', #14053 ) ;
#41242 = VERTEX_POINT ( 'NONE', #67368 ) ;
#41243 = LINE ( 'NONE', #44243, #70816 ) ;
#41244 = ORIENTED_EDGE ( 'NONE', *, *, #73444, .F. ) ;
#41245 = CARTESIAN_POINT ( 'NONE',  ( -46.62287095715004881, -29.50248528299804818, 1.056150453629033370 ) ) ;
#41246 = CARTESIAN_POINT ( 'NONE',  ( -113.6228709571500559, -23.73907113216990794, -1.053371485793225260 ) ) ;
#41247 = CARTESIAN_POINT ( 'NONE',  ( 10.86157628581156764, 18.25448884030880592, 11.49999999999998934 ) ) ;
#41248 = CARTESIAN_POINT ( 'NONE',  ( -71.20541289166536103, -29.50249360700573931, 4.885880847770192048 ) ) ;
#41249 = CARTESIAN_POINT ( 'NONE',  ( -40.85509569547110686, -25.19765059099818671, 6.732792336238610176 ) ) ;
#41250 = ADVANCED_FACE ( 'NONE', ( #29290 ), #68856, .F. ) ;
#41251 = VECTOR ( 'NONE', #73610, 1000.000000000000114 ) ;
#41252 = DIRECTION ( 'NONE',  ( -0.000000000000000000, 2.173523156925979552E-06, -0.9999999999976378895 ) ) ;
#41253 = LINE ( 'NONE', #17912, #32980 ) ;
#41254 = CARTESIAN_POINT ( 'NONE',  ( -18.22486019313910077, 6.713856318530649681, -1.500000000000002220 ) ) ;
#41255 = EDGE_CURVE ( 'NONE', #73282, #32756, #51136, .T. ) ;
#41256 = CARTESIAN_POINT ( 'NONE',  ( -45.62923331240457969, -24.83618233451450408, 1.606449574219532384 ) ) ;
#41257 = VERTEX_POINT ( 'NONE', #91184 ) ;
#41258 = CARTESIAN_POINT ( 'NONE',  ( 5.544562197198338538, -18.70016399976332977, 11.49999999999999645 ) ) ;
#41259 = CARTESIAN_POINT ( 'NONE',  ( -5.568927889719891944, -5.876774720514415407, 20.14881673916291760 ) ) ;
#41260 = CARTESIAN_POINT ( 'NONE',  ( -80.41358636250679126, -25.12334935364737376, 7.099569252745908443 ) ) ;
#41261 = ORIENTED_EDGE ( 'NONE', *, *, #75336, .F. ) ;
#41262 = VECTOR ( 'NONE', #95354, 1000.000000000000114 ) ;
#41263 = CARTESIAN_POINT ( 'NONE',  ( 8.971512145086530055, -9.528487854913503696, 3.755316172059227273E-16 ) ) ;
#41264 = CARTESIAN_POINT ( 'NONE',  ( -75.62287095715007013, -24.92579138211019796, 1.929029949965668234 ) ) ;
#41265 = FACE_OUTER_BOUND ( 'NONE', #32692, .T. ) ;
#41266 = CARTESIAN_POINT ( 'NONE',  ( -80.55728237399675606, -25.24813991124032952, 7.562285528293593906 ) ) ;
#41267 = CARTESIAN_POINT ( 'NONE',  ( 18.24227566675094181, -7.298356753547692755, 11.49999999999998934 ) ) ;
#41268 = ORIENTED_EDGE ( 'NONE', *, *, #37654, .T. ) ;
#41269 = CARTESIAN_POINT ( 'NONE',  ( -97.52287095715006160, -29.50250786944525672, 11.44777988621623166 ) ) ;
#41270 = CARTESIAN_POINT ( 'NONE',  ( -59.52287095715006160, -23.48783264082477018, -1.443836473390095021 ) ) ;
#41271 = PERSON_AND_ORGANIZATION ( #70597, #27821 ) ;
#41272 = CARTESIAN_POINT ( 'NONE',  ( 3.448102555317568374, -6.376774720514424288, 21.39871091031772110 ) ) ;
#41273 = DIRECTION ( 'NONE',  ( 0.000000000000000000, 1.000000000000000000, 0.000000000000000000 ) ) ;
#41274 = CARTESIAN_POINT ( 'NONE',  ( -115.6228709571499991, -24.83620972994592435, 8.398175272781360334 ) ) ;
#41275 = CARTESIAN_POINT ( 'NONE',  ( -97.55489214582006241, -23.96169478059713853, 10.65365249895717703 ) ) ;
#41276 = CARTESIAN_POINT ( 'NONE',  ( -94.62287095715005592, -23.48783264082478794, -1.443836473390063491 ) ) ;
#41277 = CARTESIAN_POINT ( 'NONE',  ( 5.654014271574485662, -6.376774720514420736, 20.92503208403226722 ) ) ;
#41278 = FACE_OUTER_BOUND ( 'NONE', #65365, .T. ) ;
#41279 = LINE ( 'NONE', #41795, #55927 ) ;
#41280 = CARTESIAN_POINT ( 'NONE',  ( -7.573260116017839216, 18.43532004384545786, -1.500000000000002220 ) ) ;
#41281 = CARTESIAN_POINT ( 'NONE',  ( -75.55895386407497938, -23.85049219812685806, 10.88485053497527488 ) ) ;
#41282 = CARTESIAN_POINT ( 'NONE',  ( -13.56193660873917395, -14.51407242162769151, -1.500000000000002220 ) ) ;
#41283 = EDGE_LOOP ( 'NONE', ( #44180, #51633, #29328, #30462 ) ) ;
#41284 = DIRECTION ( 'NONE',  ( 0.000000000000000000, -0.9999999999976377785, -2.173523156925979128E-06 ) ) ;
#41285 = CARTESIAN_POINT ( 'NONE',  ( -25.92875734969025814, 3.316774720514426456, 26.43402280011862615 ) ) ;
#41286 = CARTESIAN_POINT ( 'NONE',  ( 8.160000000000000142, -10.15233964170348457, 0.003711184059992174607 ) ) ;
#41287 = AXIS2_PLACEMENT_3D ( 'NONE', #91045, #29646, #36768 ) ;
#41288 = LINE ( 'NONE', #33677, #13514 ) ;
#41289 = CARTESIAN_POINT ( 'NONE',  ( 19.40640353424967302, -7.489167304209242815, 11.49999999999999645 ) ) ;
#41290 = FACE_OUTER_BOUND ( 'NONE', #22232, .T. ) ;
#41291 = LINE ( 'NONE', #97569, #74524 ) ;
#41292 = CARTESIAN_POINT ( 'NONE',  ( 22.50852769316577096, -3.342225187595919689, 11.49999999999999645 ) ) ;
#41293 = ORIENTED_EDGE ( 'NONE', *, *, #90786, .F. ) ;
#41294 = LINE ( 'NONE', #89468, #91616 ) ;
#41295 = FACE_OUTER_BOUND ( 'NONE', #75893, .T. ) ;
#41296 = ORIENTED_EDGE ( 'NONE', *, *, #76573, .F. ) ;
#41297 = ADVANCED_FACE ( 'NONE', ( #37905 ), #75952, .T. ) ;
#41298 = B_SPLINE_CURVE_WITH_KNOTS ( 'NONE', 3,
 ( #66901, #97331, #27819, #42566 ),
 .UNSPECIFIED., .F., .F.,
 ( 4, 4 ),
 ( 2.775557561562891351E-17, 0.0001000000000000167286 ),
 .UNSPECIFIED. ) ;
#41299 = CARTESIAN_POINT ( 'NONE',  ( -18.67835518149133378, -7.740158416121700746, -1.500000000000002220 ) ) ;
#41300 = DIRECTION ( 'NONE',  ( 3.773278334444166432E-23, -1.000000000000000000, 0.000000000000000000 ) ) ;
#41301 = CARTESIAN_POINT ( 'NONE',  ( -40.67156841055674477, -25.30545518805434568, 5.059772659950606766 ) ) ;
#41302 = EDGE_CURVE ( 'NONE', #23301, #1643, #91891, .T. ) ;
#41303 = CARTESIAN_POINT ( 'NONE',  ( -100.6228709571500559, -24.83602698348162008, 1.605859176311265735 ) ) ;
#41304 = EDGE_CURVE ( 'NONE', #84489, #39077, #30282, .T. ) ;
#41305 = VERTEX_POINT ( 'NONE', #90194 ) ;
#41306 = PLANE ( 'NONE',  #58251 ) ;
#41307 = CARTESIAN_POINT ( 'NONE',  ( -10.32858501761201353, 6.295917116278983983, 28.25808420984930791 ) ) ;
#41308 = CARTESIAN_POINT ( 'NONE',  ( -4.560224734120114753, 19.45435480350565882, -1.500000000000002220 ) ) ;
#41309 = EDGE_CURVE ( 'NONE', #99816, #28831, #84072, .T. ) ;
#41310 = CARTESIAN_POINT ( 'NONE',  ( -8.674659061502078217, -19.08593140856894621, 11.49999999999999645 ) ) ;
#41311 = CARTESIAN_POINT ( 'NONE',  ( -27.89254357189496858, -24.66661246132309415, 8.246170428369305583 ) ) ;
#41312 = FACE_OUTER_BOUND ( 'NONE', #85867, .T. ) ;
#41313 = CARTESIAN_POINT ( 'NONE',  ( 18.76863814860013235, 11.56883167669432133, -1.500000000000002220 ) ) ;
#41314 = EDGE_CURVE ( 'NONE', #6893, #70136, #82577, .T. ) ;
#41315 = AXIS2_PLACEMENT_3D ( 'NONE', #50788, #83216, #28937 ) ;
#41316 = CARTESIAN_POINT ( 'NONE',  ( 7.117251336872616463, 5.324156306579707731, -25.56604299071238984 ) ) ;
#41317 = ORIENTED_EDGE ( 'NONE', *, *, #89217, .T. ) ;
#41318 = CARTESIAN_POINT ( 'NONE',  ( -47.62287095715004170, -24.65952944569304250, 1.056160979905693686 ) ) ;
#41319 = FACE_OUTER_BOUND ( 'NONE', #20706, .T. ) ;
#41320 = DIRECTION ( 'NONE',  ( -3.773278334444166432E-23, 1.000000000000000000, 0.000000000000000000 ) ) ;
#41321 = ORIENTED_EDGE ( 'NONE', *, *, #90444, .T. ) ;
#41322 = CARTESIAN_POINT ( 'NONE',  ( -123.6228709571500275, -23.95044443724991012, 10.65354141964650125 ) ) ;
#41323 = ORIENTED_EDGE ( 'NONE', *, *, #70885, .T. ) ;
#41324 = ORIENTED_EDGE ( 'NONE', *, *, #86346, .T. ) ;
#41325 = PLANE ( 'NONE',  #37232 ) ;
#41326 = DIRECTION ( 'NONE',  ( 3.773278334444167608E-23, -1.000000000000000000, 0.000000000000000000 ) ) ;
#41328 = EDGE_CURVE ( 'NONE', #21186, #42265, #82086, .T. ) ;
#41327 = CARTESIAN_POINT ( 'NONE',  ( -94.62287095715009855, -24.33927499327855415, 9.819080762295811837 ) ) ;
#41329 = CARTESIAN_POINT ( 'NONE',  ( 20.13950599927006735, 4.067174238878714654, -1.500000000000002220 ) ) ;
#41330 = VECTOR ( 'NONE', #80033, 1000.000000000000000 ) ;
#41331 = ORIENTED_EDGE ( 'NONE', *, *, #15175, .F. ) ;
#41332 = PLANE ( 'NONE',  #8874 ) ;
#41333 = CARTESIAN_POINT ( 'NONE',  ( -10.21384395349167562, 3.451719627175087179, 29.49402280011861777 ) ) ;
#41334 = CARTESIAN_POINT ( 'NONE',  ( -29.49875734969026198, -0.3587747205144265483, 2.362022800118626531 ) ) ;
#41335 = CARTESIAN_POINT ( 'NONE',  ( -18.48265707593502327, -12.51853143457666562, -1.500000000000002220 ) ) ;
#41336 = AXIS2_PLACEMENT_3D ( 'NONE', #78360, #56055, #23068 ) ;
#41337 = CARTESIAN_POINT ( 'NONE',  ( -81.62287095715005592, -23.47593901973091235, -1.443836447539004642 ) ) ;
#41338 = CARTESIAN_POINT ( 'NONE',  ( -31.52287095715004739, -23.48783264083373723, -1.443836473376154617 ) ) ;
#41339 = ORIENTED_EDGE ( 'NONE', *, *, #19892, .T. ) ;
#41340 = CARTESIAN_POINT ( 'NONE',  ( -32.62287095715007013, -23.95044443724992078, 10.65354141964649592 ) ) ;
#41341 = CARTESIAN_POINT ( 'NONE',  ( -73.52287095715010423, -24.51283580621364067, 0.6167428607019833642 ) ) ;
#41342 = CARTESIAN_POINT ( 'NONE',  ( 20.84756458399398937, 0.1950554047328266483, -1.500000000000002220 ) ) ;
#41343 = ORIENTED_EDGE ( 'NONE', *, *, #71817, .T. ) ;
#41345 = ORIENTED_EDGE ( 'NONE', *, *, #15433, .F. ) ;
#41344 = CARTESIAN_POINT ( 'NONE',  ( -51.55620429048339304, -24.64898659630528499, 1.056161002820822814 ) ) ;
#41346 = ORIENTED_EDGE ( 'NONE', *, *, #34769, .F. ) ;
#41347 = CARTESIAN_POINT ( 'NONE',  ( -69.79804103094413392, -25.25935328972423832, 7.463048828822199887 ) ) ;
#41348 = CARTESIAN_POINT ( 'NONE',  ( -11.20027426441765961, 17.80179601997297212, -1.500000000000002220 ) ) ;
#41349 = EDGE_LOOP ( 'NONE', ( #62444, #79770, #41114, #82813 ) ) ;
#41350 = FACE_OUTER_BOUND ( 'NONE', #51174, .T. ) ;
#41351 = CARTESIAN_POINT ( 'NONE',  ( 26.73860345374794534, 1.682774720514426114, -7.113848178280766099 ) ) ;
#41352 = CARTESIAN_POINT ( 'NONE',  ( -120.6249267159150378, -24.63419186844610920, 9.035850630976920428 ) ) ;
#41353 = CARTESIAN_POINT ( 'NONE',  ( -86.63220028990764376, -24.15620529776628445, 10.23563542870660292 ) ) ;
#41354 = CARTESIAN_POINT ( 'NONE',  ( -73.52287095715007581, -24.65952944569304606, 1.056160979905697239 ) ) ;
#41355 = CARTESIAN_POINT ( 'NONE',  ( 21.69746526873944958, -0.4026533170205861545, -1.500000000000002220 ) ) ;
#41356 = LINE ( 'NONE', #72310, #90277 ) ;
#41358 = EDGE_LOOP ( 'NONE', ( #99476, #49954, #9362, #33970 ) ) ;
#41357 = CARTESIAN_POINT ( 'NONE',  ( -21.14947813473477822, 6.846651710974520633, 11.49999999999999645 ) ) ;
#41359 = B_SPLINE_CURVE_WITH_KNOTS ( 'NONE', 3,
 ( #21193, #29313, #61286, #21686, #90222, #20696, #75976, #29812 ),
 .UNSPECIFIED., .F., .F.,
 ( 4, 2, 2, 4 ),
 ( 6.384118678617175936E-06, 0.002007151183507260156, 0.003007534715921581642, 0.004007918248335903127 ),
 .UNSPECIFIED. ) ;
#41360 = CARTESIAN_POINT ( 'NONE',  ( -50.82761139903328029, -25.31441737940271253, 5.269904038178990113 ) ) ;
#41361 = CARTESIAN_POINT ( 'NONE',  ( 6.457852148677970305, -6.376774720514415407, 20.09052163342618158 ) ) ;
#41362 = CARTESIAN_POINT ( 'NONE',  ( -54.58953762381672448, -24.64898659630528854, 1.056161002820823258 ) ) ;
#41363 = ORIENTED_EDGE ( 'NONE', *, *, #45875, .T. ) ;
#41364 = B_SPLINE_CURVE_WITH_KNOTS ( 'NONE', 3,
 ( #78257, #9258, #56462, #71676 ),
 .UNSPECIFIED., .F., .F.,
 ( 4, 4 ),
 ( 0.2006432744510161237, 0.2096497057231316852 ),
 .UNSPECIFIED. ) ;
#41366 = EDGE_LOOP ( 'NONE', ( #30732, #78513, #64081, #2534 ) ) ;
#41365 = DIRECTION ( 'NONE',  ( 1.000000000000000000, 0.000000000000000000, 0.000000000000000000 ) ) ;
#41367 = EDGE_CURVE ( 'NONE', #94938, #2928, #74951, .T. ) ;
#41368 = VERTEX_POINT ( 'NONE', #63258 ) ;
#41369 = B_SPLINE_CURVE_WITH_KNOTS ( 'NONE', 3,
 ( #40637, #25902, #16282, #33020 ),
 .UNSPECIFIED., .F., .F.,
 ( 4, 4 ),
 ( 0.9812006513676874153, 0.9902070826398029491 ),
 .UNSPECIFIED. ) ;
#41370 = AXIS2_PLACEMENT_3D ( 'NONE', #16815, #47779, #40160 ) ;
#41371 = CARTESIAN_POINT ( 'NONE',  ( 31.21829842716237735, -4.540774721315884221, 2.131740660352481775 ) ) ;
#41372 = ADVANCED_FACE ( 'NONE', ( #32788 ), #70355, .F. ) ;
#41373 = CARTESIAN_POINT ( 'NONE',  ( -1.972954090310384379, -20.06304030521763337, -1.500000000000002220 ) ) ;
#41374 = CARTESIAN_POINT ( 'NONE',  ( -66.52287095715007581, -24.50321055353804311, 9.387540953477518713 ) ) ;
#41375 = VERTEX_POINT ( 'NONE', #69354 ) ;
#41377 = CARTESIAN_POINT ( 'NONE',  ( -130.5728709571500588, -23.92955623466736270, -0.8917680458859206238 ) ) ;
#41376 =( BOUNDED_SURFACE ( )  B_SPLINE_SURFACE ( 3, 2, ( 
 ( #78190, #7689, #93417 ),
 ( #92915, #93924, #23911 ),
 ( #92419, #22886, #7181 ),
 ( #32030, #78684, #38637 ),
 ( #47770, #84808, #68596 ),
 ( #53875, #61989, #15292 ),
 ( #23391, #86321, #54378 ),
 ( #77683, #85308, #85819 ),
 ( #60990, #16301, #15796 ),
 ( #47265, #8703, #63005 ),
 ( #39639, #24417, #55382 ),
 ( #53380, #84306, #14789 ),
 ( #45757, #76678, #38131 ),
 ( #69086, #49785, #26930 ),
 ( #33539, #17816, #9191 ),
 ( #94935, #1596, #96438 ),
 ( #56899, #87831, #94429 ),
 ( #56398, #17307, #26437 ) ),
 .UNSPECIFIED., .F., .F., .T. ) 
 B_SPLINE_SURFACE_WITH_KNOTS ( ( 4, 2, 2, 2, 2, 2, 2, 2, 4 ),
 ( 3, 3 ),
 ( -3.428680950268159222E-15, 0.002319258964652063781, 0.003478888446979810228, 0.004058703188143683235, 0.004638517929307556242, 0.005798147411635302256, 0.006377962152799175263, 0.006957776893963049138, 0.009277035858618542033 ),
 ( 0.000000000000000000, 1.000000000000000000 ),
 .UNSPECIFIED. ) 
 GEOMETRIC_REPRESENTATION_ITEM ( )  RATIONAL_B_SPLINE_SURFACE ( (
 ( 1.000000000000000000, 0.7071067811865475727, 1.000000000000000000),
 ( 1.000000000000000000, 0.7071067811865475727, 1.000000000000000000),
 ( 1.000000000000000000, 0.7071067811865471286, 1.000000000000000000),
 ( 1.000000000000000000, 0.7071067811865471286, 1.000000000000000000),
 ( 1.000000000000000000, 0.7071067811865473507, 1.000000000000000000),
 ( 1.000000000000000000, 0.7071067811865473507, 1.000000000000000000),
 ( 1.000000000000000000, 0.7071067811865475727, 1.000000000000000000),
 ( 1.000000000000000000, 0.7071067811865475727, 1.000000000000000000),
 ( 1.000000000000000000, 0.7071067811865476838, 1.000000000000000000),
 ( 1.000000000000000000, 0.7071067811865476838, 1.000000000000000000),
 ( 1.000000000000000000, 0.7071067811865473507, 1.000000000000000000),
 ( 1.000000000000000000, 0.7071067811865473507, 1.000000000000000000),
 ( 1.000000000000000000, 0.7071067811865471286, 1.000000000000000000),
 ( 1.000000000000000000, 0.7071067811865471286, 1.000000000000000000),
 ( 1.000000000000000000, 0.7071067811865471286, 1.000000000000000000),
 ( 1.000000000000000000, 0.7071067811865471286, 1.000000000000000000),
 ( 1.000000000000000000, 0.7071067811865475727, 1.000000000000000000),
 ( 1.000000000000000000, 0.7071067811865475727, 1.000000000000000000) ) ) 
 REPRESENTATION_ITEM ( '' )  SURFACE ( )  );
#41378 = CARTESIAN_POINT ( 'NONE',  ( -20.95026660567425481, -7.857139728745305973, -1.500000000000002220 ) ) ;
#41379 = ORIENTED_EDGE ( 'NONE', *, *, #33564, .F. ) ;
#41380 = ORIENTED_EDGE ( 'NONE', *, *, #20535, .F. ) ;
#41381 = CARTESIAN_POINT ( 'NONE',  ( -112.5934603124331517, -23.73791477778912551, 11.05961554403169878 ) ) ;
#41382 = CARTESIAN_POINT ( 'NONE',  ( -44.62287095715004881, -23.47593901973091235, -1.443836447539011525 ) ) ;
#41383 = CARTESIAN_POINT ( 'NONE',  ( -39.82981181716615282, -25.31535245520623079, 4.920765160820281814 ) ) ;
#41384 = DIRECTION ( 'NONE',  ( -0.000000000000000000, -1.000000000000000000, 0.000000000000000000 ) ) ;
#41385 = CARTESIAN_POINT ( 'NONE',  ( -30.59161074801509272, -24.82959736273286566, 8.370978854367633559 ) ) ;
#41386 = CARTESIAN_POINT ( 'NONE',  ( -2.459534284235005863, 19.42625828800391119, -1.500000000000002220 ) ) ;
#41387 = CARTESIAN_POINT ( 'NONE',  ( -20.27875734969026311, -6.376774720514428729, 24.00402280011862288 ) ) ;
#41388 = ORIENTED_EDGE ( 'NONE', *, *, #62216, .T. ) ;
#41389 = CARTESIAN_POINT ( 'NONE',  ( -10.32266838563235467, 18.89866041204108527, 11.49999999999998934 ) ) ;
#41390 = DIRECTION ( 'NONE',  ( 1.250865172912931245E-15, 0.000000000000000000, 1.000000000000000000 ) ) ;
#41391 = CARTESIAN_POINT ( 'NONE',  ( -80.46709582760330193, -25.31572646173322383, 4.967766229843499026 ) ) ;
#41392 = CARTESIAN_POINT ( 'NONE',  ( -53.58953762381671737, -23.47596703998600276, 11.44779298504227505 ) ) ;
#41393 = CARTESIAN_POINT ( 'NONE',  ( -8.499999999999987566, 18.74999999999999645, 0.000000000000000000 ) ) ;
#41395 = VECTOR ( 'NONE', #49190, 1000.000000000000114 ) ;
#41394 = CARTESIAN_POINT ( 'NONE',  ( -13.60431050971674694, 18.46711184989817411, -1.500000000000002220 ) ) ;
#41396 = CC_DESIGN_DATE_AND_TIME_ASSIGNMENT ( #86562, #41910, ( #48909 ) ) ;
#41397 = PERSON_AND_ORGANIZATION ( #70597, #27821 ) ;
#41398 = CARTESIAN_POINT ( 'NONE',  ( -70.52287095715007581, -29.50250786944525672, 11.44777988621623699 ) ) ;
#41399 = DIRECTION ( 'NONE',  ( 0.000000000000000000, -0.9999999999976377785, -2.173523156925979975E-06 ) ) ;
#41400 = CARTESIAN_POINT ( 'NONE',  ( -9.210493908506615313, -17.87979239004878451, 11.49999999999999645 ) ) ;
#41401 = CARTESIAN_POINT ( 'NONE',  ( 32.42932432802503939, -0.3587747205144265483, -0.2107846672978405389 ) ) ;
#41402 = CARTESIAN_POINT ( 'NONE',  ( -32.48906222994808246, -24.35071581493542681, 9.817618358456035921 ) ) ;
#41403 = CARTESIAN_POINT ( 'NONE',  ( -111.6228709571500559, -29.50250243563736774, 8.947779886222136270 ) ) ;
#41404 = DIRECTION ( 'NONE',  ( -1.000000000000000000, 0.000000000000000000, -0.000000000000000000 ) ) ;
#41405 = CARTESIAN_POINT ( 'NONE',  ( -82.52287095715003318, -24.50321055353804311, 9.387540953477522265 ) ) ;
#41406 = CARTESIAN_POINT ( 'NONE',  ( 19.67252036444665109, 2.607452956813616218, 11.49999999999998934 ) ) ;
#41407 = VECTOR ( 'NONE', #14872, 1000.000000000000000 ) ;
#41408 = DIRECTION ( 'NONE',  ( 0.7071067811865476838, 0.000000000000000000, -0.7071067811865474617 ) ) ;
#41409 = CARTESIAN_POINT ( 'NONE',  ( -18.83419513347712737, -5.836681878196540829, -1.500000000000002220 ) ) ;
#41410 = VECTOR ( 'NONE', #11826, 1000.000000000000114 ) ;
#41411 = FACE_OUTER_BOUND ( 'NONE', #66803, .T. ) ;
#41412 = CARTESIAN_POINT ( 'NONE',  ( -101.3738023147422638, -25.26303730729093999, 3.986250639247583827 ) ) ;
#41413 = CALENDAR_DATE ( 2026, 9, 10 ) ;
#41414 = CARTESIAN_POINT ( 'NONE',  ( -57.52287095715004739, -24.33927499327854349, 9.819080762295813614 ) ) ;
#41415 = CARTESIAN_POINT ( 'NONE',  ( -39.42660405732974738, -25.30265167098723822, 5.336464896208934938 ) ) ;
#41416 = CARTESIAN_POINT ( 'NONE',  ( -4.647353109605855792, 20.10343637636090719, 11.49999999999999645 ) ) ;
#41417 = FACE_OUTER_BOUND ( 'NONE', #59574, .T. ) ;
#41418 = CARTESIAN_POINT ( 'NONE',  ( 0.000000000000000000, 5.449678256205721784E-16, -4.450000000000000178 ) ) ;
#41419 = CARTESIAN_POINT ( 'NONE',  ( 16.66146196086182130, -15.28366505690825328, 11.49999999999999645 ) ) ;
#41420 = ORIENTED_EDGE ( 'NONE', *, *, #79148, .F. ) ;
#41421 = CARTESIAN_POINT ( 'NONE',  ( -53.58953762381671737, -24.65952944569304250, 1.056160979905693686 ) ) ;
#41422 = CARTESIAN_POINT ( 'NONE',  ( -51.25929116468429925, -25.28952511681641013, 4.204884817874903646 ) ) ;
#41423 = CARTESIAN_POINT ( 'NONE',  ( -27.68651082257922980, -24.78174777341091328, 2.274903344755643708 ) ) ;
#41424 = EDGE_CURVE ( 'NONE', #60391, #11305, #7443, .T. ) ;
#41425 = LINE ( 'NONE', #97202, #69493 ) ;
#41426 = DIRECTION ( 'NONE',  ( -3.773278334453079030E-23, 0.9999999999976377785, 2.173523156925979128E-06 ) ) ;
#41427 = ORIENTED_EDGE ( 'NONE', *, *, #82307, .T. ) ;
#41428 = CARTESIAN_POINT ( 'NONE',  ( 6.977686149863070675, -22.03694335537135984, 11.49999999999999645 ) ) ;
#41429 = CARTESIAN_POINT ( 'NONE',  ( -21.78311099772515647, -6.823855485095160489, -1.500000000000002220 ) ) ;
#41430 = CARTESIAN_POINT ( 'NONE',  ( -111.3346403563335514, -25.26931265113162794, 4.061649485443762586 ) ) ;
#41431 = CARTESIAN_POINT ( 'NONE',  ( -79.52287095715004739, -23.48783264082476663, -1.443836473390090358 ) ) ;
#41432 = CARTESIAN_POINT ( 'NONE',  ( -63.65418217327448502, -23.48786465467241413, 11.44779295918254824 ) ) ;
#41433 = VECTOR ( 'NONE', #45167, 1000.000000000000114 ) ;
#41434 = EDGE_CURVE ( 'NONE', #30205, #85507, #60279, .T. ) ;
#41435 = CARTESIAN_POINT ( 'NONE',  ( 17.87336509531889561, -13.68139028912531785, 11.49999999999999645 ) ) ;
#41436 = ORIENTED_EDGE ( 'NONE', *, *, #78773, .F. ) ;
#41437 = CARTESIAN_POINT ( 'NONE',  ( -36.62287095715004170, -23.47596703998600276, 11.44779298504227505 ) ) ;
#41438 = CARTESIAN_POINT ( 'NONE',  ( -21.51515180086577317, 4.489188270810763548, 11.49999999999998934 ) ) ;
#41439 = EDGE_CURVE ( 'NONE', #57039, #20017, #16667, .T. ) ;
#41440 = DIRECTION ( 'NONE',  ( -3.773278334453079618E-23, 0.9999999999976377785, 2.173523156925979975E-06 ) ) ;
#41441 = FACE_OUTER_BOUND ( 'NONE', #87014, .T. ) ;
#41442 = CARTESIAN_POINT ( 'NONE',  ( -66.62287095715005592, -29.50247984919015209, -1.443849546365055359 ) ) ;
#41443 = ORIENTED_EDGE ( 'NONE', *, *, #91163, .F. ) ;
#41444 = DIRECTION ( 'NONE',  ( 0.000000000000000000, 0.9999999999976377785, 2.173523156925979128E-06 ) ) ;
#41445 = CARTESIAN_POINT ( 'NONE',  ( -0.4453066574538939171, -6.376774720514410077, 19.14913681718892491 ) ) ;
#41446 = ORIENTED_EDGE ( 'NONE', *, *, #74935, .T. ) ;
#41447 = CARTESIAN_POINT ( 'NONE',  ( -69.52287095715006160, -23.47596703998600631, 11.44779298504228748 ) ) ;
#41448 = CARTESIAN_POINT ( 'NONE',  ( 12.01435098137705637, -16.61664908515649941, -1.500000000000002220 ) ) ;
#41449 = ORIENTED_EDGE ( 'NONE', *, *, #24368, .F. ) ;
#41450 = ORIENTED_EDGE ( 'NONE', *, *, #71491, .T. ) ;
#41451 = VERTEX_POINT ( 'NONE', #78952 ) ;
#41452 = ORIENTED_EDGE ( 'NONE', *, *, #65724, .T. ) ;
#41453 = CARTESIAN_POINT ( 'NONE',  ( -72.22287095715007865, -23.47593901973090169, -1.443836447538997536 ) ) ;
#41454 = CARTESIAN_POINT ( 'NONE',  ( 20.31487730549432413, -11.01532776123576518, 11.49999999999998934 ) ) ;
#41456 = ADVANCED_FACE ( 'NONE', ( #1850 ), #92677, .T. ) ;
#41455 = CARTESIAN_POINT ( 'NONE',  ( -104.6266608578756063, -24.35071581493543746, 9.817618358456019934 ) ) ;
#41457 = CARTESIAN_POINT ( 'NONE',  ( -0.6891947355827284794, 20.32259304938107292, -1.500000000000002220 ) ) ;
#41458 = ORIENTED_EDGE ( 'NONE', *, *, #19191, .T. ) ;
#41459 = DIRECTION ( 'NONE',  ( -0.000000000000000000, 2.173523156925979552E-06, -0.9999999999976378895 ) ) ;
#41460 = DIRECTION ( 'NONE',  ( -3.773278334453079030E-23, 0.9999999999976377785, 2.173523156925979128E-06 ) ) ;
#41461 = CARTESIAN_POINT ( 'NONE',  ( -114.6228709571500559, -29.50248528299804818, 1.056150453629043584 ) ) ;
#41462 = CARTESIAN_POINT ( 'NONE',  ( -70.48847287023792774, -24.92564183028979130, 1.928384488918253536 ) ) ;
#41463 = ORIENTED_EDGE ( 'NONE', *, *, #94500, .T. ) ;
#41464 = LINE ( 'NONE', #10503, #98644 ) ;
#41465 = CARTESIAN_POINT ( 'NONE',  ( -120.6228709571500417, -29.50249982740957577, 7.747779886224967605 ) ) ;
#41466 = VERTEX_POINT ( 'NONE', #63770 ) ;
#41467 = CARTESIAN_POINT ( 'NONE',  ( 4.358738815032396907, -20.29635662749097236, -1.500000000000002220 ) ) ;
#41468 = ORIENTED_EDGE ( 'NONE', *, *, #69180, .F. ) ;
#41470 = ORIENTED_EDGE ( 'NONE', *, *, #93180, .F. ) ;
#41469 = DIRECTION ( 'NONE',  ( 3.773278334444166432E-23, -1.000000000000000000, 0.000000000000000000 ) ) ;
#41471 = AXIS2_PLACEMENT_3D ( 'NONE', #17470, #32189, #15463 ) ;
#41472 = CARTESIAN_POINT ( 'NONE',  ( -82.58953762381672448, -24.64898659630367916, 1.056161002820385830 ) ) ;
#41473 = CARTESIAN_POINT ( 'NONE',  ( -107.6228709571500701, -24.64898659630368272, 1.056161002820831474 ) ) ;
#41474 = ORIENTED_EDGE ( 'NONE', *, *, #73444, .T. ) ;
#41475 = VERTEX_POINT ( 'NONE', #23155 ) ;
#41476 = AXIS2_PLACEMENT_3D ( 'NONE', #29241, #12022, #42991 ) ;
#41477 = DIRECTION ( 'NONE',  ( 0.000000000000000000, 1.000000000000000000, 0.000000000000000000 ) ) ;
#41478 = CARTESIAN_POINT ( 'NONE',  ( -123.5562042904833930, -24.64965694238575011, 8.947790433994185832 ) ) ;
#41479 = AXIS2_PLACEMENT_3D ( 'NONE', #63750, #70336, #24151 ) ;
#41480 = B_SPLINE_CURVE_WITH_KNOTS ( 'NONE', 3,
 ( #18355, #34089, #49322, #29343 ),
 .UNSPECIFIED., .F., .F.,
 ( 4, 4 ),
 ( 0.6092082805810596913, 0.6102090276218251619 ),
 .UNSPECIFIED. ) ;
#41482 = ADVANCED_FACE ( 'NONE', ( #84570 ), #22656, .F. ) ;
#41481 = CARTESIAN_POINT ( 'NONE',  ( -34.52287095715006160, -23.48786465467240347, 11.44779295918255357 ) ) ;
#41484 = ORIENTED_EDGE ( 'NONE', *, *, #56792, .T. ) ;
#41483 = CARTESIAN_POINT ( 'NONE',  ( 4.500060333422437608, -21.59917750860068963, 11.49999999999999645 ) ) ;
#41485 = AXIS2_PLACEMENT_3D ( 'NONE', #97988, #68065, #59450 ) ;
#41486 = CARTESIAN_POINT ( 'NONE',  ( -103.5979499207285954, -23.48783264082477018, -1.443836473390091246 ) ) ;
#41487 = CARTESIAN_POINT ( 'NONE',  ( -20.50338545487000275, 9.463669735852004550, -1.500000000000002220 ) ) ;
#41488 = VECTOR ( 'NONE', #18734, 1000.000000000000000 ) ;
#41490 = ORIENTED_EDGE ( 'NONE', *, *, #93348, .T. ) ;
#41489 = DIRECTION ( 'NONE',  ( -3.773278334453080206E-23, 0.9999999999976377785, 2.173523156925979975E-06 ) ) ;
#41491 = EDGE_LOOP ( 'NONE', ( #34860, #48965, #43493, #71327, #21926, #97487, #30731, #65925 ) ) ;
#41492 = CARTESIAN_POINT ( 'NONE',  ( -59.52287095715004739, -24.66019654487199375, 8.947790411086128159 ) ) ;
#41493 = EDGE_CURVE ( 'NONE', #86903, #25620, #66407, .T. ) ;
#41494 = LINE ( 'NONE', #11532, #84633 ) ;
#41495 = VERTEX_POINT ( 'NONE', #47525 ) ;
#41496 = CARTESIAN_POINT ( 'NONE',  ( -19.86647519178106691, -7.318714840676754818, -1.500000000000002220 ) ) ;
#41497 = DIRECTION ( 'NONE',  ( -3.773278334444166432E-23, 1.000000000000000000, 0.000000000000000000 ) ) ;
#41498 = CARTESIAN_POINT ( 'NONE',  ( -78.94303308397306296, -25.27791628310042427, 5.977536664604797600 ) ) ;
#41499 = CARTESIAN_POINT ( 'NONE',  ( -7.324001883147635894, -6.376774720514413630, 20.17732409774492197 ) ) ;
#41500 = PLANE ( 'NONE',  #38975 ) ;
#41501 = CARTESIAN_POINT ( 'NONE',  ( 1.019757120859956512, 22.21710203930399175, -1.500000000000002220 ) ) ;
#41502 = CARTESIAN_POINT ( 'NONE',  ( -74.62287095715005592, -24.64965695001467694, 8.947790433994184056 ) ) ;
#41503 = VERTEX_POINT ( 'NONE', #78449 ) ;
#41504 = CARTESIAN_POINT ( 'NONE',  ( -5.574014511416001127, -6.376774720514415407, 20.24089781925592391 ) ) ;
#41505 = LINE ( 'NONE', #81061, #78328 ) ;
#41506 = CARTESIAN_POINT ( 'NONE',  ( -14.46832242630667942, -12.86894606327920876, 11.49999999999999645 ) ) ;
#41507 = CARTESIAN_POINT ( 'NONE',  ( 32.06540688909004189, -1.682774720514426114, -12.44045471929205249 ) ) ;
#41508 = DIRECTION ( 'NONE',  ( -1.000000000000000000, 0.000000000000000000, -0.000000000000000000 ) ) ;
#41509 = CARTESIAN_POINT ( 'NONE',  ( -17.65537929698502495, 8.214918384300796461, 11.49999999999998934 ) ) ;
#41510 = CARTESIAN_POINT ( 'NONE',  ( -15.65470850568805083, 14.63654280257262386, 11.49999999999998934 ) ) ;
#41511 = CARTESIAN_POINT ( 'NONE',  ( -56.62287095715009144, -23.94994826722566117, -0.6494450866342736939 ) ) ;
#41512 = CARTESIAN_POINT ( 'NONE',  ( -26.59970390766585169, -24.92774742939907284, 1.981116289752363757 ) ) ;
#41513 = CARTESIAN_POINT ( 'NONE',  ( -32.62287095715004881, -29.50250786944525672, 11.44777988621624409 ) ) ;
#41514 = CARTESIAN_POINT ( 'NONE',  ( -120.6228709571500559, -23.48786465467241769, 11.44779295918253759 ) ) ;
#41515 = B_SPLINE_CURVE_WITH_KNOTS ( 'NONE', 3,
 ( #59596, #83407, #81923, #89538, #89043, #11911, #82906, #90038 ),
 .UNSPECIFIED., .F., .F.,
 ( 4, 2, 2, 4 ),
 ( 6.384118678617664674E-06, 0.002007151183507262758, 0.003007534715921585545, 0.004007918248335907464 ),
 .UNSPECIFIED. ) ;
#41516 = CARTESIAN_POINT ( 'NONE',  ( 0.9741843557120299923, -22.74547949729550922, -1.500000000000002220 ) ) ;
#41517 = B_SPLINE_CURVE_WITH_KNOTS ( 'NONE', 3,
 ( #74417, #96755, #27254, #13003 ),
 .UNSPECIFIED., .F., .F.,
 ( 4, 4 ),
 ( 0.000000000000000000, 0.0001000000000000167422 ),
 .UNSPECIFIED. ) ;
#41518 = EDGE_CURVE ( 'NONE', #39996, #36540, #78409, .T. ) ;
#41519 = DIRECTION ( 'NONE',  ( -1.909006365409802006E-24, 1.000000000000000000, -6.950561949739505919E-24 ) ) ;
#41520 = CARTESIAN_POINT ( 'NONE',  ( -106.5861024369675079, -24.66019654487200441, 8.947790411086108620 ) ) ;
#41521 = CARTESIAN_POINT ( 'NONE',  ( -98.62287095715012697, -24.51283580621365132, 0.6167428607019801445 ) ) ;
#41522 = CARTESIAN_POINT ( 'NONE',  ( 15.94990109002195489, -11.90149544800030590, 11.49999999999999645 ) ) ;
#41523 = CARTESIAN_POINT ( 'NONE',  ( -104.5889287620974244, -24.34968618360934300, 0.1864209137778872205 ) ) ;
#41524 = ADVANCED_FACE ( 'NONE', ( #86075 ), #54637, .F. ) ;
#41525 = CARTESIAN_POINT ( 'NONE',  ( -39.58691133940545370, -24.35071581493543036, 9.817618358456035921 ) ) ;
#41526 = DIRECTION ( 'NONE',  ( 0.000000000000000000, -1.000000000000000000, 0.000000000000000000 ) ) ;
#41527 = ORIENTED_EDGE ( 'NONE', *, *, #82458, .T. ) ;
#41528 = CARTESIAN_POINT ( 'NONE',  ( 29.73860345376319358, 4.772803916115708311, -4.021109907510727943 ) ) ;
#41529 = CARTESIAN_POINT ( 'NONE',  ( -77.52287095715010423, -23.96127896941631974, -0.6493128931038042451 ) ) ;
#41530 = CARTESIAN_POINT ( 'NONE',  ( -10.61912389536305490, -18.88692380039396213, 11.49999999999998934 ) ) ;
#41531 = EDGE_CURVE ( 'NONE', #69943, #30492, #31284, .T. ) ;
#41532 = CARTESIAN_POINT ( 'NONE',  ( -93.62287095715005592, -24.65952944569304606, 1.056160979905701236 ) ) ;
#41533 = CARTESIAN_POINT ( 'NONE',  ( -14.34788840963776124, 13.16932220997287928, -1.500000000000002220 ) ) ;
#41534 = EDGE_CURVE ( 'NONE', #39987, #16850, #33674, .T. ) ;
#41535 = CIRCLE ( 'NONE', #46367, 3.060000000000000053 ) ;
#41536 = DIRECTION ( 'NONE',  ( -0.000000000000000000, 1.000000000000000000, -0.000000000000000000 ) ) ;
#41537 = ORIENTED_EDGE ( 'NONE', *, *, #53877, .T. ) ;
#41538 = DATE_AND_TIME ( #65400, #31217 ) ;
#41539 = ADVANCED_FACE ( 'NONE', ( #16549 ), #8952, .F. ) ;
#41540 = DIRECTION ( 'NONE',  ( -1.000000000000000000, -3.773278334444167608E-23, -8.201307833595939069E-29 ) ) ;
#41541 = CARTESIAN_POINT ( 'NONE',  ( 7.241121213506172438, 19.11196469071355963, 11.49999999999999645 ) ) ;
#41542 = PLANE ( 'NONE',  #40781 ) ;
#41543 = VECTOR ( 'NONE', #32945, 1000.000000000000114 ) ;
#41544 = CARTESIAN_POINT ( 'NONE',  ( 25.05730599792488178, 500000.0000000000582, -18.59674224247031304 ) ) ;
#41545 = ORIENTED_EDGE ( 'NONE', *, *, #71542, .T. ) ;
#41546 = CARTESIAN_POINT ( 'NONE',  ( -62.62287095715004881, -24.65952944569304606, 1.056160979905693909 ) ) ;
#41547 = CARTESIAN_POINT ( 'NONE',  ( 33.54680291763921929, 3.871631182425088191, -11.45966867074879580 ) ) ;
#41548 = CARTESIAN_POINT ( 'NONE',  ( -49.52287095715006160, -23.47596703998600631, 11.44779298504229104 ) ) ;
#41549 = AXIS2_PLACEMENT_3D ( 'NONE', #47192, #2523, #17736 ) ;
#41550 = CARTESIAN_POINT ( 'NONE',  ( 5.271800844963591359, -3.316774720514426456, -28.56638892015329034 ) ) ;
#41551 = AXIS2_PLACEMENT_3D ( 'NONE', #7182, #69087, #100012 ) ;
#41552 = EDGE_CURVE ( 'NONE', #27354, #40387, #31136, .T. ) ;
#41553 = VECTOR ( 'NONE', #10189, 1000.000000000000114 ) ;
#41554 = CARTESIAN_POINT ( 'NONE',  ( -31.79944283184904563, -24.87479601683089570, 8.247789944647550442 ) ) ;
#41555 = VERTEX_POINT ( 'NONE', #48027 ) ;
#41556 = CARTESIAN_POINT ( 'NONE',  ( -66.59259126670630735, -24.15620529776628089, 10.23563542870660470 ) ) ;
#41557 = TOROIDAL_SURFACE ( 'NONE', #59370, 132.8284398600581540, 2.040000000000000036 ) ;
#41558 = B_SPLINE_CURVE_WITH_KNOTS ( 'NONE', 3,
 ( #36854, #83511, #97251, #35852, #44471, #13499, #67818, #91129 ),
 .UNSPECIFIED., .F., .F.,
 ( 4, 2, 2, 4 ),
 ( 0.004987975423754770384, 0.005587860113707344804, 0.005887802458683627678, 0.006187744803659911419 ),
 .UNSPECIFIED. ) ;
#41559 = CARTESIAN_POINT ( 'NONE',  ( -22.04953120734539240, -6.464106996104416858, 11.49999999999999645 ) ) ;
#41560 = CARTESIAN_POINT ( 'NONE',  ( 6.135622925040504327, -21.92205258971886650, -1.500000000000002220 ) ) ;
#41561 = CARTESIAN_POINT ( 'NONE',  ( -110.5481088315369504, -25.00182538069147142, 7.747789668545045139 ) ) ;
#41562 = DIRECTION ( 'NONE',  ( 0.000000000000000000, -1.000000000000000000, 0.000000000000000000 ) ) ;
#41563 = CARTESIAN_POINT ( 'NONE',  ( -90.62479129791826438, -24.92564183028979130, 1.928384488918253536 ) ) ;
#41564 = CARTESIAN_POINT ( 'NONE',  ( 8.160000000000000142, -9.652339641703484574, -1.621096496867199033 ) ) ;
#41565 = CARTESIAN_POINT ( 'NONE',  ( -44.52287095715004739, -23.48783264082477018, -1.443836473390094577 ) ) ;
#41566 = CARTESIAN_POINT ( 'NONE',  ( -20.57654891367511851, 7.437132321665034240, 11.49999999999998934 ) ) ;
#41567 = EDGE_CURVE ( 'NONE', #99058, #62319, #56648, .T. ) ;
#41568 = CARTESIAN_POINT ( 'NONE',  ( -70.62287095715005592, -24.99132157543083821, 2.256160258750667502 ) ) ;
#41569 = EDGE_CURVE ( 'NONE', #14228, #89486, #9952, .T. ) ;
#41570 = CARTESIAN_POINT ( 'NONE',  ( -26.17111397533802730, -24.91964606936674187, 3.942482870127836048 ) ) ;
#41571 = CARTESIAN_POINT ( 'NONE',  ( 1.999999999999998224, 2.265596578422603396E-15, -18.50000000000000000 ) ) ;
#41572 = CARTESIAN_POINT ( 'NONE',  ( -98.99594346619821295, -25.25460612665171212, 5.589964028470313373 ) ) ;
#41573 = ORIENTED_EDGE ( 'NONE', *, *, #9694, .F. ) ;
#41574 = CARTESIAN_POINT ( 'NONE',  ( -1.067026067711715154, -20.38227831319515460, 11.49999999999998934 ) ) ;
#41575 = VERTEX_POINT ( 'NONE', #79460 ) ;
#41576 = ORIENTED_EDGE ( 'NONE', *, *, #24445, .T. ) ;
#41577 = CARTESIAN_POINT ( 'NONE',  ( 22.09143763772896918, 6.410036269187016522, 11.49999999999998934 ) ) ;
#41579 = EDGE_CURVE ( 'NONE', #40572, #25637, #64777, .T. ) ;
#41578 = CARTESIAN_POINT ( 'NONE',  ( -78.62287095715005592, -24.64898659630367916, 1.056161002820826145 ) ) ;
#41580 = ORIENTED_EDGE ( 'NONE', *, *, #71459, .F. ) ;
#41581 = VECTOR ( 'NONE', #58310, 1000.000000000000114 ) ;
#41582 = FACE_OUTER_BOUND ( 'NONE', #251, .T. ) ;
#41583 = CARTESIAN_POINT ( 'NONE',  ( 0.000000000000000000, -1.473225279485573802, 0.000000000000000000 ) ) ;
#41584 = EDGE_CURVE ( 'NONE', #32620, #35375, #7076, .T. ) ;
#41585 = EDGE_CURVE ( 'NONE', #93008, #28007, #8630, .T. ) ;
#41586 = LINE ( 'NONE', #55812, #99737 ) ;
#41587 = CARTESIAN_POINT ( 'NONE',  ( -119.4728709572981842, -25.30561158020721635, 5.197944563078277014 ) ) ;
#41589 = VERTEX_POINT ( 'NONE', #57646 ) ;
#41588 = CARTESIAN_POINT ( 'NONE',  ( -6.079122355442096115, 20.50309271558274915, 11.49999999999999645 ) ) ;
#41590 = ORIENTED_EDGE ( 'NONE', *, *, #76504, .T. ) ;
#41591 = CARTESIAN_POINT ( 'NONE',  ( -9.187330254778467875, -20.22999604658808082, 11.49999999999998934 ) ) ;
#41592 = CARTESIAN_POINT ( 'NONE',  ( -19.50335911044312098, -6.847048061534898977, 11.49999999999998934 ) ) ;
#41593 = VERTEX_POINT ( 'NONE', #18561 ) ;
#41594 = CARTESIAN_POINT ( 'NONE',  ( -5.877732331298974877, -6.376774720514411854, 19.69174559449349005 ) ) ;
#41595 = DIRECTION ( 'NONE',  ( 0.000000000000000000, 0.9999999999976377785, 2.173523156925979975E-06 ) ) ;
#41596 = ORIENTED_EDGE ( 'NONE', *, *, #83211, .F. ) ;
#41597 = B_SPLINE_CURVE_WITH_KNOTS ( 'NONE', 3,
 ( #70343, #86062, #47512, #69338 ),
 .UNSPECIFIED., .F., .F.,
 ( 4, 4 ),
 ( 0.000000000000000000, 0.0001000000000000167422 ),
 .UNSPECIFIED. ) ;
#41598 = CARTESIAN_POINT ( 'NONE',  ( -80.62287095715005592, -23.47593901973091235, -1.443836447539004642 ) ) ;
#41599 = EDGE_LOOP ( 'NONE', ( #75128, #19609, #33952, #84472 ) ) ;
#41600 = CARTESIAN_POINT ( 'NONE',  ( 7.805843057017202824, -3.316774720514425567, -27.15467198446602026 ) ) ;
#41601 =( NAMED_UNIT ( * ) SI_UNIT ( $, .STERADIAN. ) SOLID_ANGLE_UNIT ( ) );
#41602 = CARTESIAN_POINT ( 'NONE',  ( -14.93763623016880082, -14.57113377498261997, -1.500000000000002220 ) ) ;
#41603 = CARTESIAN_POINT ( 'NONE',  ( 8.256513476402210117, 20.27555108428041208, 11.49999999999999645 ) ) ;
#41604 = B_SPLINE_CURVE_WITH_KNOTS ( 'NONE', 3,
 ( #27907, #58863, #5564, #75562 ),
 .UNSPECIFIED., .F., .F.,
 ( 4, 4 ),
 ( 0.000000000000000000, 9.999999999998897304E-05 ),
 .UNSPECIFIED. ) ;
#41605 = CARTESIAN_POINT ( 'NONE',  ( -26.38306202989770455, -24.77993590978327276, 6.654069811898469133 ) ) ;
#41606 = CARTESIAN_POINT ( 'NONE',  ( 15.27779656932134067, -3.574456261761478792, -27.18758201676848785 ) ) ;
#41607 = CARTESIAN_POINT ( 'NONE',  ( 22.48569338394020534, -0.9006126209707296937, -1.500000000000002220 ) ) ;
#41608 = VECTOR ( 'NONE', #23282, 1000.000000000000000 ) ;
#41609 = CARTESIAN_POINT ( 'NONE',  ( -18.74228827200876779, -9.293929619069025705, -1.500000000000002220 ) ) ;
#41610 = CARTESIAN_POINT ( 'NONE',  ( -38.48527873623334017, -24.51314013834316086, 0.6176544820404135105 ) ) ;
#41611 = DIRECTION ( 'NONE',  ( -3.773278334453079618E-23, 0.9999999999976377785, 2.173523156925978705E-06 ) ) ;
#41612 = CARTESIAN_POINT ( 'NONE',  ( 2.750000000000001332, 27.59999999999999432, 2.100000000000000089 ) ) ;
#41613 = EDGE_LOOP ( 'NONE', ( #29040, #87876, #72671, #98519 ) ) ;
#41614 = ORIENTED_EDGE ( 'NONE', *, *, #98841, .F. ) ;
#41615 = ORIENTED_EDGE ( 'NONE', *, *, #50918, .F. ) ;
#41616 = FACE_OUTER_BOUND ( 'NONE', #78386, .T. ) ;
#41617 = EDGE_LOOP ( 'NONE', ( #25421, #47113, #39129, #13383 ) ) ;
#41618 = VECTOR ( 'NONE', #76702, 1000.000000000000000 ) ;
#41619 = CARTESIAN_POINT ( 'NONE',  ( 5.397486108853063236, 20.74927772461418485, -1.500000000000002220 ) ) ;
#41620 = VERTEX_POINT ( 'NONE', #49032 ) ;
#41621 = CARTESIAN_POINT ( 'NONE',  ( 0.2196812790064107401, -6.376774720514408301, 19.42522865122897002 ) ) ;
#41622 = AXIS2_PLACEMENT_3D ( 'NONE', #44834, #14858, #60567 ) ;
#41623 = CARTESIAN_POINT ( 'NONE',  ( 11.82777538550527119, 17.46297031709455183, -1.500000000000002220 ) ) ;
#41624 = CARTESIAN_POINT ( 'NONE',  ( -30.53645441241393499, -24.83558246553552706, 8.370654131274084975 ) ) ;
#41625 = DIRECTION ( 'NONE',  ( 0.000000000000000000, -0.9999999999976377785, -2.173523156925979975E-06 ) ) ;
#41626 = DIRECTION ( 'NONE',  ( 0.000000000000000000, 0.000000000000000000, -1.000000000000000000 ) ) ;
#41627 = VECTOR ( 'NONE', #57224, 1000.000000000000000 ) ;
#41628 = CARTESIAN_POINT ( 'NONE',  ( -101.5506399398690007, -24.34968618360934300, 0.1864209137778871928 ) ) ;
#41629 = CARTESIAN_POINT ( 'NONE',  ( -109.8280019483771497, -25.31620647586430906, 5.181285762822000152 ) ) ;
#41630 = CARTESIAN_POINT ( 'NONE',  ( 4.500060333422437608, -21.59917750860068963, -1.500000000000002220 ) ) ;
#41631 = ORIENTED_EDGE ( 'NONE', *, *, #100039, .F. ) ;
#41632 = CARTESIAN_POINT ( 'NONE',  ( -116.5939885159102261, -23.48783264082478439, -1.443836473390061936 ) ) ;
#41633 = CARTESIAN_POINT ( 'NONE',  ( -65.05438548721848235, -6.475225279485573360, 0.7300228001186309656 ) ) ;
#41634 = CARTESIAN_POINT ( 'NONE',  ( -41.47025245262053517, -25.27955988164092105, 5.160615522818375212 ) ) ;
#41635 = VECTOR ( 'NONE', #5464, 1000.000000000000000 ) ;
#41636 = CARTESIAN_POINT ( 'NONE',  ( -62.51545974119872540, -23.73791477778911840, 11.05961554403171121 ) ) ;
#41637 = CARTESIAN_POINT ( 'NONE',  ( -53.62287095715005592, -29.50250786944525672, 11.44777988621624054 ) ) ;
#41638 = DIRECTION ( 'NONE',  ( -0.000000000000000000, 1.000000000000000000, -0.000000000000000000 ) ) ;
#41639 = CARTESIAN_POINT ( 'NONE',  ( -13.37813101364405100, 16.61575060780308277, 11.49999999999998934 ) ) ;
#41640 = CARTESIAN_POINT ( 'NONE',  ( -29.52287095715006160, -29.50247984919040434, -1.443849432928222987 ) ) ;
#41641 = CARTESIAN_POINT ( 'NONE',  ( -117.5228709571500332, -24.66019654487200441, 8.947790411086108620 ) ) ;
#41642 = CARTESIAN_POINT ( 'NONE',  ( 7.160000000000000142, -6.754662360505033547, 7.925641719537454222 ) ) ;
#41643 = DIRECTION ( 'NONE',  ( 0.000000000000000000, 0.7071067811865437980, 0.7071067811865513475 ) ) ;
#41644 = CARTESIAN_POINT ( 'NONE',  ( -16.68516988606489448, 15.22057433622007316, -1.500000000000002220 ) ) ;
#41645 = EDGE_CURVE ( 'NONE', #58910, #99120, #65150, .T. ) ;
#41646 = CARTESIAN_POINT ( 'NONE',  ( -83.62287095715007013, -24.66019654487199730, 8.947790411086126383 ) ) ;
#41647 = ORIENTED_EDGE ( 'NONE', *, *, #56999, .F. ) ;
#41648 = CARTESIAN_POINT ( 'NONE',  ( -35.62287095715005592, -23.48786465467240347, 11.44779295918255180 ) ) ;
#41649 = CARTESIAN_POINT ( 'NONE',  ( -122.6228709571500843, -23.94994826722515668, -0.6494450866351679785 ) ) ;
#41650 = CARTESIAN_POINT ( 'NONE',  ( -19.67082186522023690, -1.387426831159568108, 11.49999999999999645 ) ) ;
#41651 = DIRECTION ( 'NONE',  ( -3.773278334444167608E-23, 1.000000000000000000, 0.000000000000000000 ) ) ;
#41652 = CARTESIAN_POINT ( 'NONE',  ( -73.52287095715007581, -24.64965694238407323, 8.947790433994200043 ) ) ;
#41653 = EDGE_LOOP ( 'NONE', ( #94382, #2793, #34164, #77605 ) ) ;
#41654 = LINE ( 'NONE', #50261, #44187 ) ;
#41655 = DIRECTION ( 'NONE',  ( 0.000000000000000000, 0.000000000000000000, 1.000000000000000000 ) ) ;
#41657 = ADVANCED_FACE ( 'NONE', ( #41411 ), #34863, .T. ) ;
#41656 = CARTESIAN_POINT ( 'NONE',  ( -124.5909694504235148, -23.73791477778912551, 11.05961554403169878 ) ) ;
#41658 = AXIS2_PLACEMENT_3D ( 'NONE', #27006, #11773, #3185 ) ;
#41659 = ADVANCED_FACE ( 'NONE', ( #58145 ), #94684, .F. ) ;
#41660 = CARTESIAN_POINT ( 'NONE',  ( -91.22287095715003602, -23.47593901973090169, -1.443836447538996870 ) ) ;
#41661 = PLANE ( 'NONE',  #78735 ) ;
#41662 = ADVANCED_FACE ( 'NONE', ( #57152 ), #7885, .T. ) ;
#41663 = FACE_OUTER_BOUND ( 'NONE', #16348, .T. ) ;
#41664 = DIRECTION ( 'NONE',  ( 0.000000000000000000, 0.9999999999976377785, 2.173523156925979128E-06 ) ) ;
#41665 = CARTESIAN_POINT ( 'NONE',  ( 13.37688099249405127, 14.58279310912311111, 11.49999999999998934 ) ) ;
#41666 = B_SPLINE_CURVE_WITH_KNOTS ( 'NONE', 3,
 ( #56355, #33001, #60596, #83906 ),
 .UNSPECIFIED., .F., .F.,
 ( 4, 4 ),
 ( 1.387778780781445521E-17, 9.999999999997510880E-05 ),
 .UNSPECIFIED. ) ;
#41667 = ORIENTED_EDGE ( 'NONE', *, *, #57122, .T. ) ;
#41668 = ADVANCED_FACE ( 'NONE', ( #28677 ), #74351, .F. ) ;
#41669 = AXIS2_PLACEMENT_3D ( 'NONE', #79291, #25515, #16898 ) ;
#41670 = CARTESIAN_POINT ( 'NONE',  ( -0.5548696950099620828, -20.20177982057877841, 11.49999999999999645 ) ) ;
#41671 = CARTESIAN_POINT ( 'NONE',  ( 6.199338013146583393, -5.876774720514415407, 20.11757922567734980 ) ) ;
#41672 = ORIENTED_EDGE ( 'NONE', *, *, #61611, .F. ) ;
#41673 = CARTESIAN_POINT ( 'NONE',  ( -65.58953762381672448, -23.47596703998600276, 11.44779298504227505 ) ) ;
#41674 = CARTESIAN_POINT ( 'NONE',  ( 0.1645010273463760886, -0.3687607960183646449, -1.417169167140628350 ) ) ;
#41675 = CARTESIAN_POINT ( 'NONE',  ( -59.58953762381672448, -23.48786465467241058, 11.44779295918254824 ) ) ;
#41676 = CARTESIAN_POINT ( 'NONE',  ( -31.58953762381671382, -23.48786465467240347, 11.44779295918255180 ) ) ;
#41677 = CARTESIAN_POINT ( 'NONE',  ( -39.62287095715004881, -23.48783264082477373, -1.443836473390072594 ) ) ;
#41678 = CARTESIAN_POINT ( 'NONE',  ( -81.62287095715005592, -24.65952944569304606, 1.056160979905699460 ) ) ;
#41679 = CARTESIAN_POINT ( 'NONE',  ( 18.22975119132022215, -8.346483668847822557, -1.500000000000002220 ) ) ;
#41680 = EDGE_CURVE ( 'NONE', #86931, #3899, #21541, .T. ) ;
#41681 = PLANE ( 'NONE',  #35389 ) ;
#41682 = ORIENTED_EDGE ( 'NONE', *, *, #1818, .T. ) ;
#41683 = VECTOR ( 'NONE', #45151, 1000.000000000000000 ) ;
#41684 = EDGE_CURVE ( 'NONE', #81663, #50305, #67252, .T. ) ;
#41685 = CARTESIAN_POINT ( 'NONE',  ( -0.02075734969026423599, 5.965225279485572685, -0.08597719988137648983 ) ) ;
#41686 = CARTESIAN_POINT ( 'NONE',  ( -35.58103620899936459, -24.73486907724918282, 1.287355809206967461 ) ) ;
#41687 = CARTESIAN_POINT ( 'NONE',  ( -79.34687923781920915, -25.26778825442007559, 5.960409282772108241 ) ) ;
#41688 = PLANE ( 'NONE',  #85331 ) ;
#41689 = CARTESIAN_POINT ( 'NONE',  ( -101.0647859952741783, -25.13441618929300603, 2.968838638867928648 ) ) ;
#41690 = ADVANCED_FACE ( 'NONE', ( #60641 ), #13438, .F. ) ;
#41691 = VECTOR ( 'NONE', #50173, 1000.000000000000000 ) ;
#41692 = LINE ( 'NONE', #10728, #5736 ) ;
#41693 = CARTESIAN_POINT ( 'NONE',  ( -99.90680059161346094, -25.20650842489795807, 6.812665538484692362 ) ) ;
#41694 = ORIENTED_EDGE ( 'NONE', *, *, #52755, .T. ) ;
#41695 = AXIS2_PLACEMENT_3D ( 'NONE', #8660, #30986, #91882 ) ;
#41696 = CARTESIAN_POINT ( 'NONE',  ( -13.46841296510753061, 15.22696965993213070, -1.500000000000002220 ) ) ;
#41697 = VERTEX_POINT ( 'NONE', #43417 ) ;
#41698 = ADVANCED_FACE ( 'NONE', ( #99169 ), #84836, .T. ) ;
#41699 = CARTESIAN_POINT ( 'NONE',  ( 31.61404304915243202, 4.508643932895013862, 26.44173824648443727 ) ) ;
#41700 = CARTESIAN_POINT ( 'NONE',  ( -127.5564499832624108, -23.48786465467242124, 11.44779295918253226 ) ) ;
#41701 = ORIENTED_EDGE ( 'NONE', *, *, #17964, .T. ) ;
#41702 = CARTESIAN_POINT ( 'NONE',  ( -105.6228709571500559, -24.63287334234180292, 0.9662140553045504010 ) ) ;
#41703 = EDGE_CURVE ( 'NONE', #14845, #42618, #53024, .T. ) ;
#41704 = CARTESIAN_POINT ( 'NONE',  ( -49.74873825466967503, -25.26264143758006142, 6.941713674697326475 ) ) ;
#41705 = CARTESIAN_POINT ( 'NONE',  ( -19.69812919673063689, -0.3587747205143964613, -22.00173861453436430 ) ) ;
#41706 = CARTESIAN_POINT ( 'NONE',  ( -9.521469661382619520, 18.92286876745961166, 11.49999999999999645 ) ) ;
#41707 = CARTESIAN_POINT ( 'NONE',  ( -14.81638660137672225, 16.44347145309322045, 11.49999999999998934 ) ) ;
#41708 = EDGE_CURVE ( 'NONE', #30045, #43147, #83448, .T. ) ;
#41709 = CARTESIAN_POINT ( 'NONE',  ( -1.637206367458305500, 20.51943892441452633, 11.49999999999998934 ) ) ;
#41710 = B_SPLINE_CURVE_WITH_KNOTS ( 'NONE', 3,
 ( #94864, #1021, #94364, #64455 ),
 .UNSPECIFIED., .F., .F.,
 ( 4, 4 ),
 ( 0.000000000000000000, 9.999999999997510880E-05 ),
 .UNSPECIFIED. ) ;
#41711 = ORIENTED_EDGE ( 'NONE', *, *, #79429, .F. ) ;
#41712 = CARTESIAN_POINT ( 'NONE',  ( -113.5895376238167245, -23.47596703998600631, 11.44779298504227683 ) ) ;
#41713 = ORIENTED_EDGE ( 'NONE', *, *, #43593, .T. ) ;
#41714 = CARTESIAN_POINT ( 'NONE',  ( 7.166666666666668739, -6.376774720514414518, 20.78665865384614975 ) ) ;
#41715 = DIRECTION ( 'NONE',  ( 0.000000000000000000, -2.173523156925979552E-06, 0.9999999999976378895 ) ) ;
#41716 = ORIENTED_EDGE ( 'NONE', *, *, #47680, .T. ) ;
#41717 = ORIENTED_EDGE ( 'NONE', *, *, #75667, .F. ) ;
#41718 = ORIENTED_EDGE ( 'NONE', *, *, #43698, .T. ) ;
#41719 = CARTESIAN_POINT ( 'NONE',  ( -116.6228709571500275, -23.47596703998600631, 11.44779298504227860 ) ) ;
#41720 = CARTESIAN_POINT ( 'NONE',  ( 6.727829057902616761, -6.376774720514417183, 20.13865202822440281 ) ) ;
#41721 = CARTESIAN_POINT ( 'NONE',  ( 6.329711958793041049, -5.876774720514411854, 19.73172534246499765 ) ) ;
#41722 = CARTESIAN_POINT ( 'NONE',  ( -20.55201672899488585, 2.666056886502145673, -1.500000000000002220 ) ) ;
#41723 = CARTESIAN_POINT ( 'NONE',  ( -20.56447267657262401, 6.860157381912782348, 11.49999999999999645 ) ) ;
#41724 = ORIENTED_EDGE ( 'NONE', *, *, #2877, .F. ) ;
#41725 = CARTESIAN_POINT ( 'NONE',  ( -94.52287095715006160, -23.48786465467242479, 11.44779295918254292 ) ) ;
#41726 = AXIS2_PLACEMENT_3D ( 'NONE', #88409, #34626, #57475 ) ;
#41727 = LINE ( 'NONE', #20349, #40016 ) ;
#41728 = CARTESIAN_POINT ( 'NONE',  ( 10.13505985054399083, -19.98934331558005439, 11.49999999999998934 ) ) ;
#41729 = CARTESIAN_POINT ( 'NONE',  ( -110.9909297185884327, -25.14264188228929697, 6.986250900936915365 ) ) ;
#41730 = FACE_OUTER_BOUND ( 'NONE', #40808, .T. ) ;
#41731 = VERTEX_POINT ( 'NONE', #55519 ) ;
#41732 = CARTESIAN_POINT ( 'NONE',  ( 9.071512145086501278, -0.9000000000000000222, -3.687490859131162591 ) ) ;
#41733 = DIRECTION ( 'NONE',  ( 0.000000000000000000, -2.173523156925979552E-06, 0.9999999999976378895 ) ) ;
#41734 = B_SPLINE_SURFACE_WITH_KNOTS ( 'NONE', 3, 1, ( 
 ( #71268, #79867 ),
 ( #87488, #47933 ),
 ( #48437, #25078 ),
 ( #32695, #17978 ),
 ( #63166, #10360 ),
 ( #85479, #46930 ),
 ( #70265, #749 ),
 ( #31702, #40317 ),
 ( #9356, #62668 ),
 ( #63677, #24079 ),
 ( #55048, #70767 ),
 ( #47432, #8861 ),
 ( #1263, #94597 ),
 ( #67165, #88494 ),
 ( #50934, #81872 ),
 ( #20457, #97591 ),
 ( #51430, #58546 ),
 ( #97098, #65679 ),
 ( #4752, #66680 ) ),
 .UNSPECIFIED., .F., .F., .F.,
 ( 4, 1, 1, 1, 1, 1, 1, 1, 1, 1, 1, 1, 1, 1, 1, 1, 4 ),
 ( 2, 2 ),
 ( 0.000000000000000000, 0.05090243768365541877, 0.1010340427826159765, 0.1510838170086600818, 0.2030619875551388231, 0.2562484343627552397, 0.3108467145046008295, 0.3687690999693260530, 0.4300150403860056869, 0.4925196472738457842, 0.5560487215256794125, 0.6219956829149523303, 0.6901923690829533387, 0.7613848549885010586, 0.8363562199507234007, 0.9154870053271095820, 1.000000000000000000 ),
 ( 0.000000000000000000, 1.000000000000000000 ),
 .UNSPECIFIED. ) ;
#41735 = ORIENTED_EDGE ( 'NONE', *, *, #47982, .T. ) ;
#41736 = VERTEX_POINT ( 'NONE', #77817 ) ;
#41737 = CARTESIAN_POINT ( 'NONE',  ( -46.59348642383254457, -24.15620529776627379, 10.23563542870660825 ) ) ;
#41738 = ORIENTED_EDGE ( 'NONE', *, *, #30938, .F. ) ;
#41739 = DIRECTION ( 'NONE',  ( 0.000000000000000000, 0.9999999999976377785, 2.173523156925978705E-06 ) ) ;
#41740 = CARTESIAN_POINT ( 'NONE',  ( -4.916304867406160461, -20.68799595667769964, -1.500000000000002220 ) ) ;
#41741 = ORIENTED_EDGE ( 'NONE', *, *, #73062, .F. ) ;
#41742 = CARTESIAN_POINT ( 'NONE',  ( 22.81105451610979173, 8.475225279485572472, -19.61691820600746539 ) ) ;
#41743 = PRODUCT_DEFINITION_SHAPE ( 'NONE', 'NONE',  #69913 ) ;
#41744 = CARTESIAN_POINT ( 'NONE',  ( -19.11951126197014261, -10.51958540666066533, -1.500000000000002220 ) ) ;
#41745 = DIRECTION ( 'NONE',  ( 0.000000000000000000, 2.173523156925980399E-06, -0.9999999999976378895 ) ) ;
#41746 = CARTESIAN_POINT ( 'NONE',  ( -71.52287095715007581, -23.47596703998600631, 11.44779298504228748 ) ) ;
#41747 = CARTESIAN_POINT ( 'NONE',  ( -85.62287095715004170, -29.50248789122583659, 2.256150453626215580 ) ) ;
#41748 = CARTESIAN_POINT ( 'NONE',  ( -9.708950231915746798, -19.59419465507263070, -1.500000000000002220 ) ) ;
#41749 = CARTESIAN_POINT ( 'NONE',  ( 6.697025426467099862, -6.376774720514424288, 21.43052570396496037 ) ) ;
#41750 = VERTEX_POINT ( 'NONE', #55016 ) ;
#41751 = CARTESIAN_POINT ( 'NONE',  ( 29.58031977903354459, -3.717801497966991775, 29.19834312781581076 ) ) ;
#41752 = CARTESIAN_POINT ( 'NONE',  ( -85.50394113191364909, -24.52399227489127043, 9.353111116836526406 ) ) ;
#41753 = VECTOR ( 'NONE', #57616, 1000.000000000000114 ) ;
#41754 = ORIENTED_EDGE ( 'NONE', *, *, #28523, .F. ) ;
#41755 = LINE ( 'NONE', #26007, #82104 ) ;
#41756 = VERTEX_POINT ( 'NONE', #7318 ) ;
#41757 = CARTESIAN_POINT ( 'NONE',  ( -88.62287095715004170, -29.50247984919015209, -1.443849546365051806 ) ) ;
#41758 = CARTESIAN_POINT ( 'NONE',  ( -7.641025641025638748, -6.376774720514427841, 21.75000000000001066 ) ) ;
#41759 = CARTESIAN_POINT ( 'NONE',  ( 3.248270302591931724, 20.98854991013365279, 11.49999999999998934 ) ) ;
#41760 = DIRECTION ( 'NONE',  ( 0.000000000000000000, 0.000000000000000000, -1.000000000000000000 ) ) ;
#41761 = CARTESIAN_POINT ( 'NONE',  ( -130.5728709571501440, -23.87624887660337691, 11.01174216661999772 ) ) ;
#41762 = LINE ( 'NONE', #55479, #61604 ) ;
#41763 = CIRCLE ( 'NONE', #98435, 1.700000000000008615 ) ;
#41764 = CARTESIAN_POINT ( 'NONE',  ( -68.54924039429016602, -24.15543982623907127, -0.2315651400026649820 ) ) ;
#41765 = CARTESIAN_POINT ( 'NONE',  ( -12.45040968399260883, -14.89389333286084671, -1.500000000000002220 ) ) ;
#41766 = CARTESIAN_POINT ( 'NONE',  ( -45.58529216989418131, -24.63355581998384736, 0.9682620441944017609 ) ) ;
#41767 = ORIENTED_EDGE ( 'NONE', *, *, #31789, .F. ) ;
#41768 = EDGE_CURVE ( 'NONE', #81441, #18133, #83263, .T. ) ;
#41769 = CARTESIAN_POINT ( 'NONE',  ( -0.9579564967699066846, 19.55851204243107233, 11.49999999999999645 ) ) ;
#41770 = CARTESIAN_POINT ( 'NONE',  ( -5.000686017310577824, -5.876774720514410077, 19.46274624311237034 ) ) ;
#41771 = VECTOR ( 'NONE', #10796, 1000.000000000000000 ) ;
#41772 = EDGE_CURVE ( 'NONE', #24307, #96497, #16938, .T. ) ;
#41773 = PLANE ( 'NONE',  #90151 ) ;
#41774 = VERTEX_POINT ( 'NONE', #24044 ) ;
#41775 = ADVANCED_FACE ( 'NONE', ( #85444, #15931 ), #46897, .F. ) ;
#41776 = CARTESIAN_POINT ( 'NONE',  ( -97.62287095715005592, -23.47593901973091235, -1.443836447539001089 ) ) ;
#41777 = DIRECTION ( 'NONE',  ( 0.000000000000000000, 0.9999999999976377785, 2.173523156925979975E-06 ) ) ;
#41778 = EDGE_CURVE ( 'NONE', #19254, #98127, #30163, .T. ) ;
#41779 = PLANE ( 'NONE',  #19615 ) ;
#41780 = CARTESIAN_POINT ( 'NONE',  ( 13.31108137134011393, -2.682774720514426559, -27.16778744938429924 ) ) ;
#41781 = CARTESIAN_POINT ( 'NONE',  ( 13.13437215454093199, 14.66711140016434278, 11.49999999999998934 ) ) ;
#41782 = ORIENTED_EDGE ( 'NONE', *, *, #93875, .F. ) ;
#41783 = CARTESIAN_POINT ( 'NONE',  ( -41.32836283488544638, -5.152774720514427642, 39.26872235229541985 ) ) ;
#41784 = CARTESIAN_POINT ( 'NONE',  ( -8.701767255460435280, 21.38705905713849020, -1.500000000000002220 ) ) ;
#41785 = B_SPLINE_CURVE_WITH_KNOTS ( 'NONE', 3,
 ( #58127, #72346, #89064, #57132 ),
 .UNSPECIFIED., .F., .F.,
 ( 4, 4 ),
 ( 8.673617379884035472E-19, 0.0002632372126714214219 ),
 .UNSPECIFIED. ) ;
#41787 = ADVANCED_FACE ( 'NONE', ( #31660 ), #72510, .T. ) ;
#41786 = PERSON_AND_ORGANIZATION ( #70597, #27821 ) ;
#41788 = ORIENTED_EDGE ( 'NONE', *, *, #98152, .T. ) ;
#41789 = CARTESIAN_POINT ( 'NONE',  ( 3.128267882468583228, -6.376774720514424288, 21.08409277973916218 ) ) ;
#41790 = LINE ( 'NONE', #64135, #73364 ) ;
#41791 = CARTESIAN_POINT ( 'NONE',  ( -92.62287095715008434, -23.96127896941632685, -0.6493128931037810414 ) ) ;
#41792 = CARTESIAN_POINT ( 'NONE',  ( -97.50897550903059141, -24.51419770103157703, 9.386484678747176957 ) ) ;
#41793 = CARTESIAN_POINT ( 'NONE',  ( -20.27875734969026311, 7.743225279485574042, 21.75402280011862644 ) ) ;
#41794 = DIRECTION ( 'NONE',  ( -1.000000000000000000, 0.000000000000000000, 0.000000000000000000 ) ) ;
#41795 = CARTESIAN_POINT ( 'NONE',  ( 32.25183987940364005, 6.376774720514426953, 2.026414261721653176 ) ) ;
#41796 = CARTESIAN_POINT ( 'NONE',  ( 19.92730240972663935, 0.8534881809820089593, 11.49999999999998934 ) ) ;
#41797 = CARTESIAN_POINT ( 'NONE',  ( -75.53786448191598879, -24.83644354573578994, 8.397322867130100121 ) ) ;
#41798 = CARTESIAN_POINT ( 'NONE',  ( 19.88832268942539017, -0.5522253751840191516, -1.500000000000002220 ) ) ;
#41799 = VERTEX_POINT ( 'NONE', #49915 ) ;
#41800 = AXIS2_PLACEMENT_3D ( 'NONE', #14639, #9032, #39983 ) ;
#41801 = CARTESIAN_POINT ( 'NONE',  ( -122.5228709571500758, -24.50321055353805733, 9.387540953477520489 ) ) ;
#41802 = CARTESIAN_POINT ( 'NONE',  ( -125.5228709571500616, -24.99132157543084531, 2.256160258750667502 ) ) ;
#41803 = DIRECTION ( 'NONE',  ( -0.2488812114211667037, -0.000000000000000000, -0.9685340172660599212 ) ) ;
#41804 = CARTESIAN_POINT ( 'NONE',  ( -80.53777078880429485, -24.92592662359561118, 8.075495903017996469 ) ) ;
#41805 = CARTESIAN_POINT ( 'NONE',  ( -4.307737697753418082, 20.33289072680551968, 11.49999999999999645 ) ) ;
#41806 = CARTESIAN_POINT ( 'NONE',  ( -38.52287095715006870, -23.47593901973090169, -1.443836447538997092 ) ) ;
#41807 = CARTESIAN_POINT ( 'NONE',  ( -50.45700478961177993, -25.18512690614146265, 3.295337589435844539 ) ) ;
#41808 = CARTESIAN_POINT ( 'NONE',  ( -2.521034868938843765, 22.70145277337256218, 11.49999999999999645 ) ) ;
#41809 = ORIENTED_EDGE ( 'NONE', *, *, #88179, .T. ) ;
#41810 = B_SPLINE_SURFACE_WITH_KNOTS ( 'NONE', 3, 3, ( 
 ( #31478, #16254, #1032, #15750 ),
 ( #15247, #29, #16745, #47212 ),
 ( #78630, #40603, #32481, #63454 ),
 ( #40096, #94375, #71050, #39591 ),
 ( #55835, #86763, #70543, #46203 ),
 ( #17251, #53828, #48218, #31981 ),
 ( #62949, #39085, #47717, #32990 ) ),
 .UNSPECIFIED., .F., .F., .F.,
 ( 4, 3, 4 ),
 ( 4, 4 ),
 ( 0.7945040050992238090, 0.8970133687736495665, 0.9995227324480753239 ),
 ( 0.1195243700447448237, 0.1205922749804624466 ),
 .UNSPECIFIED. ) ;
#41811 = DIRECTION ( 'NONE',  ( 0.000000000000000000, 0.9999999999976377785, 2.173523156925979128E-06 ) ) ;
#41812 = CARTESIAN_POINT ( 'NONE',  ( 16.00000000000000000, 0.000000000000000000, 0.000000000000000000 ) ) ;
#41813 = ORIENTED_EDGE ( 'NONE', *, *, #51980, .F. ) ;
#41814 = CARTESIAN_POINT ( 'NONE',  ( -14.69473627950705108, 13.90061564059656440, 11.49999999999998934 ) ) ;
#41815 = CYLINDRICAL_SURFACE ( 'NONE', #14427, 3.349999999999998757 ) ;
#41816 = CARTESIAN_POINT ( 'NONE',  ( -4.929522925832178437, -5.965225279485572685, -28.63504101147568903 ) ) ;
#41817 = AXIS2_PLACEMENT_3D ( 'NONE', #59128, #44398, #89070 ) ;
#41818 = DIRECTION ( 'NONE',  ( -1.000000000000000000, -0.000000000000000000, -0.000000000000000000 ) ) ;
#41820 = VERTEX_POINT ( 'NONE', #1725 ) ;
#41819 = EDGE_CURVE ( 'NONE', #98879, #55323, #87962, .T. ) ;
#41821 = CARTESIAN_POINT ( 'NONE',  ( -78.94507867893470632, -25.28412234718345530, 5.882162795622602580 ) ) ;
#41822 = CARTESIAN_POINT ( 'NONE',  ( -51.29687923781917647, -25.27420715122566364, 3.993462153431225570 ) ) ;
#41823 = CARTESIAN_POINT ( 'NONE',  ( -19.32702923155483177, -5.217993511516596961, -1.500000000000002220 ) ) ;
#41824 = CARTESIAN_POINT ( 'NONE',  ( 9.933205088616889000, -18.45388779576350302, 11.49999999999999645 ) ) ;
#41825 = PLANE ( 'NONE',  #30795 ) ;
#41826 = DIRECTION ( 'NONE',  ( 0.000000000000000000, 0.000000000000000000, 1.000000000000000000 ) ) ;
#41827 = CARTESIAN_POINT ( 'NONE',  ( 16.78392297789021015, 14.29496084597832883, -1.500000000000002220 ) ) ;
#41828 = EDGE_CURVE ( 'NONE', #68707, #19712, #3243, .T. ) ;
#41829 = VECTOR ( 'NONE', #30084, 1000.000000000000114 ) ;
#41830 = CARTESIAN_POINT ( 'NONE',  ( -39.65036112522632550, -25.31589258738599568, 4.754946542694897360 ) ) ;
#41831 = ORIENTED_EDGE ( 'NONE', *, *, #23311, .T. ) ;
#41832 = DIRECTION ( 'NONE',  ( 0.000000000000000000, -0.9999999999976377785, -2.173523156925979975E-06 ) ) ;
#41833 = DIRECTION ( 'NONE',  ( 3.773278334444166432E-23, -1.000000000000000000, 0.000000000000000000 ) ) ;
#41834 = CARTESIAN_POINT ( 'NONE',  ( 17.91726403014145319, -0.5000000000000000000, -1.691563534834430227 ) ) ;
#41835 = ORIENTED_EDGE ( 'NONE', *, *, #8867, .F. ) ;
#41836 = CARTESIAN_POINT ( 'NONE',  ( -51.62287095715005592, -29.50250243563736774, 8.947779886222146928 ) ) ;
#41837 = VERTEX_POINT ( 'NONE', #34676 ) ;
#41838 = VECTOR ( 'NONE', #82824, 1000.000000000000000 ) ;
#41839 = VERTEX_POINT ( 'NONE', #2234 ) ;
#41840 = CARTESIAN_POINT ( 'NONE',  ( 13.55016566187448923, 5.965225279485570908, -28.22449608469281657 ) ) ;
#41841 = CARTESIAN_POINT ( 'NONE',  ( -100.8972602205940063, -25.27404646237970454, 2.905315430698961698 ) ) ;
#41842 = PLANE ( 'NONE',  #35796 ) ;
#41843 = CARTESIAN_POINT ( 'NONE',  ( -14.05295919346176170, -14.94737400546395456, -1.500000000000002220 ) ) ;
#41844 = ORIENTED_EDGE ( 'NONE', *, *, #48010, .T. ) ;
#41845 = DIRECTION ( 'NONE',  ( -0.000000000000000000, 0.000000000000000000, 1.000000000000000000 ) ) ;
#41846 = CARTESIAN_POINT ( 'NONE',  ( 6.509931258083027750, -5.876774720514417183, 20.09204137875607188 ) ) ;
#41847 = CARTESIAN_POINT ( 'NONE',  ( -96.52287095715001897, -24.66019654487199730, 8.947790411086115725 ) ) ;
#41848 = CARTESIAN_POINT ( 'NONE',  ( -21.40455707349245529, -6.346402434563959361, 11.49999999999998934 ) ) ;
#41849 = B_SPLINE_CURVE_WITH_KNOTS ( 'NONE', 3,
 ( #78500, #86627, #62817, #25223 ),
 .UNSPECIFIED., .F., .F.,
 ( 4, 4 ),
 ( 0.3207290247458886023, 0.3297354560180041361 ),
 .UNSPECIFIED. ) ;
#41850 = CARTESIAN_POINT ( 'NONE',  ( -0.05083659990941528928, -22.39188026470795378, 1.363349870542274189 ) ) ;
#41851 = CARTESIAN_POINT ( 'NONE',  ( -122.5228709571500616, -23.47596703998600631, 11.44779298504227860 ) ) ;
#41852 = ORIENTED_EDGE ( 'NONE', *, *, #79295, .T. ) ;
#41853 = CARTESIAN_POINT ( 'NONE',  ( -101.6228709571500559, -24.65952944569304606, 1.056160979905702790 ) ) ;
#41854 = FACE_OUTER_BOUND ( 'NONE', #36564, .T. ) ;
#41855 = VECTOR ( 'NONE', #63126, 1000.000000000000000 ) ;
#41856 = CARTESIAN_POINT ( 'NONE',  ( -17.86878485216894319, -10.78119150571587781, 11.49999999999998934 ) ) ;
#41857 = ORIENTED_EDGE ( 'NONE', *, *, #90530, .F. ) ;
#41859 = EDGE_LOOP ( 'NONE', ( #91262, #48916, #18245, #98413 ) ) ;
#41858 = PLANE ( 'NONE',  #91134 ) ;
#41860 = ORIENTED_EDGE ( 'NONE', *, *, #22270, .F. ) ;
#41861 = DIRECTION ( 'NONE',  ( 0.000000000000000000, 1.000000000000000000, 0.000000000000000000 ) ) ;
#41862 = CARTESIAN_POINT ( 'NONE',  ( 20.56459456670464547, 4.482388377596099538, -1.500000000000002220 ) ) ;
#41863 = VERTEX_POINT ( 'NONE', #56021 ) ;
#41864 = CARTESIAN_POINT ( 'NONE',  ( -95.62287095715005592, -23.47593901973091235, -1.443836447539001089 ) ) ;
#41865 = DIRECTION ( 'NONE',  ( -3.773278334453079618E-23, 0.9999999999976377785, 2.173523156925979975E-06 ) ) ;
#41866 = CARTESIAN_POINT ( 'NONE',  ( -120.6258260306066745, -24.40133493613049964, 9.663955038902800609 ) ) ;
#41867 = CARTESIAN_POINT ( 'NONE',  ( -101.4365978186105366, -25.03152376165066073, 7.227289064697279386 ) ) ;
#41868 = CARTESIAN_POINT ( 'NONE',  ( -129.6228709571500417, -24.64965695001463430, 8.947790411086117501 ) ) ;
#41869 = CARTESIAN_POINT ( 'NONE',  ( -20.76051858633888259, -6.224802954461835292, -1.500000000000002220 ) ) ;
#41870 = CARTESIAN_POINT ( 'NONE',  ( -79.99654428403167117, -25.05785469192115045, 7.493821146766848074 ) ) ;
#41872 = ORIENTED_EDGE ( 'NONE', *, *, #13322, .T. ) ;
#41871 = CARTESIAN_POINT ( 'NONE',  ( -15.91109736606077441, 15.52988587838853540, 11.49999999999999645 ) ) ;
#41873 = CARTESIAN_POINT ( 'NONE',  ( -51.19842764437002813, -25.31441786624639079, 5.493892295348231869 ) ) ;
#41874 = CARTESIAN_POINT ( 'NONE',  ( -100.6814946224345846, -25.30267106336103922, 4.736250553104468963 ) ) ;
#41875 = CARTESIAN_POINT ( 'NONE',  ( 13.91401389203221406, 6.376774720514426953, 158.0376437107427137 ) ) ;
#41876 = ORIENTED_EDGE ( 'NONE', *, *, #39827, .F. ) ;
#41878 = EDGE_LOOP ( 'NONE', ( #43427, #8815, #60054, #81011 ) ) ;
#41877 = CARTESIAN_POINT ( 'NONE',  ( -76.62287095715007013, -23.72747288104442021, -1.053458166803662444 ) ) ;
#41879 = B_SPLINE_CURVE_WITH_KNOTS ( 'NONE', 3,
 ( #35966, #76510, #37963, #7015 ),
 .UNSPECIFIED., .F., .F.,
 ( 4, 4 ),
 ( 0.000000000000000000, 0.0002633127703855885223 ),
 .UNSPECIFIED. ) ;
#41880 = ORIENTED_EDGE ( 'NONE', *, *, #27573, .T. ) ;
#41881 = DIRECTION ( 'NONE',  ( 0.000000000000000000, 0.000000000000000000, 1.000000000000000000 ) ) ;
#41882 = B_SPLINE_CURVE_WITH_KNOTS ( 'NONE', 3,
 ( #47687, #45305, #29561, #83850, #76226, #24336 ),
 .UNSPECIFIED., .F., .F.,
 ( 4, 2, 4 ),
 ( 0.000000000000000000, 0.001380764517853247733, 0.002761529035706495466 ),
 .UNSPECIFIED. ) ;
#41883 = CARTESIAN_POINT ( 'NONE',  ( -107.5228709571501327, -23.96127896942120827, -0.6493128930941749477 ) ) ;
#41884 = CARTESIAN_POINT ( 'NONE',  ( -51.52287095715006870, -23.47596703998600631, 11.44779298504229104 ) ) ;
#41885 = ORIENTED_EDGE ( 'NONE', *, *, #96389, .F. ) ;
#41886 = EDGE_CURVE ( 'NONE', #10916, #95349, #30055, .T. ) ;
#41887 = CARTESIAN_POINT ( 'NONE',  ( -130.5728709571500588, -24.85767102478814650, 1.377180730259818908 ) ) ;
#41888 = CARTESIAN_POINT ( 'NONE',  ( -13.02831144489870319, 18.26546089674541307, -1.500000000000002220 ) ) ;
#41889 = B_SPLINE_CURVE_WITH_KNOTS ( 'NONE', 3,
 ( #79450, #73353, #49525, #94675, #11941, #9942, #57142 ),
 .UNSPECIFIED., .F., .F.,
 ( 4, 3, 4 ),
 ( 0.000000000000000000, 1.195459452644217715E-05, 2.107775188753445374E-05 ),
 .UNSPECIFIED. ) ;
#41890 = ORIENTED_EDGE ( 'NONE', *, *, #50843, .F. ) ;
#41891 = CARTESIAN_POINT ( 'NONE',  ( -89.40841769935769889, -25.23397913219577049, 6.409327625469732226 ) ) ;
#41892 = CARTESIAN_POINT ( 'NONE',  ( -101.6251895264811225, -24.51419770103158413, 9.386484678747175181 ) ) ;
#41893 = ADVANCED_FACE ( 'NONE', ( #71238 ), #72240, .F. ) ;
#41894 = CARTESIAN_POINT ( 'NONE',  ( -98.62287095715005592, -29.50250786944525672, 11.44777988621623166 ) ) ;
#41895 = LINE ( 'NONE', #72840, #70839 ) ;
#41896 = AXIS2_PLACEMENT_3D ( 'NONE', #7447, #48030, #85075 ) ;
#41897 = ADVANCED_FACE ( 'NONE', ( #18936 ), #17946, .F. ) ;
#41898 = CARTESIAN_POINT ( 'NONE',  ( -30.57310282152668890, -25.30559561715417516, 6.147794833475641596 ) ) ;
#41899 = CARTESIAN_POINT ( 'NONE',  ( 17.47348308817029405, 8.859467055162037141, -1.500000000000002220 ) ) ;
#41900 = EDGE_CURVE ( 'NONE', #33323, #95752, #86952, .T. ) ;
#41901 = DIRECTION ( 'NONE',  ( -0.000000000000000000, 1.000000000000000000, -0.000000000000000000 ) ) ;
#41902 = ORIENTED_EDGE ( 'NONE', *, *, #85531, .F. ) ;
#41903 = CARTESIAN_POINT ( 'NONE',  ( -19.98823316618875268, 7.996883007359760320, 11.49999999999998934 ) ) ;
#41904 = DIRECTION ( 'NONE',  ( -0.000000000000000000, -0.000000000000000000, 1.000000000000000000 ) ) ;
#41905 = EDGE_CURVE ( 'NONE', #14276, #35568, #71239, .T. ) ;
#41906 = LINE ( 'NONE', #72347, #31891 ) ;
#41907 = PLANE ( 'NONE',  #84679 ) ;
#41908 = CARTESIAN_POINT ( 'NONE',  ( -128.6228709571500417, -23.48786465467242479, 11.44779295918253403 ) ) ;
#41909 = CARTESIAN_POINT ( 'NONE',  ( -5.713817535623205046, 22.21719745612757535, -1.500000000000002220 ) ) ;
#41910 = DATE_TIME_ROLE ( 'classification_date' ) ;
#41911 = DIRECTION ( 'NONE',  ( -3.773278334453079618E-23, 0.9999999999976377785, 2.173523156925979975E-06 ) ) ;
#41912 = CARTESIAN_POINT ( 'NONE',  ( -49.50711149851015591, -23.96119346886879953, -0.6495511937832113558 ) ) ;
#41913 = CARTESIAN_POINT ( 'NONE',  ( 10.01938154005162218, -17.43019892170380913, 11.49999999999999645 ) ) ;
#41914 = CARTESIAN_POINT ( 'NONE',  ( -109.8914236385200525, -25.10927407888622653, 2.885852620966828042 ) ) ;
#41915 = CARTESIAN_POINT ( 'NONE',  ( 13.57581083383197296, -5.876774720514426953, 19.78786796564403616 ) ) ;
#41916 = VECTOR ( 'NONE', #2878, 1000.000000000000000 ) ;
#41917 = CARTESIAN_POINT ( 'NONE',  ( 2.100208336950355914, 1.530808498934186394E-16, -1.249999999999996003 ) ) ;
#41918 = CARTESIAN_POINT ( 'NONE',  ( -65.62287095715008434, -24.14321612903114556, -0.2833117244521677347 ) ) ;
#41919 = EDGE_CURVE ( 'NONE', #62726, #92355, #61534, .T. ) ;
#41920 = FACE_OUTER_BOUND ( 'NONE', #96262, .T. ) ;
#41921 = CARTESIAN_POINT ( 'NONE',  ( -19.81728208556213389, 0.3677575464312098363, 11.49999999999998934 ) ) ;
#41922 = PLANE ( 'NONE',  #22089 ) ;
#41923 = CARTESIAN_POINT ( 'NONE',  ( -19.65353550717971487, 1.628721094194526486, -1.500000000000002220 ) ) ;
#41924 = CARTESIAN_POINT ( 'NONE',  ( -60.58953762381671737, -23.48783264082478439, -1.443836473390068820 ) ) ;
#41925 = AXIS2_PLACEMENT_3D ( 'NONE', #1233, #31164, #86956 ) ;
#41926 = PERSON_AND_ORGANIZATION ( #98436, #68376 ) ;
#41927 = DIRECTION ( 'NONE',  ( -1.000000000000000000, -3.773278334444166432E-23, -8.201307841325785021E-29 ) ) ;
#41928 = CARTESIAN_POINT ( 'NONE',  ( 3.450324536843889067, -6.376774720514404748, 18.60429515659643229 ) ) ;
#41929 = CARTESIAN_POINT ( 'NONE',  ( 20.22723401096548201, -3.897675682603606084, 11.49999999999999645 ) ) ;
#41931 = B_SPLINE_CURVE_WITH_KNOTS ( 'NONE', 3,
 ( #34603, #49841, #94487, #65574 ),
 .UNSPECIFIED., .F., .F.,
 ( 4, 4 ),
 ( 0.000000000000000000, 9.999999999998897304E-05 ),
 .UNSPECIFIED. ) ;
#41930 = CARTESIAN_POINT ( 'NONE',  ( -24.90875734969025501, 5.965225279485572685, 30.51402280011862089 ) ) ;
#41932 = CARTESIAN_POINT ( 'NONE',  ( 10.43192878459595185, 20.09917060401269850, 11.49999999999999645 ) ) ;
#41933 = ORIENTED_EDGE ( 'NONE', *, *, #28038, .F. ) ;
#41934 = CARTESIAN_POINT ( 'NONE',  ( -69.34542366606198982, -25.25639427084792032, 6.299234904174134897 ) ) ;
#41935 = CARTESIAN_POINT ( 'NONE',  ( -109.6228709571501128, -24.33927499327855415, 9.819080762295815390 ) ) ;
#41936 = EDGE_CURVE ( 'NONE', #90373, #59480, #95567, .T. ) ;
#41937 = DIRECTION ( 'NONE',  ( 0.000000000000000000, 0.000000000000000000, -1.000000000000000000 ) ) ;
#41938 = CARTESIAN_POINT ( 'NONE',  ( -36.58953762381672448, -23.48783264082477729, -1.443836473390072372 ) ) ;
#41939 = B_SPLINE_CURVE_WITH_KNOTS ( 'NONE', 3,
 ( #93276, #70458, #93783, #9549, #8048, #71967 ),
 .UNSPECIFIED., .F., .F.,
 ( 4, 2, 4 ),
 ( 0.000000000000000000, 0.5000000000000000000, 1.000000000000000000 ),
 .UNSPECIFIED. ) ;
#41940 = ADVANCED_FACE ( 'NONE', ( #50402 ), #26052, .T. ) ;
#41941 = ORIENTED_EDGE ( 'NONE', *, *, #90910, .F. ) ;
#41942 = CARTESIAN_POINT ( 'NONE',  ( -79.89247415061277025, -25.26749899421020373, 5.073623479721068641 ) ) ;
#41943 = CARTESIAN_POINT ( 'NONE',  ( -7.631545101075025705, 21.52643039700453897, -1.500000000000002220 ) ) ;
#41944 = CARTESIAN_POINT ( 'NONE',  ( 32.66876533700882845, -5.965225279485572685, -12.58926540598385557 ) ) ;
#41945 = FACE_OUTER_BOUND ( 'NONE', #80293, .T. ) ;
#41946 = CARTESIAN_POINT ( 'NONE',  ( -82.51327497436713543, -23.96169478059713143, 10.65365249895718414 ) ) ;
#41947 = CARTESIAN_POINT ( 'NONE',  ( -12.88509029660790617, -18.40938060607246740, 11.49999999999999645 ) ) ;
#41948 = EDGE_LOOP ( 'NONE', ( #90777, #25978, #71770, #68194 ) ) ;
#41949 = CARTESIAN_POINT ( 'NONE',  ( -36.58953762381671737, -23.47596703998600276, 11.44779298504227505 ) ) ;
#41950 = CARTESIAN_POINT ( 'NONE',  ( -18.27885182143903720, 12.20952002138517045, -1.500000000000002220 ) ) ;
#41951 = FACE_OUTER_BOUND ( 'NONE', #99815, .T. ) ;
#41952 = CARTESIAN_POINT ( 'NONE',  ( -0.02075734969026423599, 5.866774720514426278, -0.08597719988137648983 ) ) ;
#41953 = CARTESIAN_POINT ( 'NONE',  ( -69.62287095715005592, -29.50250786944525672, 11.44777988621623699 ) ) ;
#41954 = VERTEX_POINT ( 'NONE', #80340 ) ;
#41955 = CARTESIAN_POINT ( 'NONE',  ( -71.52287095715010423, -23.48783264082477018, -1.443836473390091246 ) ) ;
#41956 = EDGE_CURVE ( 'NONE', #3335, #12512, #74813, .T. ) ;
#41957 = CARTESIAN_POINT ( 'NONE',  ( 22.81105451610979173, -1.682774720514426114, -18.46691820600746681 ) ) ;
#41958 = ORIENTED_EDGE ( 'NONE', *, *, #63883, .T. ) ;
#41959 = CARTESIAN_POINT ( 'NONE',  ( -103.5228709571501042, -23.48783264082477018, -1.443836473390087916 ) ) ;
#41960 = VECTOR ( 'NONE', #70505, 1000.000000000000000 ) ;
#41961 = CARTESIAN_POINT ( 'NONE',  ( -11.60840874443078263, -16.91462557209307960, 11.49999999999998934 ) ) ;
#41962 = ORIENTED_EDGE ( 'NONE', *, *, #82237, .T. ) ;
#41963 = VECTOR ( 'NONE', #27277, 1000.000000000000000 ) ;
#41964 = VERTEX_POINT ( 'NONE', #65647 ) ;
#41965 = EDGE_LOOP ( 'NONE', ( #56109, #98367, #37382 ) ) ;
#41966 = DIRECTION ( 'NONE',  ( -3.773278334453079030E-23, 0.9999999999976377785, 2.173523156925979128E-06 ) ) ;
#41967 = CARTESIAN_POINT ( 'NONE',  ( 6.977686149863070675, -22.03694335537135984, 11.49999999999998934 ) ) ;
#41968 = CARTESIAN_POINT ( 'NONE',  ( -104.5117914961601713, -24.51419770103158768, 9.386484678747166299 ) ) ;
#41969 = CARTESIAN_POINT ( 'NONE',  ( -18.82316870354832616, 7.800066519331792847, -1.500000000000002220 ) ) ;
#41970 = ADVANCED_FACE ( 'NONE', ( #25046 ), #79335, .T. ) ;
#41971 = ORIENTED_EDGE ( 'NONE', *, *, #41314, .F. ) ;
#41972 = LINE ( 'NONE', #28223, #33139 ) ;
#41973 = VECTOR ( 'NONE', #73038, 1000.000000000000114 ) ;
#41974 = DIRECTION ( 'NONE',  ( 0.000000000000000000, -0.000000000000000000, -1.000000000000000000 ) ) ;
#41975 = DIRECTION ( 'NONE',  ( 0.000000000000000000, 0.000000000000000000, 1.000000000000000000 ) ) ;
#41976 = CARTESIAN_POINT ( 'NONE',  ( -71.66734858977571321, -25.25855161950308769, 6.551008370017044058 ) ) ;
#41977 = ORIENTED_EDGE ( 'NONE', *, *, #30514, .F. ) ;
#41978 = CARTESIAN_POINT ( 'NONE',  ( -29.17364183714287762, -25.21531997571052486, 3.835940394522498575 ) ) ;
#41979 = CARTESIAN_POINT ( 'NONE',  ( -93.52287095715007581, -24.50321055353807154, 9.387540953477520489 ) ) ;
#41980 = VERTEX_POINT ( 'NONE', #79833 ) ;
#41981 = AXIS2_PLACEMENT_3D ( 'NONE', #10343, #73251, #55533 ) ;
#41982 = CARTESIAN_POINT ( 'NONE',  ( -4.307737697753418082, 20.33289072680551968, -1.500000000000002220 ) ) ;
#41983 = ORIENTED_EDGE ( 'NONE', *, *, #33299, .F. ) ;
#41984 = CC_DESIGN_PERSON_AND_ORGANIZATION_ASSIGNMENT ( #37770, #78314, ( #21418 ) ) ;
#41986 = VERTEX_POINT ( 'NONE', #96072 ) ;
#41985 = CARTESIAN_POINT ( 'NONE',  ( -125.5888994550898303, -24.92564183028979485, 1.928384488918254425 ) ) ;
#41987 = B_SPLINE_CURVE_WITH_KNOTS ( 'NONE', 3,
 ( #24508, #55478, #86414, #71702 ),
 .UNSPECIFIED., .F., .F.,
 ( 4, 4 ),
 ( 0.000000000000000000, 9.999999999998897304E-05 ),
 .UNSPECIFIED. ) ;
#41988 = CARTESIAN_POINT ( 'NONE',  ( -41.66427398439827812, -23.48786465467240347, 11.44779295918255180 ) ) ;
#41989 = CARTESIAN_POINT ( 'NONE',  ( -102.6228709571500701, -24.50216790748099172, 0.6166512839513705879 ) ) ;
#41990 = ORIENTED_EDGE ( 'NONE', *, *, #73705, .F. ) ;
#41991 = ORIENTED_EDGE ( 'NONE', *, *, #43217, .F. ) ;
#41992 = DIRECTION ( 'NONE',  ( 0.000000000000000000, 0.9999999999976377785, 2.173523156925979128E-06 ) ) ;
#41993 = B_SPLINE_CURVE_WITH_KNOTS ( 'NONE', 3,
 ( #49253, #34512, #80180, #65484, #26892, #72084 ),
 .UNSPECIFIED., .F., .F.,
 ( 4, 2, 4 ),
 ( 1.570887131794638196E-05, 0.001396322306279761073, 0.002776935741241575838 ),
 .UNSPECIFIED. ) ;
#41994 = AXIS2_PLACEMENT_3D ( 'NONE', #46063, #83601, #100307 ) ;
#41995 = CARTESIAN_POINT ( 'NONE',  ( 6.881670032588234953, 3.316774720514422903, -27.26384557944684062 ) ) ;
#41996 = B_SPLINE_CURVE_WITH_KNOTS ( 'NONE', 3,
 ( #10605, #55299, #33947, #26334, #3505, #10105, #64926, #71016, #25328, #1507, #9103, #88239, #41063, #34449 ),
 .UNSPECIFIED., .F., .F.,
 ( 4, 2, 2, 2, 2, 2, 4 ),
 ( 0.000000000000000000, 0.0001952411637358899145, 0.0003904823274717798289, 0.0007809646549435615009, 0.001171446982415343119, 0.001366688146151234145, 0.001561929309887125170 ),
 .UNSPECIFIED. ) ;
#41997 = CARTESIAN_POINT ( 'NONE',  ( -71.10442080388585850, -25.31201661486003474, 5.639839434645662841 ) ) ;
#41999 = ORIENTED_EDGE ( 'NONE', *, *, #16602, .F. ) ;
#41998 = CARTESIAN_POINT ( 'NONE',  ( 22.02032638543937182, 1.892999326154024553, 11.49999999999999645 ) ) ;
#42000 = LINE ( 'NONE', #64852, #98163 ) ;
#42001 = CARTESIAN_POINT ( 'NONE',  ( -19.18631400275845422, -11.98935526391121087, -1.500000000000002220 ) ) ;
#42003 = ORIENTED_EDGE ( 'NONE', *, *, #13390, .T. ) ;
#42002 = FACE_OUTER_BOUND ( 'NONE', #82808, .T. ) ;
#42004 = ORIENTED_EDGE ( 'NONE', *, *, #34078, .F. ) ;
#42005 = DIRECTION ( 'NONE',  ( -3.773278334444166432E-23, 1.000000000000000000, 0.000000000000000000 ) ) ;
#42006 = CARTESIAN_POINT ( 'NONE',  ( -0.3059464777392852941, -8.530684776139525027, -9.000000000000000000 ) ) ;
#42007 = EDGE_LOOP ( 'NONE', ( #24128, #18265, #79084, #15231 ) ) ;
#42008 = CARTESIAN_POINT ( 'NONE',  ( -9.521469661382619520, 18.92286876745961166, 11.49999999999998934 ) ) ;
#42009 = CARTESIAN_POINT ( 'NONE',  ( -78.95422500253870624, -25.03138002232442005, 6.195241297245855705 ) ) ;
#42010 = CARTESIAN_POINT ( 'NONE',  ( -7.064692883725313344, -5.876774720514411854, 19.55266968305501862 ) ) ;
#42011 = FACE_OUTER_BOUND ( 'NONE', #24986, .T. ) ;
#42012 = CARTESIAN_POINT ( 'NONE',  ( 0.7529269182969693386, -22.20201975079678647, -1.500000000000002220 ) ) ;
#42013 = CARTESIAN_POINT ( 'NONE',  ( -49.25033725972690490, -25.03220807947403515, 7.108518685806449966 ) ) ;
#42014 = EDGE_CURVE ( 'NONE', #47218, #27337, #967, .T. ) ;
#42015 = EDGE_LOOP ( 'NONE', ( #43565, #32173, #12916, #11215 ) ) ;
#42016 = CARTESIAN_POINT ( 'NONE',  ( -79.62287095715004170, -23.47596703998600631, 11.44779298504227860 ) ) ;
#42017 = CARTESIAN_POINT ( 'NONE',  ( -104.5228709571500758, -23.47593901973090524, -1.443836447538996204 ) ) ;
#42018 = CARTESIAN_POINT ( 'NONE',  ( -36.54573691098784849, -24.15620529776627379, 10.23563542870660825 ) ) ;
#42019 = DIRECTION ( 'NONE',  ( -0.000000000000000000, -0.000000000000000000, -1.000000000000000000 ) ) ;
#42020 = CARTESIAN_POINT ( 'NONE',  ( -14.34788840963776124, 13.16932220997287928, -1.500000000000002220 ) ) ;
#42021 = ADVANCED_FACE ( 'NONE', ( #90944 ), #4223, .T. ) ;
#42022 = CARTESIAN_POINT ( 'NONE',  ( 9.988417798295188277, 18.97302403871600518, 11.49999999999998934 ) ) ;
#42023 = CARTESIAN_POINT ( 'NONE',  ( -27.26447433122779884, -24.92774676623168162, 1.676004566348860525 ) ) ;
#42024 = B_SPLINE_CURVE_WITH_KNOTS ( 'NONE', 3,
 ( #80962, #73357, #41918, #95687, #26172, #27180, #81470, #65762 ),
 .UNSPECIFIED., .F., .F.,
 ( 4, 2, 2, 4 ),
 ( 0.000000000000000000, 0.002001098010032689289, 0.003001647015049033716, 0.004002196020065378577 ),
 .UNSPECIFIED. ) ;
#42025 = EDGE_CURVE ( 'NONE', #72159, #16956, #36170, .T. ) ;
#42026 = DIRECTION ( 'NONE',  ( -3.773278334453079618E-23, 0.9999999999976377785, 2.173523156925979975E-06 ) ) ;
#42027 = CARTESIAN_POINT ( 'NONE',  ( -77.63398884115866849, -24.15543982623907482, -0.2315651400026658147 ) ) ;
#42028 = CARTESIAN_POINT ( 'NONE',  ( -20.46125754976198508, 9.905080999540670561, -1.500000000000002220 ) ) ;
#42029 = CARTESIAN_POINT ( 'NONE',  ( 147.5443831022365373, -6.474179415928273507, 23.70558727230208618 ) ) ;
#42030 = CARTESIAN_POINT ( 'NONE',  ( -98.55250747182638804, -24.15543982623907482, -0.2315651400026625395 ) ) ;
#42031 = CARTESIAN_POINT ( 'NONE',  ( -119.5228709571500758, -29.50250786944525672, 11.44777988621622811 ) ) ;
#42032 = CARTESIAN_POINT ( 'NONE',  ( 3.219775368129482285, -19.64489633315863770, 11.49999999999999645 ) ) ;
#42033 = PLANE ( 'NONE',  #21156 ) ;
#42034 = CIRCLE ( 'NONE', #38740, 3.979149600822063704 ) ;
#42035 = CARTESIAN_POINT ( 'NONE',  ( -39.54606421208372069, -24.15620529776627734, 10.23563542870661180 ) ) ;
#42036 = CARTESIAN_POINT ( 'NONE',  ( -128.5562042904833788, -24.66019654487199730, 8.947790411086119278 ) ) ;
#42037 = ORIENTED_EDGE ( 'NONE', *, *, #32238, .F. ) ;
#42038 = EDGE_CURVE ( 'NONE', #27723, #53455, #20419, .T. ) ;
#42039 = PLANE ( 'NONE',  #62374 ) ;
#42040 = DIRECTION ( 'NONE',  ( -3.773278334453079030E-23, 0.9999999999976377785, 2.173523156925979128E-06 ) ) ;
#42041 = CARTESIAN_POINT ( 'NONE',  ( 21.21565077533257337, 4.556159429511043690, -1.500000000000002220 ) ) ;
#42042 = CARTESIAN_POINT ( 'NONE',  ( -84.52287095715010423, -23.73934037231757443, 11.05740245334329153 ) ) ;
#42043 = CIRCLE ( 'NONE', #1539, 2.040000000000001368 ) ;
#42044 = CARTESIAN_POINT ( 'NONE',  ( 14.87128047407919951, 12.67365258641725312, -1.500000000000002220 ) ) ;
#42045 = CARTESIAN_POINT ( 'NONE',  ( -93.52287095715011844, -24.51283580621364067, 0.6167428607019835862 ) ) ;
#42046 = ORIENTED_EDGE ( 'NONE', *, *, #93972, .T. ) ;
#42047 = AXIS2_PLACEMENT_3D ( 'NONE', #12976, #19594, #42462 ) ;
#42048 = CALENDAR_DATE ( 2026, 9, 10 ) ;
#42049 = VECTOR ( 'NONE', #91442, 1000.000000000000114 ) ;
#42050 = DIRECTION ( 'NONE',  ( -3.773278334453080206E-23, 0.9999999999976377785, 2.173523156925979975E-06 ) ) ;
#42051 = CARTESIAN_POINT ( 'NONE',  ( -20.22731604866883970, -2.807383831903240257, 11.49999999999999645 ) ) ;
#42052 = DIRECTION ( 'NONE',  ( -3.773278334453079030E-23, 0.9999999999976377785, 2.173523156925979128E-06 ) ) ;
#42053 = PLANE ( 'NONE',  #85341 ) ;
#42054 = AXIS2_PLACEMENT_3D ( 'NONE', #9392, #29111, #60086 ) ;
#42055 = EDGE_LOOP ( 'NONE', ( #31236, #64454, #13636, #3108 ) ) ;
#42056 = CARTESIAN_POINT ( 'NONE',  ( 8.160000000000000142, -9.870548898049497311, 1.288651800197855746 ) ) ;
#42057 = CARTESIAN_POINT ( 'NONE',  ( -39.44943695351214785, -25.28892596830959505, 4.097884984622077731 ) ) ;
#42058 = FACE_OUTER_BOUND ( 'NONE', #75813, .T. ) ;
#42059 = FACE_OUTER_BOUND ( 'NONE', #33310, .T. ) ;
#42060 = ORIENTED_EDGE ( 'NONE', *, *, #28431, .F. ) ;
#42061 = LINE ( 'NONE', #94323, #54437 ) ;
#42062 = ADVANCED_FACE ( 'NONE', ( #43785 ), #89455, .F. ) ;
#42063 = CARTESIAN_POINT ( 'NONE',  ( -18.54830753475928518, 13.48922247889305837, 11.49999999999999645 ) ) ;
#42064 = CARTESIAN_POINT ( 'NONE',  ( 2.720868037236281012, -22.60253418658637869, -1.500000000000002220 ) ) ;
#42065 = CARTESIAN_POINT ( 'NONE',  ( 4.638796026491669444, -6.376774720514424288, 21.40644651702305268 ) ) ;
#42066 = CARTESIAN_POINT ( 'NONE',  ( 33.61713288457014670, 3.416362262365323144, -11.96006463429725564 ) ) ;
#42067 = CARTESIAN_POINT ( 'NONE',  ( -90.58606721154154684, -24.73486907724917572, 1.287355809206966573 ) ) ;
#42068 = CARTESIAN_POINT ( 'NONE',  ( -74.52287095715010423, -24.35013146730203815, 9.818937971375095941 ) ) ;
#42069 = CARTESIAN_POINT ( 'NONE',  ( -69.86226356453386188, -25.11033435731149055, 2.832404375966413479 ) ) ;
#42070 = CARTESIAN_POINT ( 'NONE',  ( -20.59625928752216240, -7.366027188055905839, 11.49999999999998934 ) ) ;
#42071 = EDGE_CURVE ( 'NONE', #57281, #5782, #35177, .T. ) ;
#42072 = CARTESIAN_POINT ( 'NONE',  ( -7.160000000000000142, -5.907068460905239425E-16, 5.788828319098143105 ) ) ;
#42073 = EDGE_CURVE ( 'NONE', #96286, #33243, #50568, .T. ) ;
#42074 = CARTESIAN_POINT ( 'NONE',  ( -26.09950754783970339, -24.95550736417008508, 4.652252430823455853 ) ) ;
#42075 = CARTESIAN_POINT ( 'NONE',  ( -71.70841769935766763, -25.24715640642683923, 6.192981443001071895 ) ) ;
#42076 = CARTESIAN_POINT ( 'NONE',  ( -58.50334559872716511, -24.15543982623907482, -0.2315651400026660645 ) ) ;
#42077 = ORIENTED_EDGE ( 'NONE', *, *, #47858, .F. ) ;
#42078 = CARTESIAN_POINT ( 'NONE',  ( -19.05221060042639536, -7.346018566486852031, 11.49999999999998934 ) ) ;
#42079 = VERTEX_POINT ( 'NONE', #19932 ) ;
#42080 = ORIENTED_EDGE ( 'NONE', *, *, #9310, .F. ) ;
#42081 = VERTEX_POINT ( 'NONE', #97064 ) ;
#42082 = CARTESIAN_POINT ( 'NONE',  ( -1.485350438481424895, -22.96994831426971828, 11.49999999999998934 ) ) ;
#42083 = LINE ( 'NONE', #89743, #42196 ) ;
#42084 = CARTESIAN_POINT ( 'NONE',  ( 20.15506735835773000, -1.303320585059813741, -1.500000000000002220 ) ) ;
#42085 = ORIENTED_EDGE ( 'NONE', *, *, #19206, .F. ) ;
#42086 = CARTESIAN_POINT ( 'NONE',  ( -24.90875734969025501, 3.316774720514426456, 27.45402280011862572 ) ) ;
#42087 = LINE ( 'NONE', #50687, #6100 ) ;
#42088 = DIRECTION ( 'NONE',  ( 0.000000000000000000, 0.000000000000000000, -1.000000000000000000 ) ) ;
#42089 = CARTESIAN_POINT ( 'NONE',  ( -123.5895376238167245, -23.47593901973091235, -1.443836447538997536 ) ) ;
#42091 = ORIENTED_EDGE ( 'NONE', *, *, #23043, .F. ) ;
#42090 = CARTESIAN_POINT ( 'NONE',  ( 16.24497012180664868, 13.92215130028523973, 11.49999999999999645 ) ) ;
#42092 = DIRECTION ( 'NONE',  ( 0.7296913851534244655, -1.486204343759023298E-06, 0.6837766319717778485 ) ) ;
#42093 = EDGE_LOOP ( 'NONE', ( #11917, #46189, #51839, #86553, #36506, #19471, #81272, #97726 ) ) ;
#42094 = CARTESIAN_POINT ( 'NONE',  ( -7.755428854246955161, -20.87388092083558888, 11.49999999999998934 ) ) ;
#42095 = CARTESIAN_POINT ( 'NONE',  ( 12.06641648444584369, 16.80774221200798735, -1.500000000000002220 ) ) ;
#42096 = VECTOR ( 'NONE', #57418, 1000.000000000000000 ) ;
#42097 = EDGE_CURVE ( 'NONE', #27790, #16362, #10674, .T. ) ;
#42098 = B_SPLINE_CURVE_WITH_KNOTS ( 'NONE', 3,
 ( #48837, #4154, #81770, #65577 ),
 .UNSPECIFIED., .F., .F.,
 ( 4, 4 ),
 ( 0.000000000000000000, 9.999999999999592548E-05 ),
 .UNSPECIFIED. ) ;
#42099 = ORIENTED_EDGE ( 'NONE', *, *, #67550, .T. ) ;
#42100 = CARTESIAN_POINT ( 'NONE',  ( -5.850750514176234596, -5.876774720514411854, 19.74039977944280366 ) ) ;
#42101 = CARTESIAN_POINT ( 'NONE',  ( -68.92786316032828609, -25.03707830618030172, 7.590867772707288630 ) ) ;
#42102 = ORIENTED_EDGE ( 'NONE', *, *, #68237, .F. ) ;
#42103 = CARTESIAN_POINT ( 'NONE',  ( -81.52287095715007581, -24.51283580621452884, 0.6167428607046336886 ) ) ;
#42104 = VERTEX_POINT ( 'NONE', #81841 ) ;
#42105 = CARTESIAN_POINT ( 'NONE',  ( 9.016989526679575206, 6.475225279485574248, -27.05137190084761301 ) ) ;
#42106 = CARTESIAN_POINT ( 'NONE',  ( 2.313481123293766206, -20.83243486019555135, -1.500000000000002220 ) ) ;
#42107 = B_SPLINE_CURVE_WITH_KNOTS ( 'NONE', 3,
 ( #83688, #36017, #53758, #46140, #83181, #13665 ),
 .UNSPECIFIED., .F., .F.,
 ( 4, 2, 4 ),
 ( 0.000000000000000000, 0.001380901958385383124, 0.002761803916770766247 ),
 .UNSPECIFIED. ) ;
#42108 = CARTESIAN_POINT ( 'NONE',  ( -16.46405638241306946, -14.47283864684382237, 11.49999999999999645 ) ) ;
#42109 = CARTESIAN_POINT ( 'NONE',  ( -73.53860178212968890, -24.66019654487200441, 8.947790411086119278 ) ) ;
#42110 = CARTESIAN_POINT ( 'NONE',  ( -1.726696889551340153, 22.42386595106472669, 11.49999999999998934 ) ) ;
#42111 = EDGE_CURVE ( 'NONE', #73872, #71528, #40859, .T. ) ;
#42112 = VECTOR ( 'NONE', #88038, 1000.000000000000000 ) ;
#42113 = EDGE_CURVE ( 'NONE', #78770, #59659, #29042, .T. ) ;
#42114 = CARTESIAN_POINT ( 'NONE',  ( 19.95448254803897115, -6.385634049875297258, 11.49999999999998934 ) ) ;
#42115 = CARTESIAN_POINT ( 'NONE',  ( -27.70544111104076990, -29.50248652753305478, 1.628739237965270537 ) ) ;
#42116 = CARTESIAN_POINT ( 'NONE',  ( -108.8968792378192063, -25.12726808145882629, 7.140617874877389859 ) ) ;
#42117 = CARTESIAN_POINT ( 'NONE',  ( -91.55620429048339304, -24.64965694238574656, 8.947790433994201820 ) ) ;
#42118 = ORIENTED_EDGE ( 'NONE', *, *, #2219, .F. ) ;
#42119 = CIRCLE ( 'NONE', #25939, 1.835999999999993859 ) ;
#42120 = EDGE_CURVE ( 'NONE', #67426, #12600, #82335, .T. ) ;
#42121 = ORIENTED_EDGE ( 'NONE', *, *, #71711, .F. ) ;
#42122 = AXIS2_PLACEMENT_3D ( 'NONE', #74099, #88828, #2596 ) ;
#42123 = ORIENTED_EDGE ( 'NONE', *, *, #94048, .F. ) ;
#42124 = CARTESIAN_POINT ( 'NONE',  ( -52.54749795293748349, -24.15543982623907482, -0.2315651400026529916 ) ) ;
#42125 = ORIENTED_EDGE ( 'NONE', *, *, #31146, .F. ) ;
#42126 = B_SPLINE_CURVE_WITH_KNOTS ( 'NONE', 3,
 ( #87481, #49438, #40804, #73267 ),
 .UNSPECIFIED., .F., .F.,
 ( 4, 4 ),
 ( 0.000000000000000000, 0.0001000000000000028644 ),
 .UNSPECIFIED. ) ;
#42127 = AXIS2_PLACEMENT_3D ( 'NONE', #66095, #34625, #43240 ) ;
#42128 = CARTESIAN_POINT ( 'NONE',  ( -12.70309173801008562, -17.24390854791867511, -1.500000000000002220 ) ) ;
#42129 = VERTEX_POINT ( 'NONE', #90448 ) ;
#42130 = CARTESIAN_POINT ( 'NONE',  ( -26.19055979656421584, -24.92561770071717930, 6.008896093053317067 ) ) ;
#42131 = CARTESIAN_POINT ( 'NONE',  ( 20.24497096899912307, 5.935080660949433096, 11.49999999999998934 ) ) ;
#42132 = CARTESIAN_POINT ( 'NONE',  ( -30.61623571243587349, -24.27934583723679651, 9.960304333224314632 ) ) ;
#42133 = CARTESIAN_POINT ( 'NONE',  ( 2.832419239133125544, -6.376774720514422512, 21.23415460623727213 ) ) ;
#42134 = CARTESIAN_POINT ( 'NONE',  ( -97.22287095715006444, -23.47596703998600631, 11.44779298504227860 ) ) ;
#42135 = CARTESIAN_POINT ( 'NONE',  ( -80.35919894935767616, -25.30877072896627666, 4.505481309076929897 ) ) ;
#42136 = CARTESIAN_POINT ( 'NONE',  ( -129.5899315912527356, -23.73791477778912906, 11.05961554403170233 ) ) ;
#42137 = CARTESIAN_POINT ( 'NONE',  ( 2.156995527713877259, 21.93451973775924557, -1.500000000000002220 ) ) ;
#42138 = VERTEX_POINT ( 'NONE', #12812 ) ;
#42139 = CARTESIAN_POINT ( 'NONE',  ( -65.53230649573079347, -24.92592662359560762, 8.075495903017996469 ) ) ;
#42140 = EDGE_CURVE ( 'NONE', #96582, #49194, #17851, .T. ) ;
#42141 = CARTESIAN_POINT ( 'NONE',  ( 9.450000000000002842, -2.000000000000001332, 24.00000000000000000 ) ) ;
#42142 = CARTESIAN_POINT ( 'NONE',  ( -40.76794460738368997, -25.27956066610283870, 5.521532736733258950 ) ) ;
#42143 = CARTESIAN_POINT ( 'NONE',  ( -62.61045561229671108, -23.48786465467241413, 11.44779295918255002 ) ) ;
#42144 = CARTESIAN_POINT ( 'NONE',  ( -26.57444913475580250, -24.61859514035917584, 1.999156410758380575 ) ) ;
#42145 = CARTESIAN_POINT ( 'NONE',  ( -102.5895376238167245, -23.47593901973091235, -1.443836447539001089 ) ) ;
#42146 = CARTESIAN_POINT ( 'NONE',  ( 21.34331307443176584, 0.5271963136488534429, -1.500000000000002220 ) ) ;
#42147 = FACE_OUTER_BOUND ( 'NONE', #100337, .T. ) ;
#42148 = CARTESIAN_POINT ( 'NONE',  ( -50.92004226540860401, -25.20650842489795451, 6.812665538484691474 ) ) ;
#42149 = ADVANCED_FACE ( 'NONE', ( #52392 ), #74229, .T. ) ;
#42150 = CARTESIAN_POINT ( 'NONE',  ( -0.1490749075164066184, -21.12010817310450861, 11.44779298504228038 ) ) ;
#42151 = DIRECTION ( 'NONE',  ( 1.000000000000000000, 0.000000000000000000, -0.000000000000000000 ) ) ;
#42152 = CARTESIAN_POINT ( 'NONE',  ( -3.174168706971715270, 22.36591850054903929, -1.500000000000002220 ) ) ;
#42153 = EDGE_CURVE ( 'NONE', #28343, #25435, #45710, .T. ) ;
#42154 = PLANE ( 'NONE',  #58780 ) ;
#42155 = VERTEX_POINT ( 'NONE', #53115 ) ;
#42156 = PLANE ( 'NONE',  #35304 ) ;
#42157 = CARTESIAN_POINT ( 'NONE',  ( -79.64187532455639484, -23.73766607897669800, -1.055555164236459564 ) ) ;
#42158 = CARTESIAN_POINT ( 'NONE',  ( -10.80270875523330965, -16.48872379891551532, 11.49999999999999645 ) ) ;
#42159 = CARTESIAN_POINT ( 'NONE',  ( -32.07722060962684196, -24.87479601683932984, 8.247789944617052171 ) ) ;
#42160 = LINE ( 'NONE', #65504, #96578 ) ;
#42161 = ORIENTED_EDGE ( 'NONE', *, *, #73259, .F. ) ;
#42162 = EDGE_CURVE ( 'NONE', #39424, #5922, #75423, .T. ) ;
#42163 = CARTESIAN_POINT ( 'NONE',  ( -7.641025641025640525, -6.376774720514417183, 20.36458333333334281 ) ) ;
#42164 = CARTESIAN_POINT ( 'NONE',  ( -29.12854162637831834, -25.26026429949986607, 2.289899196687330551 ) ) ;
#42165 = CARTESIAN_POINT ( 'NONE',  ( -101.1189062734182755, -25.17353303595478664, 6.916461067677506236 ) ) ;
#42166 = CARTESIAN_POINT ( 'NONE',  ( 7.158504886898216846, -20.39052948596947346, -1.500000000000002220 ) ) ;
#42167 = CARTESIAN_POINT ( 'NONE',  ( -11.16000000000000014, -10.65233964170348635, 1.628518864987183790 ) ) ;
#42168 = CARTESIAN_POINT ( 'NONE',  ( -13.40542139710017899, 13.98966777563825481, -1.500000000000002220 ) ) ;
#42169 = ADVANCED_FACE ( 'NONE', ( #28768 ), #68830, .F. ) ;
#42170 = CARTESIAN_POINT ( 'NONE',  ( 27.86270917940689174, -0.3587747205144265483, 29.49402280011862487 ) ) ;
#42171 = DIRECTION ( 'NONE',  ( -3.773278334453079618E-23, 0.9999999999976377785, 2.173523156925978705E-06 ) ) ;
#42172 = CARTESIAN_POINT ( 'NONE',  ( -15.09475962229707591, 12.77647934908296712, -1.500000000000002220 ) ) ;
#42173 = EDGE_LOOP ( 'NONE', ( #142, #51094, #87716, #91726 ) ) ;
#42174 = CARTESIAN_POINT ( 'NONE',  ( 20.23688964843749005, 1.552196809742036221, 11.49999999999999645 ) ) ;
#42175 = CARTESIAN_POINT ( 'NONE',  ( -5.366453405989236813, 0.000000000000000000, 0.000000000000000000 ) ) ;
#42176 = AXIS2_PLACEMENT_3D ( 'NONE', #11371, #34711, #65685 ) ;
#42177 = ORIENTED_EDGE ( 'NONE', *, *, #68320, .F. ) ;
#42178 = CARTESIAN_POINT ( 'NONE',  ( 32.53135143123563466, -0.3587747205144265483, 6.926385399448451885 ) ) ;
#42179 = CARTESIAN_POINT ( 'NONE',  ( -19.77875734969026311, -6.143225279485574397, 27.35402280011862430 ) ) ;
#42180 = LINE ( 'NONE', #47776, #15295 ) ;
#42181 = DIRECTION ( 'NONE',  ( -0.9997753877537052247, 0.000000000000000000, 0.02119372647573814633 ) ) ;
#42182 = VECTOR ( 'NONE', #5629, 1000.000000000000000 ) ;
#42183 = CARTESIAN_POINT ( 'NONE',  ( -105.5228709571500758, -29.50247984919015209, -1.443849546365048253 ) ) ;
#42184 = B_SPLINE_CURVE_WITH_KNOTS ( 'NONE', 3,
 ( #64729, #100347, #86151, #41874 ),
 .UNSPECIFIED., .F., .F.,
 ( 4, 4 ),
 ( 3.973137263842166252E-09, 0.0004615443969624879301 ),
 .UNSPECIFIED. ) ;
#42185 = CARTESIAN_POINT ( 'NONE',  ( -71.62287095715005592, -23.47593901973091235, -1.443836447539006196 ) ) ;
#42186 = CARTESIAN_POINT ( 'NONE',  ( 9.011679573027636891, 17.89655708981447901, 11.49999999999998934 ) ) ;
#42187 = FACE_OUTER_BOUND ( 'NONE', #11797, .T. ) ;
#42188 = VECTOR ( 'NONE', #82719, 1000.000000000000114 ) ;
#42189 = ORIENTED_EDGE ( 'NONE', *, *, #7495, .T. ) ;
#42190 = VECTOR ( 'NONE', #5541, 1000.000000000000000 ) ;
#42191 = EDGE_CURVE ( 'NONE', #73900, #22592, #51612, .T. ) ;
#42192 = VECTOR ( 'NONE', #86165, 1000.000000000000000 ) ;
#42193 = DIRECTION ( 'NONE',  ( -0.9913618264504691080, 0.000000000000000000, 0.1311553622875927805 ) ) ;
#42194 = CARTESIAN_POINT ( 'NONE',  ( 2.499999999999995115, 19.99999999999999645, 2.100000000000000089 ) ) ;
#42195 = DIRECTION ( 'NONE',  ( -0.000000000000000000, -1.000000000000000000, -0.000000000000000000 ) ) ;
#42196 = VECTOR ( 'NONE', #95851, 1000.000000000000114 ) ;
#42197 = CARTESIAN_POINT ( 'NONE',  ( -105.5228709571500900, -24.82558206586144678, 1.605769216559448598 ) ) ;
#42198 = CARTESIAN_POINT ( 'NONE',  ( 8.160000000000000142, -10.15233964170348457, 0.003711184059992174607 ) ) ;
#42199 = AXIS2_PLACEMENT_3D ( 'NONE', #3558, #65477, #53228 ) ;
#42200 = CARTESIAN_POINT ( 'NONE',  ( 14.52861783435592713, 3.922795597835279313, -28.30212872328009510 ) ) ;
#42201 = EDGE_CURVE ( 'NONE', #96767, #26965, #38369, .T. ) ;
#42202 = CARTESIAN_POINT ( 'NONE',  ( -50.02370822792538974, -25.23256535379771037, 6.480020017899467355 ) ) ;
#42203 = VERTEX_POINT ( 'NONE', #97773 ) ;
#42204 = CARTESIAN_POINT ( 'NONE',  ( -8.236308187080631171, 18.58821751820538637, -1.500000000000002220 ) ) ;
#42205 = VERTEX_POINT ( 'NONE', #84047 ) ;
#42206 = CARTESIAN_POINT ( 'NONE',  ( -5.713817535623205046, 22.21719745612757535, 11.49999999999998934 ) ) ;
#42207 = CARTESIAN_POINT ( 'NONE',  ( 31.67769140193662381, 4.988134948533209823, 28.98636546410035564 ) ) ;
#42208 = CARTESIAN_POINT ( 'NONE',  ( -127.5217000848324034, -23.96169478059714208, 10.65365249895716282 ) ) ;
#42209 = ORIENTED_EDGE ( 'NONE', *, *, #28124, .T. ) ;
#42210 = CARTESIAN_POINT ( 'NONE',  ( -49.13243839854418127, -25.28217150478232256, 4.246802725325826700 ) ) ;
#42211 = CARTESIAN_POINT ( 'NONE',  ( 14.71033543815184252, 3.370934240161822526, -27.37556158125726213 ) ) ;
#42212 = B_SPLINE_CURVE_WITH_KNOTS ( 'NONE', 3,
 ( #88719, #41554, #34928, #81100 ),
 .UNSPECIFIED., .F., .F.,
 ( 4, 4 ),
 ( 0.000000000000000000, 0.0008333333333333525772 ),
 .UNSPECIFIED. ) ;
#42213 = CARTESIAN_POINT ( 'NONE',  ( -30.47287095715008221, -23.78471427653590453, -0.9626557455456202783 ) ) ;
#42214 = CARTESIAN_POINT ( 'NONE',  ( -1.756177585742932479, 21.11346882147791959, 11.49999999999999645 ) ) ;
#42215 = CARTESIAN_POINT ( 'NONE',  ( -13.50798789833325664, 17.53495777034937220, -1.500000000000002220 ) ) ;
#42216 = CARTESIAN_POINT ( 'NONE',  ( 10.54205562766345672, -17.70522803435136083, 11.49999999999998934 ) ) ;
#42217 = ADVANCED_FACE ( 'NONE', ( #90662 ), #36878, .T. ) ;
#42218 = ORIENTED_EDGE ( 'NONE', *, *, #37906, .F. ) ;
#42219 = CARTESIAN_POINT ( 'NONE',  ( -107.5228709571500758, -24.64898659630367916, 1.056161002820831474 ) ) ;
#42220 = ORIENTED_EDGE ( 'NONE', *, *, #78206, .F. ) ;
#42221 = CARTESIAN_POINT ( 'NONE',  ( -54.59313660317440053, -24.15543982623906416, -0.2315651400026691176 ) ) ;
#42222 = CARTESIAN_POINT ( 'NONE',  ( 2.611202098145462891, -5.876774720514419847, 20.45574432200782766 ) ) ;
#42223 = ORIENTED_EDGE ( 'NONE', *, *, #73199, .F. ) ;
#42224 = EDGE_LOOP ( 'NONE', ( #67507, #29591, #32621, #80947 ) ) ;
#42225 = ORIENTED_EDGE ( 'NONE', *, *, #94312, .F. ) ;
#42226 = LINE ( 'NONE', #19357, #8110 ) ;
#42227 = CARTESIAN_POINT ( 'NONE',  ( -46.52287095715007581, -23.47593901973090524, -1.443836447538997314 ) ) ;
#42228 = LINE ( 'NONE', #49837, #22803 ) ;
#42229 = CARTESIAN_POINT ( 'NONE',  ( 20.64725891757762355, 2.036748910689437864, -1.500000000000002220 ) ) ;
#42230 = CARTESIAN_POINT ( 'NONE',  ( -19.25911440464646063, 10.06369110047026538, 11.49999999999999645 ) ) ;
#42231 = ORIENTED_EDGE ( 'NONE', *, *, #76044, .F. ) ;
#42232 = B_SPLINE_CURVE_WITH_KNOTS ( 'NONE', 3,
 ( #75942, #83558, #7434, #29280 ),
 .UNSPECIFIED., .F., .F.,
 ( 4, 4 ),
 ( 1.387778780781445676E-17, 0.0001000000000000028508 ),
 .UNSPECIFIED. ) ;
#42233 = ADVANCED_FACE ( 'NONE', ( #99748 ), #30251, .F. ) ;
#42234 = DIRECTION ( 'NONE',  ( 1.000000000000000000, -0.000000000000000000, 0.000000000000000000 ) ) ;
#42235 = CARTESIAN_POINT ( 'NONE',  ( -111.7814946224345789, -25.28710546256127145, 4.332404433089555695 ) ) ;
#42236 = CARTESIAN_POINT ( 'NONE',  ( 19.55810785529653373, 10.91776788121007868, -1.500000000000002220 ) ) ;
#42237 = EDGE_CURVE ( 'NONE', #92752, #503, #73381, .T. ) ;
#42238 = ADVANCED_FACE ( 'NONE', ( #75924 ), #76917, .F. ) ;
#42239 = DIRECTION ( 'NONE',  ( -0.000000000000000000, 0.000000000000000000, -1.000000000000000000 ) ) ;
#42240 = DIRECTION ( 'NONE',  ( -0.1311553622875919756, 0.000000000000000000, -0.9913618264504692190 ) ) ;
#42241 = ORIENTED_EDGE ( 'NONE', *, *, #55190, .F. ) ;
#42242 = CARTESIAN_POINT ( 'NONE',  ( -8.160000000000000142, -10.15233964170348457, 0.003711184059992174607 ) ) ;
#42243 = FACE_OUTER_BOUND ( 'NONE', #22325, .T. ) ;
#42244 = ADVANCED_FACE ( 'NONE', ( #20643 ), #5427, .T. ) ;
#42245 = VERTEX_POINT ( 'NONE', #98261 ) ;
#42246 = MANIFOLD_SOLID_BREP ( 'Radyus1', #35477 ) ;
#42247 = VERTEX_POINT ( 'NONE', #29259 ) ;
#42248 = AXIS2_PLACEMENT_3D ( 'NONE', #73426, #34858, #49099 ) ;
#42249 = CARTESIAN_POINT ( 'NONE',  ( -69.62287095715005592, -23.73934037231756733, 11.05740245334329330 ) ) ;
#42250 = EDGE_LOOP ( 'NONE', ( #10637, #6126, #80042, #44423 ) ) ;
#42251 = CARTESIAN_POINT ( 'NONE',  ( 14.73992482348874411, 15.29747818672187165, -1.500000000000002220 ) ) ;
#42252 = ORIENTED_EDGE ( 'NONE', *, *, #32587, .T. ) ;
#42253 = CARTESIAN_POINT ( 'NONE',  ( -100.5774747013531822, -25.12365577940056482, 7.097838394941334172 ) ) ;
#42254 = CARTESIAN_POINT ( 'NONE',  ( 3.337383349182757364, -21.60657791699550856, 11.49999999999998934 ) ) ;
#42255 = DIRECTION ( 'NONE',  ( 0.000000000000000000, 0.9999999999976377785, 2.173523156925979975E-06 ) ) ;
#42256 = CARTESIAN_POINT ( 'NONE',  ( 6.660000000000001030, 0.000000000000000000, 0.000000000000000000 ) ) ;
#42257 = PLANE ( 'NONE',  #82196 ) ;
#42258 = CARTESIAN_POINT ( 'NONE',  ( 21.44370820036873937, 4.193779532373530294, -1.500000000000002220 ) ) ;
#42259 = CARTESIAN_POINT ( 'NONE',  ( 7.111284305517425075, -5.876774720514421624, 21.05363841023157434 ) ) ;
#42260 = ORIENTED_EDGE ( 'NONE', *, *, #16319, .T. ) ;
#42261 = DIRECTION ( 'NONE',  ( 0.000000000000000000, -0.000000000000000000, -1.000000000000000000 ) ) ;
#42263 = EDGE_CURVE ( 'NONE', #86407, #89859, #25027, .T. ) ;
#42262 = DIRECTION ( 'NONE',  ( 0.000000000000000000, 0.000000000000000000, -1.000000000000000000 ) ) ;
#42264 = EDGE_CURVE ( 'NONE', #99862, #56477, #80754, .T. ) ;
#42265 = VERTEX_POINT ( 'NONE', #40378 ) ;
#42266 = CARTESIAN_POINT ( 'NONE',  ( -30.62525681927276011, -24.05323539164308855, 10.46343928437834414 ) ) ;
#42267 = AXIS2_PLACEMENT_3D ( 'NONE', #23383, #47252, #52861 ) ;
#42268 = ORIENTED_EDGE ( 'NONE', *, *, #353, .T. ) ;
#42269 = CARTESIAN_POINT ( 'NONE',  ( 30.53060340732036693, -4.905826575867056505, 14.32820694822485841 ) ) ;
#42270 = AXIS2_PLACEMENT_3D ( 'NONE', #79639, #72052, #10134 ) ;
#42271 = CARTESIAN_POINT ( 'NONE',  ( -30.61630412665073919, -24.37835529153250747, 0.3010598746230513933 ) ) ;
#42272 = CARTESIAN_POINT ( 'NONE',  ( -15.93125441714207646, -14.09135727244061265, 11.49999999999998934 ) ) ;
#42273 = DIRECTION ( 'NONE',  ( 1.000000000000000000, 3.773278334444167608E-23, 8.201307833595939069E-29 ) ) ;
#42274 = DIRECTION ( 'NONE',  ( -0.000000000000000000, 1.000000000000000000, -0.000000000000000000 ) ) ;
#42275 = ADVANCED_FACE ( 'NONE', ( #69322 ), #15525, .F. ) ;
#42276 = CARTESIAN_POINT ( 'NONE',  ( -85.52211224428006631, -23.48783264082476308, -1.443836473390098796 ) ) ;
#42277 = CARTESIAN_POINT ( 'NONE',  ( 33.10875634548599322, -5.965225279485572685, -11.42349945801155719 ) ) ;
#42278 = AXIS2_PLACEMENT_3D ( 'NONE', #41141, #93905, #80191 ) ;
#42279 = CARTESIAN_POINT ( 'NONE',  ( -16.98888496755095545, 9.415225082695979353, -1.500000000000002220 ) ) ;
#42280 = CARTESIAN_POINT ( 'NONE',  ( -117.5527607394227090, -24.51419770103158768, 9.386484678747166299 ) ) ;
#42281 = VERTEX_POINT ( 'NONE', #32758 ) ;
#42282 = CARTESIAN_POINT ( 'NONE',  ( -16.69004703121433408, -10.21020960635683394, 11.49999999999999645 ) ) ;
#42283 = CARTESIAN_POINT ( 'NONE',  ( -81.62287095715008434, -23.47596703998600631, 11.44779298504227860 ) ) ;
#42284 = CARTESIAN_POINT ( 'NONE',  ( -29.36005952620050863, -24.99996101429923812, 7.263710429510505939 ) ) ;
#42285 = ORIENTED_EDGE ( 'NONE', *, *, #38290, .T. ) ;
#42286 = EDGE_CURVE ( 'NONE', #63089, #89004, #93145, .T. ) ;
#42287 = CARTESIAN_POINT ( 'NONE',  ( -117.5228709571500758, -23.95044443724993144, 10.65354141964648882 ) ) ;
#42288 = CARTESIAN_POINT ( 'NONE',  ( -47.52287095715007581, -23.47593901973090169, -1.443836447538997092 ) ) ;
#42290 = EDGE_CURVE ( 'NONE', #87149, #56850, #100243, .T. ) ;
#42289 = CARTESIAN_POINT ( 'NONE',  ( -90.52287095715004739, -24.52232992886363405, 0.6492154411906000400 ) ) ;
#42291 = CARTESIAN_POINT ( 'NONE',  ( -88.62287095715004170, -23.48783264082479150, -1.443836473390063935 ) ) ;
#42292 = CARTESIAN_POINT ( 'NONE',  ( 18.75866648459458830, -6.009157199652424453, 11.49999999999998934 ) ) ;
#42293 = EDGE_CURVE ( 'NONE', #79556, #62504, #5616, .T. ) ;
#42294 = EDGE_LOOP ( 'NONE', ( #25741, #100030, #26578, #45003 ) ) ;
#42295 = CARTESIAN_POINT ( 'NONE',  ( -94.62287095715002749, -23.94994826722566117, -0.6494450866342748041 ) ) ;
#42296 = CARTESIAN_POINT ( 'NONE',  ( 30.58729439590577570, -4.540774720514427543, 26.14186284044645703 ) ) ;
#42297 = COORDINATED_UNIVERSAL_TIME_OFFSET ( 0, 0, .AHEAD. ) ;
#42298 = VERTEX_POINT ( 'NONE', #31255 ) ;
#42299 = LINE ( 'NONE', #73228, #61376 ) ;
#42300 = CARTESIAN_POINT ( 'NONE',  ( 9.543201319291914093E-14, -5.876774720514426953, 18.21871304725679508 ) ) ;
#42301 = CARTESIAN_POINT ( 'NONE',  ( -69.62287095715004170, -24.33832256526968862, 0.1851278514119857332 ) ) ;
#42302 = DIRECTION ( 'NONE',  ( -0.6392559695863496705, 6.845827386180411947E-16, -0.7689940216596069522 ) ) ;
#42303 = CARTESIAN_POINT ( 'NONE',  ( -81.90695487689731635, -25.03722721891040948, 7.590183713343859218 ) ) ;
#42304 = DIRECTION ( 'NONE',  ( -1.000000000000000000, -0.000000000000000000, -7.994117400814786717E-16 ) ) ;
#42305 = CARTESIAN_POINT ( 'NONE',  ( -79.52287095715004739, -23.48783264082476663, -1.443836473390090358 ) ) ;
#42306 = CARTESIAN_POINT ( 'NONE',  ( 19.92730240972663935, 0.8534881809820089593, -1.500000000000002220 ) ) ;
#42307 = CARTESIAN_POINT ( 'NONE',  ( -0.08206578796906692508, -21.98759388411814086, 10.03296377820838892 ) ) ;
#42308 = CARTESIAN_POINT ( 'NONE',  ( -13.97081141688431138, 14.13901428111770819, -1.500000000000002220 ) ) ;
#42309 = ORIENTED_EDGE ( 'NONE', *, *, #44779, .F. ) ;
#42310 = CARTESIAN_POINT ( 'NONE',  ( -71.52287095715007581, -24.33832256527048798, 0.1851278514138584019 ) ) ;
#42311 = CARTESIAN_POINT ( 'NONE',  ( -29.52287095715004739, -23.65317350716957279, 11.05752279813568251 ) ) ;
#42312 = CARTESIAN_POINT ( 'NONE',  ( -80.62364780861474856, -25.00182538069147142, 7.747789668545041586 ) ) ;
#42313 = CARTESIAN_POINT ( 'NONE',  ( 6.705275102110877405, 19.67741782454948662, 11.49999999999999645 ) ) ;
#42314 = CARTESIAN_POINT ( 'NONE',  ( -36.22287095715005734, -23.47593901973090169, -1.443836447538998202 ) ) ;
#42315 = AXIS2_PLACEMENT_3D ( 'NONE', #91657, #90173, #76920 ) ;
#42316 = PLANE ( 'NONE',  #30771 ) ;
#42317 = CARTESIAN_POINT ( 'NONE',  ( -0.7673284989158746239, 22.82873350090251918, 11.49999999999999645 ) ) ;
#42318 = ORIENTED_EDGE ( 'NONE', *, *, #88664, .T. ) ;
#42319 = CARTESIAN_POINT ( 'NONE',  ( 30.09341516180546350, -1.682774720514426114, -13.09311774897855862 ) ) ;
#42320 = CARTESIAN_POINT ( 'NONE',  ( -38.52287095715006870, -23.73907113217726916, -1.053371485780264294 ) ) ;
#42321 = ORIENTED_EDGE ( 'NONE', *, *, #42290, .T. ) ;
#42322 = CARTESIAN_POINT ( 'NONE',  ( 12.36038202409810438, -16.04522380935875248, 11.49999999999998934 ) ) ;
#42323 = CARTESIAN_POINT ( 'NONE',  ( 7.072045900997899537, -5.876774720514427841, 21.62824307385093192 ) ) ;
#42324 = CARTESIAN_POINT ( 'NONE',  ( 7.462166178408539352, 6.475225279485573360, -27.67315496249664974 ) ) ;
#42325 = CARTESIAN_POINT ( 'NONE',  ( 26.74698519091204574, -1.477225279485574028, -10.98683230472873973 ) ) ;
#42326 = EDGE_LOOP ( 'NONE', ( #61706, #18805, #72674, #93633 ) ) ;
#42327 = PLANE ( 'NONE',  #4715 ) ;
#42328 = CARTESIAN_POINT ( 'NONE',  ( -51.62287095715004881, -23.73907113216990084, -1.053371485793233475 ) ) ;
#42329 = AXIS2_PLACEMENT_3D ( 'NONE', #36280, #67239, #99641 ) ;
#42330 = CARTESIAN_POINT ( 'NONE',  ( 17.67427751897593069, 9.450557017276361549, -1.500000000000002220 ) ) ;
#42331 = CARTESIAN_POINT ( 'NONE',  ( -19.96636262075925927, 6.592627302904066511, 11.49999999999999645 ) ) ;
#42332 = DIRECTION ( 'NONE',  ( 1.700709290173338723E-14, 0.000000000000000000, 1.000000000000000000 ) ) ;
#42333 = CARTESIAN_POINT ( 'NONE',  ( -124.6228709571500559, -24.64965695001469115, 8.947790433994175174 ) ) ;
#42334 = CARTESIAN_POINT ( 'NONE',  ( 21.95769793831392036, 2.030053023538682222, 11.49999999999998934 ) ) ;
#42335 = CARTESIAN_POINT ( 'NONE',  ( 7.346158715828313923, 5.304593391634067068, -25.62898491049482885 ) ) ;
#42336 = ADVANCED_FACE ( 'NONE', ( #8422 ), #45137, .T. ) ;
#42337 = CARTESIAN_POINT ( 'NONE',  ( -81.88534077628074215, -29.50249666744127808, 6.293933732382250845 ) ) ;
#42338 = DIRECTION ( 'NONE',  ( 0.000000000000000000, 0.000000000000000000, 1.000000000000000000 ) ) ;
#42339 = CARTESIAN_POINT ( 'NONE',  ( -72.62362975610302840, -24.65952944569304250, 1.056160979905695463 ) ) ;
#42340 = CARTESIAN_POINT ( 'NONE',  ( -31.50374477195024170, -23.96119346886880663, -0.6495511937832003646 ) ) ;
#42341 = ADVANCED_FACE ( 'NONE', ( #47492 ), #29731, .T. ) ;
#42342 = ORIENTED_EDGE ( 'NONE', *, *, #51036, .T. ) ;
#42343 = EDGE_CURVE ( 'NONE', #68827, #39091, #96135, .T. ) ;
#42344 = ORIENTED_EDGE ( 'NONE', *, *, #13267, .F. ) ;
#42345 = LINE ( 'NONE', #19472, #77761 ) ;
#42346 = CARTESIAN_POINT ( 'NONE',  ( -7.749999999999996447, 24.84999999999999787, 2.100000000000000089 ) ) ;
#42347 = DIRECTION ( 'NONE',  ( -3.773278334453080206E-23, 0.9999999999976377785, 2.173523156925979975E-06 ) ) ;
#42348 = CARTESIAN_POINT ( 'NONE',  ( -13.21525772315781388, 15.71049578022273785, -1.500000000000002220 ) ) ;
#42349 = EDGE_CURVE ( 'NONE', #75496, #28958, #49211, .T. ) ;
#42350 = EDGE_LOOP ( 'NONE', ( #89019, #11133, #88497, #12361 ) ) ;
#42351 = FACE_OUTER_BOUND ( 'NONE', #33302, .T. ) ;
#42352 = CARTESIAN_POINT ( 'NONE',  ( -10.23311166579590825, 4.222446552888387217, 29.28685113854110966 ) ) ;
#42353 = CARTESIAN_POINT ( 'NONE',  ( -83.52287095715004739, -23.96127896941631619, -0.6493128931038049112 ) ) ;
#42354 = CARTESIAN_POINT ( 'NONE',  ( 18.98964132805693694, -11.70494588174365092, -1.500000000000002220 ) ) ;
#42355 = EDGE_CURVE ( 'NONE', #48556, #27910, #38325, .T. ) ;
#42356 = ADVANCED_FACE ( 'NONE', ( #81443 ), #57617, .T. ) ;
#42357 = B_SPLINE_CURVE_WITH_KNOTS ( 'NONE', 3,
 ( #3709, #58006, #88938, #19415, #15172, #13288, #85188, #77063 ),
 .UNSPECIFIED., .F., .F.,
 ( 4, 2, 2, 4 ),
 ( 6.384118678608834355E-06, 0.002007151183507251049, 0.003007534715921573835, 0.004007918248335896189 ),
 .UNSPECIFIED. ) ;
#42358 = CARTESIAN_POINT ( 'NONE',  ( -47.52287095715004739, -24.66019654487199375, 8.947790411086122830 ) ) ;
#42359 = CARTESIAN_POINT ( 'NONE',  ( 13.60020833695035947, 0.000000000000000000, 1.249999999999999112 ) ) ;
#42360 = ORIENTED_EDGE ( 'NONE', *, *, #15121, .F. ) ;
#42361 = CARTESIAN_POINT ( 'NONE',  ( 33.62089986283198328, -3.615790004618635312, -11.40738377976237494 ) ) ;
#42362 = CARTESIAN_POINT ( 'NONE',  ( -47.92287095715007439, -23.47596703998600276, 11.44779298504227683 ) ) ;
#42363 = CARTESIAN_POINT ( 'NONE',  ( -20.60679684081203789, -3.318877370925724879, 11.49999999999998934 ) ) ;
#42364 = ORIENTED_EDGE ( 'NONE', *, *, #80875, .F. ) ;
#42366 = ORIENTED_EDGE ( 'NONE', *, *, #19334, .T. ) ;
#42365 = CARTESIAN_POINT ( 'NONE',  ( -39.04303308397305727, -25.28006866179717349, 4.215216948383927686 ) ) ;
#42367 = VERTEX_POINT ( 'NONE', #72336 ) ;
#42368 = DIRECTION ( 'NONE',  ( -0.000000000000000000, -0.000000000000000000, -1.000000000000000000 ) ) ;
#42369 = CARTESIAN_POINT ( 'NONE',  ( 9.758084087097168791, -18.66043984184860349, -1.500000000000002220 ) ) ;
#42370 = EDGE_LOOP ( 'NONE', ( #74319, #65067, #83762, #42493 ) ) ;
#42371 = CARTESIAN_POINT ( 'NONE',  ( -114.6228709571500701, -23.48783264082478794, -1.443836473390060382 ) ) ;
#42372 = CARTESIAN_POINT ( 'NONE',  ( 31.31283134548411340, -1.682774720514426114, -10.20862453625735533 ) ) ;
#42373 = CARTESIAN_POINT ( 'NONE',  ( -120.6267747408976874, -24.15602025860899360, 10.28564288303534902 ) ) ;
#42374 = CARTESIAN_POINT ( 'NONE',  ( -68.62287095715005592, -23.48786465467241058, 11.44779295918254647 ) ) ;
#42375 = B_SPLINE_CURVE_WITH_KNOTS ( 'NONE', 3,
 ( #45713, #7138, #38088, #69042 ),
 .UNSPECIFIED., .F., .F.,
 ( 4, 4 ),
 ( 0.000000000000000000, 0.0004038461538461851630 ),
 .UNSPECIFIED. ) ;
#42376 = CARTESIAN_POINT ( 'NONE',  ( 7.234974673537251100, -6.376774720514415407, 19.99114326857715795 ) ) ;
#42377 = CARTESIAN_POINT ( 'NONE',  ( 13.45394552336293614, 17.01807010946250287, -1.500000000000002220 ) ) ;
#42378 = FACE_OUTER_BOUND ( 'NONE', #26133, .T. ) ;
#42380 = ORIENTED_EDGE ( 'NONE', *, *, #79298, .T. ) ;
#42379 = CARTESIAN_POINT ( 'NONE',  ( -21.97457344801873447, 3.670769625195870134, 11.49999999999999645 ) ) ;
#42381 = DIRECTION ( 'NONE',  ( -3.773278334453079618E-23, 0.9999999999976377785, 2.173523156925979975E-06 ) ) ;
#42382 = CARTESIAN_POINT ( 'NONE',  ( -95.55620429048339304, -23.48786465467241058, 11.44779295918254114 ) ) ;
#42383 = EDGE_CURVE ( 'NONE', #64208, #47314, #33766, .T. ) ;
#42384 = CARTESIAN_POINT ( 'NONE',  ( -71.11462141275075055, -25.28903507783076776, 5.642180431236864635 ) ) ;
#42385 = ORIENTED_EDGE ( 'NONE', *, *, #41567, .F. ) ;
#42387 = ORIENTED_EDGE ( 'NONE', *, *, #23354, .T. ) ;
#42386 = CARTESIAN_POINT ( 'NONE',  ( -40.62287095715004881, -24.83602698348161653, 1.605859176311265735 ) ) ;
#42388 = ADVANCED_FACE ( 'NONE', ( #89550 ), #13498, .T. ) ;
#42389 = ORIENTED_EDGE ( 'NONE', *, *, #24050, .T. ) ;
#42390 = CARTESIAN_POINT ( 'NONE',  ( 31.10634905326439181, -4.583458114012134210, -2.800232393899708683 ) ) ;
#42391 = VECTOR ( 'NONE', #62246, 1000.000000000000114 ) ;
#42392 = CARTESIAN_POINT ( 'NONE',  ( -88.62287095715004170, -23.95044443724992078, 10.65354141964649237 ) ) ;
#42393 = PLANE ( 'NONE',  #29098 ) ;
#42394 = CARTESIAN_POINT ( 'NONE',  ( -51.52287095715006870, -24.64965694238407323, 8.947790433994203596 ) ) ;
#42395 = ORIENTED_EDGE ( 'NONE', *, *, #90543, .F. ) ;
#42396 = CARTESIAN_POINT ( 'NONE',  ( -130.5728709571500588, -24.69152398889280420, 9.136518679570812651 ) ) ;
#42397 = CARTESIAN_POINT ( 'NONE',  ( -5.254942042970298210, 21.81482460008805546, -1.500000000000002220 ) ) ;
#42398 = ORIENTED_EDGE ( 'NONE', *, *, #1504, .T. ) ;
#42399 = CARTESIAN_POINT ( 'NONE',  ( -66.62287095715005592, -23.48783264082478439, -1.443836473390067487 ) ) ;
#42400 = LINE ( 'NONE', #73334, #31294 ) ;
#42401 = CARTESIAN_POINT ( 'NONE',  ( 2.610950917001260141, -6.376774720514411854, 19.54489930512155027 ) ) ;
#42402 = DIRECTION ( 'NONE',  ( -0.000000000000000000, 1.000000000000000000, -0.000000000000000000 ) ) ;
#42404 = EDGE_CURVE ( 'NONE', #98936, #24018, #42400, .T. ) ;
#42403 = CARTESIAN_POINT ( 'NONE',  ( -30.59801660219940800, -24.66459861931856423, 1.095224832288508754 ) ) ;
#42405 = VECTOR ( 'NONE', #17930, 1000.000000000000114 ) ;
#42406 = CARTESIAN_POINT ( 'NONE',  ( -5.058734511472819051, -18.94576116945722788, 11.49999999999998934 ) ) ;
#42407 = CARTESIAN_POINT ( 'NONE',  ( -46.56868028461229159, -23.48783264082476663, -1.443836473390096575 ) ) ;
#42409 = ORIENTED_EDGE ( 'NONE', *, *, #93759, .T. ) ;
#42408 = LOCAL_TIME ( 0, 54, 15.00000000000000000, #26673 ) ;
#42410 = CARTESIAN_POINT ( 'NONE',  ( 11.68953838083566588, 18.09531432177502808, 11.49999999999998934 ) ) ;
#42411 = MANIFOLD_SOLID_BREP ( 'CirPattern1', #43583 ) ;
#42412 = CARTESIAN_POINT ( 'NONE',  ( -128.5894279438219883, -24.65952944569304961, 1.056160979905706787 ) ) ;
#42413 = CARTESIAN_POINT ( 'NONE',  ( -80.88693734264360558, -25.30394771627923234, 5.024145871088269821 ) ) ;
#42414 = CARTESIAN_POINT ( 'NONE',  ( -100.5995565470576167, -25.12159859110350979, 2.838444796902710010 ) ) ;
#42415 = EDGE_CURVE ( 'NONE', #16063, #56862, #3827, .T. ) ;
#42416 = PLANE ( 'NONE',  #18040 ) ;
#42417 = CARTESIAN_POINT ( 'NONE',  ( 5.527175565732886042, -22.34193536506064603, -1.500000000000002220 ) ) ;
#42418 = APPROVAL_DATE_TIME ( #94671, #66842 ) ;
#42419 = CARTESIAN_POINT ( 'NONE',  ( -47.52287095715006160, -24.65952944569304606, 1.056160979905693686 ) ) ;
#42420 = CARTESIAN_POINT ( 'NONE',  ( 15.14080536460164694, -3.622774720514426949, -26.62908960815038384 ) ) ;
#42421 = CARTESIAN_POINT ( 'NONE',  ( 19.93115673323400117, -2.579441489355707606, 11.49999999999999645 ) ) ;
#42422 = CARTESIAN_POINT ( 'NONE',  ( -68.58953762381672448, -23.47596703998600276, 11.44779298504227505 ) ) ;
#42423 = CARTESIAN_POINT ( 'NONE',  ( -118.9228709571500531, -23.47593901973090524, -1.443836447538996426 ) ) ;
#42424 = FACE_OUTER_BOUND ( 'NONE', #35867, .T. ) ;
#42425 = DIRECTION ( 'NONE',  ( 0.000000000000000000, 2.173523156925980399E-06, -0.9999999999976378895 ) ) ;
#42426 = CARTESIAN_POINT ( 'NONE',  ( -20.27875734969026311, 7.743225279485574042, 24.00402280011862288 ) ) ;
#42427 = CARTESIAN_POINT ( 'NONE',  ( -2.735935421901279696, -19.66989661884619522, 11.49999999999998934 ) ) ;
#42428 = DIRECTION ( 'NONE',  ( -0.000000000000000000, 0.000000000000000000, -1.000000000000000000 ) ) ;
#42429 = CARTESIAN_POINT ( 'NONE',  ( -18.24397684793207830, 7.494555614300850266, -1.500000000000002220 ) ) ;
#42430 = CARTESIAN_POINT ( 'NONE',  ( -42.60032721050791338, -23.96119346886880663, -0.6495511937831991434 ) ) ;
#42431 = CARTESIAN_POINT ( 'NONE',  ( 6.727764423076923350, -5.876774720514413630, 19.76442307692307665 ) ) ;
#42432 = LINE ( 'NONE', #97192, #10264 ) ;
#42433 = CARTESIAN_POINT ( 'NONE',  ( 19.36870410414886479, 7.000668502413378569, 11.49999999999999645 ) ) ;
#42434 = CARTESIAN_POINT ( 'NONE',  ( -115.6228709571500559, -24.99156045073393173, 7.747789690856161648 ) ) ;
#42435 = CARTESIAN_POINT ( 'NONE',  ( -7.973561950239375307, 21.24132968703115765, 11.49999999999999645 ) ) ;
#42436 = CIRCLE ( 'NONE', #3530, 251.4258649670780699 ) ;
#42437 = ORIENTED_EDGE ( 'NONE', *, *, #2896, .F. ) ;
#42438 = CARTESIAN_POINT ( 'NONE',  ( -69.78016143783460734, -25.12219113079085631, 6.955938379833897400 ) ) ;
#42439 = CARTESIAN_POINT ( 'NONE',  ( -97.55489528667699517, -23.96119346886881374, -0.6495511937832056937 ) ) ;
#42440 = LINE ( 'NONE', #27201, #27335 ) ;
#42441 = PLANE ( 'NONE',  #38273 ) ;
#42442 = B_SPLINE_CURVE_WITH_KNOTS ( 'NONE', 3,
 ( #14446, #92567, #23042, #54033 ),
 .UNSPECIFIED., .F., .F.,
 ( 4, 4 ),
 ( 0.2189169346825021734, 0.2199176817232675885 ),
 .UNSPECIFIED. ) ;
#42443 = EDGE_LOOP ( 'NONE', ( #60574, #90751, #37360, #14995 ) ) ;
#42444 = VERTEX_POINT ( 'NONE', #19527 ) ;
#42445 = CARTESIAN_POINT ( 'NONE',  ( -99.47014701030484218, -25.19118371826951019, 6.667201686812183503 ) ) ;
#42446 = CARTESIAN_POINT ( 'NONE',  ( -22.87863416751641310, 0.2071024363326711970, -1.500000000000002220 ) ) ;
#42447 = CARTESIAN_POINT ( 'NONE',  ( -74.49974610374124495, -24.51314013834315375, 0.6176544820404125113 ) ) ;
#42448 = CARTESIAN_POINT ( 'NONE',  ( 30.53060340732036337, 1.682774720514426114, -8.442346167188908623 ) ) ;
#42449 = CARTESIAN_POINT ( 'NONE',  ( -65.52287095715009002, -24.92579138211020151, 1.929029949965666235 ) ) ;
#42450 = CARTESIAN_POINT ( 'NONE',  ( -14.39138815452349718, -17.32352244779961481, 11.49999999999999645 ) ) ;
#42451 = VERTEX_POINT ( 'NONE', #65245 ) ;
#42452 = DIRECTION ( 'NONE',  ( -1.743630241030147277E-15, -0.000000000000000000, -1.000000000000000000 ) ) ;
#42453 = VECTOR ( 'NONE', #14188, 1000.000000000000000 ) ;
#42454 = CARTESIAN_POINT ( 'NONE',  ( -18.59763704738199408, -11.70098744416181979, -1.500000000000002220 ) ) ;
#42455 = CARTESIAN_POINT ( 'NONE',  ( -111.5891439529568743, -24.34968618360933945, 0.1864209137778883862 ) ) ;
#42456 = FACE_OUTER_BOUND ( 'NONE', #91942, .T. ) ;
#42458 = ORIENTED_EDGE ( 'NONE', *, *, #60230, .F. ) ;
#42457 = ADVANCED_FACE ( 'NONE', ( #96167 ), #50491, .T. ) ;
#42459 = FACE_OUTER_BOUND ( 'NONE', #39468, .T. ) ;
#42460 = DIRECTION ( 'NONE',  ( 1.000000000000000000, 3.773278334444166432E-23, 8.201307841325785021E-29 ) ) ;
#42461 = VERTEX_POINT ( 'NONE', #60613 ) ;
#42462 = DIRECTION ( 'NONE',  ( 0.8246584009594635223, 1.154631945610162960E-14, -0.5656310827093757876 ) ) ;
#42463 = EDGE_CURVE ( 'NONE', #61220, #36345, #21512, .T. ) ;
#42464 = CARTESIAN_POINT ( 'NONE',  ( -17.09319154528168383, -11.34935287704045948, 11.49999999999998934 ) ) ;
#42465 = ORIENTED_EDGE ( 'NONE', *, *, #12483, .T. ) ;
#42466 = ORIENTED_EDGE ( 'NONE', *, *, #99393, .F. ) ;
#42467 = ORIENTED_EDGE ( 'NONE', *, *, #44345, .F. ) ;
#42468 = DIRECTION ( 'NONE',  ( 0.000000000000000000, 0.000000000000000000, 1.000000000000000000 ) ) ;
#42469 = CARTESIAN_POINT ( 'NONE',  ( 18.33865528945960577, 14.04639130150205872, 11.49999999999998934 ) ) ;
#42470 = CARTESIAN_POINT ( 'NONE',  ( -104.5134480897169169, -24.35071581493544102, 9.817618358456019934 ) ) ;
#42471 = CARTESIAN_POINT ( 'NONE',  ( -2.495337616714382367, -20.20711602426958819, -1.500000000000002220 ) ) ;
#42472 = ADVANCED_FACE ( 'NONE', ( #67227 ), #6795, .F. ) ;
#42473 = ORIENTED_EDGE ( 'NONE', *, *, #30626, .F. ) ;
#42474 = CARTESIAN_POINT ( 'NONE',  ( -12.84880425037202656, 0.3587747205143964613, -26.59900746623529244 ) ) ;
#42475 = CARTESIAN_POINT ( 'NONE',  ( -51.69713094254252184, -25.26628317927419687, 3.905176899872079943 ) ) ;
#42476 = EDGE_CURVE ( 'NONE', #70312, #88108, #68211, .T. ) ;
#42478 = CARTESIAN_POINT ( 'NONE',  ( -105.5090439743186721, -24.83618233451451118, 1.606449574219534826 ) ) ;
#42477 = AXIS2_PLACEMENT_3D ( 'NONE', #63777, #72373, #93688 ) ;
#42479 = CARTESIAN_POINT ( 'NONE',  ( -71.31671495077925726, -25.25855297254991783, 7.173521560893385107 ) ) ;
#42480 = EDGE_LOOP ( 'NONE', ( #31366, #725, #42241, #19331, #16748, #73069, #3548, #30485 ) ) ;
#42481 = CARTESIAN_POINT ( 'NONE',  ( -29.05456498926589504, -25.21531894358851389, 3.361079100850875356 ) ) ;
#42482 = CARTESIAN_POINT ( 'NONE',  ( -86.52287095715006160, -23.48786465467241058, 11.44779295918254292 ) ) ;
#42483 = EDGE_CURVE ( 'NONE', #99053, #15989, #70195, .T. ) ;
#42484 = LOCAL_TIME ( 0, 54, 15.00000000000000000, #68725 ) ;
#42485 = ORIENTED_EDGE ( 'NONE', *, *, #90031, .F. ) ;
#42486 = ADVANCED_FACE ( 'NONE', ( #97652 ), #96208, .T. ) ;
#42487 = CARTESIAN_POINT ( 'NONE',  ( -0.3852054317258338245, -20.75737367715079174, -1.500000000000002220 ) ) ;
#42488 = ORIENTED_EDGE ( 'NONE', *, *, #51871, .T. ) ;
#42490 = ORIENTED_EDGE ( 'NONE', *, *, #28408, .T. ) ;
#42489 = CARTESIAN_POINT ( 'NONE',  ( -61.62287095715004881, -24.65952944569304606, 1.056160979905695907 ) ) ;
#42491 = LINE ( 'NONE', #10514, #58458 ) ;
#42492 = CARTESIAN_POINT ( 'NONE',  ( -51.04357394935764347, -25.30543060587211812, 4.940877950953177056 ) ) ;
#42493 = ORIENTED_EDGE ( 'NONE', *, *, #14470, .F. ) ;
#42494 = ORIENTED_EDGE ( 'NONE', *, *, #100264, .F. ) ;
#42495 = CARTESIAN_POINT ( 'NONE',  ( -79.62287095715005592, -23.48783264082478794, -1.443836473390065489 ) ) ;
#42496 = CARTESIAN_POINT ( 'NONE',  ( -116.6228709571500559, -23.73934037231757799, 11.05740245334328264 ) ) ;
#42497 = CARTESIAN_POINT ( 'NONE',  ( -70.35895856474229504, -25.24515042133736387, 5.313173755051357361 ) ) ;
#42499 = ORIENTED_EDGE ( 'NONE', *, *, #27927, .T. ) ;
#42498 = CARTESIAN_POINT ( 'NONE',  ( 20.41560922187292348, 8.460057656491983380, 11.49999999999999645 ) ) ;
#42500 = CARTESIAN_POINT ( 'NONE',  ( -45.62287095715005592, -23.48786465467240703, 11.44779295918255002 ) ) ;
#42501 = CARTESIAN_POINT ( 'NONE',  ( 18.14931799402153345, 13.46472642042223633, 11.49999999999998934 ) ) ;
#42503 = ORIENTED_EDGE ( 'NONE', *, *, #18065, .F. ) ;
#42502 = CARTESIAN_POINT ( 'NONE',  ( -46.52287095715004028, -24.35013146730202394, 9.818937971375106599 ) ) ;
#42504 = VERTEX_POINT ( 'NONE', #22007 ) ;
#42505 = FACE_OUTER_BOUND ( 'NONE', #52679, .T. ) ;
#42506 = AXIS2_PLACEMENT_3D ( 'NONE', #10035, #2942, #96772 ) ;
#42507 = CARTESIAN_POINT ( 'NONE',  ( -7.347880794884120722E-16, -4.056774720514426669, -6.000000000000000888 ) ) ;
#42508 = ORIENTED_EDGE ( 'NONE', *, *, #68361, .T. ) ;
#42509 = CARTESIAN_POINT ( 'NONE',  ( -21.05374637409849825, 2.266213160971460194, -1.500000000000002220 ) ) ;
#42510 = CARTESIAN_POINT ( 'NONE',  ( -125.5228709571500616, -29.50250786944525672, 11.44777988621622633 ) ) ;
#42511 = CARTESIAN_POINT ( 'NONE',  ( -40.66978929498593942, -25.29385509343200766, 5.536656401469072009 ) ) ;
#42512 = CARTESIAN_POINT ( 'NONE',  ( 15.07672925556244969, 16.42598562245719407, -1.500000000000002220 ) ) ;
#42513 = CARTESIAN_POINT ( 'NONE',  ( -50.04527796557857755, -25.03220900868303644, 7.536031501934568944 ) ) ;
#42514 = EDGE_LOOP ( 'NONE', ( #46654, #11482, #98917, #59398 ) ) ;
#42515 = CARTESIAN_POINT ( 'NONE',  ( 11.54156857142115911, 5.965225279485592225, -28.05134709678029381 ) ) ;
#42516 = DIRECTION ( 'NONE',  ( 1.000000000000000000, 0.000000000000000000, 0.000000000000000000 ) ) ;
#42517 = CARTESIAN_POINT ( 'NONE',  ( -36.50466263922482568, -23.96169478059712432, 10.65365249895718591 ) ) ;
#42518 = CARTESIAN_POINT ( 'NONE',  ( -83.58953762381672448, -24.64965694238407323, 8.947790433994653014 ) ) ;
#42519 = B_SPLINE_CURVE_WITH_KNOTS ( 'NONE', 3,
 ( #79684, #73090, #4576, #66497 ),
 .UNSPECIFIED., .F., .F.,
 ( 4, 4 ),
 ( 0.000000000000000000, 9.999999999998897304E-05 ),
 .UNSPECIFIED. ) ;
#42520 = CARTESIAN_POINT ( 'NONE',  ( 16.17817332762582794, -10.88531698672339942, -1.500000000000002220 ) ) ;
#42521 = VECTOR ( 'NONE', #48392, 1000.000000000000114 ) ;
#42522 = CARTESIAN_POINT ( 'NONE',  ( 17.68986881342592454, -12.14045624799103962, -1.500000000000002220 ) ) ;
#42523 = CARTESIAN_POINT ( 'NONE',  ( -1.064504969004270052, -5.876774720514408301, 19.35667676486395905 ) ) ;
#42524 = CIRCLE ( 'NONE', #99199, 4.080000000000000071 ) ;
#42525 = CARTESIAN_POINT ( 'NONE',  ( -107.5228709571500758, -23.48786465467241769, 11.44779295918253936 ) ) ;
#42526 = DIRECTION ( 'NONE',  ( 0.000000000000000000, -2.173523156925979552E-06, 0.9999999999976378895 ) ) ;
#42527 = ADVANCED_FACE ( 'NONE', ( #82918 ), #92941, .T. ) ;
#42528 = CARTESIAN_POINT ( 'NONE',  ( -19.63924127562733446, 11.44998032699685631, -1.500000000000002220 ) ) ;
#42529 = EDGE_CURVE ( 'NONE', #79651, #26860, #71051, .T. ) ;
#42530 = CARTESIAN_POINT ( 'NONE',  ( 139.5443831022365373, -6.474179415928272618, 23.70558727230211460 ) ) ;
#42531 = PLANE ( 'NONE',  #69325 ) ;
#42532 = LINE ( 'NONE', #73964, #13539 ) ;
#42533 = CARTESIAN_POINT ( 'NONE',  ( -15.73602684802347440, -12.20685706852216867, 11.49999999999999645 ) ) ;
#42534 = CARTESIAN_POINT ( 'NONE',  ( -101.6228709571500559, -24.51387760970723662, 9.387446482453405849 ) ) ;
#42535 = CARTESIAN_POINT ( 'NONE',  ( -128.5228709571501042, -23.72773821059536914, 11.05748984161097326 ) ) ;
#42536 = CARTESIAN_POINT ( 'NONE',  ( -128.5228709571501042, -24.66019654487200441, 8.947790411086108620 ) ) ;
#42537 = ORIENTED_EDGE ( 'NONE', *, *, #81323, .F. ) ;
#42538 = DIRECTION ( 'NONE',  ( -0.000000000000000000, 2.173523156925979552E-06, -0.9999999999976378895 ) ) ;
#42539 = CARTESIAN_POINT ( 'NONE',  ( -33.01375014246017514, -24.87479601683088148, 8.247789944647561100 ) ) ;
#42540 = CARTESIAN_POINT ( 'NONE',  ( 21.38347125639554136, -3.707035686939989638, -1.500000000000002220 ) ) ;
#42541 = CARTESIAN_POINT ( 'NONE',  ( -50.79429371764780399, -25.04955745062598282, 7.532901908008377667 ) ) ;
#42542 = CARTESIAN_POINT ( 'NONE',  ( 8.254404603115069960, -17.72612730319335839, -1.500000000000002220 ) ) ;
#42543 = CARTESIAN_POINT ( 'NONE',  ( -100.6228709571500559, -25.00182538069145721, 7.747789668545099317 ) ) ;
#42544 = VECTOR ( 'NONE', #94151, 1000.000000000000114 ) ;
#42545 = COORDINATED_UNIVERSAL_TIME_OFFSET ( 0, 0, .AHEAD. ) ;
#42546 = CARTESIAN_POINT ( 'NONE',  ( 31.82032313667048484, -0.3587747205144265483, 9.148483289431938559 ) ) ;
#42547 = CARTESIAN_POINT ( 'NONE',  ( -60.62287095715005592, -24.92604778743016780, 8.074972756849359001 ) ) ;
#42548 = CARTESIAN_POINT ( 'NONE',  ( -19.82921842031888104, 5.099586017421429140, 11.49999999999999645 ) ) ;
#42549 = CARTESIAN_POINT ( 'NONE',  ( 16.09831413233135677, 3.622774720514429614, -27.82446136760824018 ) ) ;
#42551 = EDGE_CURVE ( 'NONE', #92914, #99448, #766, .T. ) ;
#42550 = APPROVAL ( #68363, 'UNKNOWN' ) ;
#42552 = CARTESIAN_POINT ( 'NONE',  ( -114.6228709571500701, -23.47596703998600631, 11.44779298504227860 ) ) ;
#42553 = VECTOR ( 'NONE', #90297, 1000.000000000000000 ) ;
#42554 = EDGE_LOOP ( 'NONE', ( #90036, #89385, #28604, #31346, #753, #94713 ) ) ;
#42555 = LINE ( 'NONE', #12578, #55646 ) ;
#42556 = LINE ( 'NONE', #89215, #36391 ) ;
#42557 = DIRECTION ( 'NONE',  ( 0.000000000000000000, -0.9999999999976377785, -2.173523156925979128E-06 ) ) ;
#42558 = AXIS2_PLACEMENT_3D ( 'NONE', #49613, #47605, #80041 ) ;
#42559 = CARTESIAN_POINT ( 'NONE',  ( -109.5865577389930650, -24.65952944569305316, 1.056160979905708786 ) ) ;
#42560 = ORIENTED_EDGE ( 'NONE', *, *, #76468, .T. ) ;
#42561 = DIRECTION ( 'NONE',  ( -3.773278334444166432E-23, 1.000000000000000000, 0.000000000000000000 ) ) ;
#42562 = CARTESIAN_POINT ( 'NONE',  ( 18.48385363477634513, -13.70420857335572506, 11.49999999999999645 ) ) ;
#42563 = CARTESIAN_POINT ( 'NONE',  ( -9.471985145535571249, 20.67137392225973258, 11.49999999999998934 ) ) ;
#42564 = CARTESIAN_POINT ( 'NONE',  ( -110.5141131277583639, -24.52399227489124556, 9.353111116836533512 ) ) ;
#42565 = B_SPLINE_SURFACE_WITH_KNOTS ( 'NONE', 3, 3, ( 
 ( #19503, #95638, #71809, #33231 ),
 ( #79901, #95136, #19002, #79402 ),
 ( #26123, #49479, #49982, #25110 ),
 ( #48971, #80908, #57094, #27126 ),
 ( #41352, #80409, #11399, #72306 ),
 ( #58092, #10902, #11893, #94630 ),
 ( #41866, #89027, #4291, #2802 ),
 ( #42373, #42863, #3313, #73306 ),
 ( #73792, #56086, #74295, #89519 ),
 ( #60585, #35241, #28125, #28619 ) ),
 .UNSPECIFIED., .F., .F., .F.,
 ( 4, 3, 3, 4 ),
 ( 4, 4 ),
 ( 0.7022005934544809369, 0.7765311282028795059, 0.8508616629512781859, 0.9995227324480755460 ),
 ( 0.09950600549362356717, 0.1005780349481100455 ),
 .UNSPECIFIED. ) ;
#42566 = CARTESIAN_POINT ( 'NONE',  ( -122.5228709571500616, -24.64898659630368272, 1.056161002820833028 ) ) ;
#42567 = CARTESIAN_POINT ( 'NONE',  ( -50.52287095715006160, -25.00158670708909270, 2.256160236439166411 ) ) ;
#42568 = CARTESIAN_POINT ( 'NONE',  ( -69.34303308397305443, -25.25559839591755207, 6.209207386190695566 ) ) ;
#42569 = CARTESIAN_POINT ( 'NONE',  ( -15.13543854793762300, 15.80457324685279374, -1.500000000000002220 ) ) ;
#42570 = FACE_BOUND ( 'NONE', #67191, .T. ) ;
#42571 = CIRCLE ( 'NONE', #32858, 21.89999999999999858 ) ;
#42572 = CARTESIAN_POINT ( 'NONE',  ( -120.5228709571500900, -25.00182538069145366, 7.747789668545101982 ) ) ;
#42573 = CARTESIAN_POINT ( 'NONE',  ( -24.97666371003640506, -0.3587747205143964613, -15.72894043976419454 ) ) ;
#42574 = CARTESIAN_POINT ( 'NONE',  ( 6.573941812937369455, -0.2639660507643297183, -9.295380466955404257E-16 ) ) ;
#42575 = VERTEX_POINT ( 'NONE', #87302 ) ;
#42576 = PRODUCT ( 'oval head_am_B18.6.7M - M2.5 x 0.45 x 13 Type I Cross Recessed OHMS --13C', 'oval head_am_B18.6.7M - M2.5 x 0.45 x 13 Type I Cross Recessed OHMS --13C', '', ( #13540 ) ) ;
#42577 = CARTESIAN_POINT ( 'NONE',  ( -20.22731604866883970, -2.807383831903240257, -1.500000000000002220 ) ) ;
#42578 = VERTEX_POINT ( 'NONE', #24402 ) ;
#42579 = ORIENTED_EDGE ( 'NONE', *, *, #25403, .F. ) ;
#42580 = VERTEX_POINT ( 'NONE', #78175 ) ;
#42581 = EDGE_LOOP ( 'NONE', ( #43857, #100193, #83830, #78512, #73667, #74725, #68160, #53818, #91202, #99204 ) ) ;
#42582 = CARTESIAN_POINT ( 'NONE',  ( 0.2859537766682072601, -23.01552763051285666, 11.49999999999998934 ) ) ;
#42583 = DIRECTION ( 'NONE',  ( 0.000000000000000000, 0.9999999999976377785, 2.173523156925979128E-06 ) ) ;
#42584 = CARTESIAN_POINT ( 'NONE',  ( -16.67386609800740516, 11.36076560755915033, -1.500000000000002220 ) ) ;
#42585 = ORIENTED_EDGE ( 'NONE', *, *, #68687, .T. ) ;
#42586 = DIRECTION ( 'NONE',  ( 1.000000000000000000, 3.773278334444167608E-23, 8.201307833595939069E-29 ) ) ;
#42587 = CARTESIAN_POINT ( 'NONE',  ( -77.62287095715009855, -23.47596703998600631, 11.44779298504227683 ) ) ;
#42588 = CARTESIAN_POINT ( 'NONE',  ( -95.50150878202170190, -25.00158670708911046, 2.256160236439221034 ) ) ;
#42589 = CARTESIAN_POINT ( 'NONE',  ( -108.6228709571500559, -29.50248528299804818, 1.056150453629043584 ) ) ;
#42591 = EDGE_LOOP ( 'NONE', ( #26584, #46559, #43814, #9288 ) ) ;
#42590 = CARTESIAN_POINT ( 'NONE',  ( 15.12546962493697933, 15.13007008128210096, 11.49999999999999645 ) ) ;
#42592 = CARTESIAN_POINT ( 'NONE',  ( -55.52287095715006870, -24.91544648472619983, 1.928969306349232360 ) ) ;
#42593 = VECTOR ( 'NONE', #93423, 1000.000000000000114 ) ;
#42594 = EDGE_CURVE ( 'NONE', #17644, #29613, #97635, .T. ) ;
#42595 = ORIENTED_EDGE ( 'NONE', *, *, #79921, .T. ) ;
#42596 = CARTESIAN_POINT ( 'NONE',  ( 0.6114060112162268412, -22.25658958135186793, 11.49999999999998934 ) ) ;
#42597 = EDGE_CURVE ( 'NONE', #77757, #28152, #62606, .T. ) ;
#42598 = CARTESIAN_POINT ( 'NONE',  ( -14.21563987850626276, 15.01860006206015008, -1.500000000000002220 ) ) ;
#42599 = EDGE_LOOP ( 'NONE', ( #26954, #64225, #67569, #67471 ) ) ;
#42600 = CARTESIAN_POINT ( 'NONE',  ( -71.73006576507869170, -25.03707830618030172, 7.590867772707287742 ) ) ;
#42601 = EDGE_LOOP ( 'NONE', ( #40954, #63428, #25304, #33000 ) ) ;
#42602 = CARTESIAN_POINT ( 'NONE',  ( -56.52287095715006160, -24.33832256527049154, 0.1851278514138608444 ) ) ;
#42603 = EDGE_LOOP ( 'NONE', ( #50611, #72913, #50947, #9011 ) ) ;
#42604 = CARTESIAN_POINT ( 'NONE',  ( 11.41483471809167405, -3.316774720514427344, -27.05170832580397189 ) ) ;
#42605 = CARTESIAN_POINT ( 'NONE',  ( -11.48448384864204996, -17.54081393385053644, -1.500000000000002220 ) ) ;
#42606 = EDGE_CURVE ( 'NONE', #35113, #76129, #16789, .T. ) ;
#42607 = CARTESIAN_POINT ( 'NONE',  ( 21.74639208212181529, -2.611101805624240768, 11.49999999999999645 ) ) ;
#42608 = CARTESIAN_POINT ( 'NONE',  ( -73.54545617769827004, -24.35071581493543036, 9.817618358456027039 ) ) ;
#42609 = CARTESIAN_POINT ( 'NONE',  ( 5.070899574700155732, -21.93562493352797915, 11.49999999999998934 ) ) ;
#42610 = CARTESIAN_POINT ( 'NONE',  ( -8.544475976622297964, 19.10969517993760292, 11.49999999999998934 ) ) ;
#42611 = CARTESIAN_POINT ( 'NONE',  ( -110.5228709571500616, -24.99132157543167310, 2.256160258750667502 ) ) ;
#42612 = CARTESIAN_POINT ( 'NONE',  ( 5.872047395031165351, -5.876774720514415407, 20.29192741308114734 ) ) ;
#42613 = CARTESIAN_POINT ( 'NONE',  ( -29.62287095715005236, -23.66089804901488947, 11.05752276264044021 ) ) ;
#42614 = FACE_OUTER_BOUND ( 'NONE', #35238, .T. ) ;
#42615 = ORIENTED_EDGE ( 'NONE', *, *, #9351, .T. ) ;
#42616 = CARTESIAN_POINT ( 'NONE',  ( -84.55620429048339304, -23.48786465467241413, 11.44779295918254469 ) ) ;
#42617 = VERTEX_POINT ( 'NONE', #70582 ) ;
#42618 = VERTEX_POINT ( 'NONE', #18300 ) ;
#42619 = DIRECTION ( 'NONE',  ( -3.773278334453079618E-23, 0.9999999999976377785, 2.173523156925979975E-06 ) ) ;
#42620 = ORIENTED_EDGE ( 'NONE', *, *, #74125, .F. ) ;
#42621 = CARTESIAN_POINT ( 'NONE',  ( 21.36505145794347982, 1.902718533054148509, -1.500000000000002220 ) ) ;
#42622 = AXIS2_PLACEMENT_3D ( 'NONE', #72989, #3478, #34416 ) ;
#42623 = CARTESIAN_POINT ( 'NONE',  ( 282.9764569301858046, -0.3587747205144265483, 20.79159422840526616 ) ) ;
#42624 = CARTESIAN_POINT ( 'NONE',  ( 15.50021099394596646, 14.30638080151107694, 11.49999999999998934 ) ) ;
#42625 = CARTESIAN_POINT ( 'NONE',  ( -99.53456258256274225, -25.26500153315007324, 3.892973016135182096 ) ) ;
#42626 = CARTESIAN_POINT ( 'NONE',  ( 3.714529970114099022, -6.376774720514426065, 21.83853177191107520 ) ) ;
#42627 = CARTESIAN_POINT ( 'NONE',  ( -50.57159555137985052, -23.48786465467240347, 11.44779295918255002 ) ) ;
#42628 = CARTESIAN_POINT ( 'NONE',  ( -101.6314100629513035, -23.96119346886880663, -0.6495511937832048055 ) ) ;
#42629 = CARTESIAN_POINT ( 'NONE',  ( -129.5560488321862351, -23.73791477778912551, 11.05961554403170055 ) ) ;
#42630 = CARTESIAN_POINT ( 'NONE',  ( 11.82310115920509830, 18.66461490495635545, -1.500000000000002220 ) ) ;
#42631 = AXIS2_PLACEMENT_3D ( 'NONE', #96638, #22715, #46584 ) ;
#42632 = ORIENTED_EDGE ( 'NONE', *, *, #59636, .F. ) ;
#42633 = CARTESIAN_POINT ( 'NONE',  ( -81.50253896702017187, -24.51419770103159834, 9.386484678747182286 ) ) ;
#42634 = B_SPLINE_CURVE_WITH_KNOTS ( 'NONE', 3,
 ( #36234, #29603, #82890, #53463 ),
 .UNSPECIFIED., .F., .F.,
 ( 4, 4 ),
 ( 0.07055037829823759821, 0.07955680957035315970 ),
 .UNSPECIFIED. ) ;
#42635 = CARTESIAN_POINT ( 'NONE',  ( -113.6228709571500559, -29.50247984919015209, -1.443849546365048253 ) ) ;
#42636 = CARTESIAN_POINT ( 'NONE',  ( -40.53889064818358889, -25.27956071218200762, 5.542732955578356879 ) ) ;
#42637 = B_SPLINE_CURVE_WITH_KNOTS ( 'NONE', 3,
 ( #651, #7764, #92990, #22469, #92495, #93491 ),
 .UNSPECIFIED., .F., .F.,
 ( 4, 2, 4 ),
 ( 0.000000000000000000, 0.001380901958385388545, 0.002761803916770777089 ),
 .UNSPECIFIED. ) ;
#42638 = B_SPLINE_CURVE_WITH_KNOTS ( 'NONE', 3,
 ( #68949, #30381, #99873, #29884 ),
 .UNSPECIFIED., .F., .F.,
 ( 4, 4 ),
 ( 0.000000000000000000, 9.999999999998897304E-05 ),
 .UNSPECIFIED. ) ;
#42639 = ADVANCED_FACE ( 'NONE', ( #65003 ), #45966, .T. ) ;
#42640 = CARTESIAN_POINT ( 'NONE',  ( -25.50502449915233072, -24.92980806509333647, 6.075536601959949934 ) ) ;
#42641 = B_SPLINE_CURVE_WITH_KNOTS ( 'NONE', 3,
 ( #98897, #53747, #77055, #38508 ),
 .UNSPECIFIED., .F., .F.,
 ( 4, 4 ),
 ( 0.000000000000000000, 0.003057692307692316813 ),
 .UNSPECIFIED. ) ;
#42642 = DIRECTION ( 'NONE',  ( 0.5656310827093757876, 2.995395837334948684E-15, -0.8246584009594636333 ) ) ;
#42643 = CARTESIAN_POINT ( 'NONE',  ( -11.21157863559261791, -18.18922556752850994, -1.500000000000002220 ) ) ;
#42644 = CARTESIAN_POINT ( 'NONE',  ( -69.98187464599547525, -25.05189924121757272, 7.521888907215067199 ) ) ;
#42645 = CARTESIAN_POINT ( 'NONE',  ( -79.62287095715005592, -29.50250786944525672, 11.44777988621623521 ) ) ;
#42646 = EDGE_CURVE ( 'NONE', #48546, #64856, #51642, .T. ) ;
#42647 = PLANE ( 'NONE',  #11390 ) ;
#42648 = CARTESIAN_POINT ( 'NONE',  ( 14.76093561896379214, -5.965225279485572685, -26.55548769130089681 ) ) ;
#42649 = CARTESIAN_POINT ( 'NONE',  ( -22.56969522194696509, -0.6267768857631424995, -1.500000000000002220 ) ) ;
#42650 = B_SPLINE_SURFACE_WITH_KNOTS ( 'NONE', 3, 3, ( 
 ( #30693, #32187, #85472, #45935 ),
 ( #76845, #61666, #38801, #15957 ),
 ( #92582, #61170, #37812, #84976 ),
 ( #15461, #78354, #69763, #243 ),
 ( #62160, #23567, #86478, #8354 ),
 ( #743, #24074, #94087, #55043 ),
 ( #85981, #8855, #1752, #17973 ) ),
 .UNSPECIFIED., .F., .F., .F.,
 ( 4, 3, 4 ),
 ( 4, 4 ),
 ( 0.0004766839783823611197, 0.1029713700210900251, 0.2054660560637976974 ),
 ( 0.05950913535538977089, 0.06054931731713387305 ),
 .UNSPECIFIED. ) ;
#42651 = CARTESIAN_POINT ( 'NONE',  ( -70.62287095715005592, -29.50250786944525672, 11.44777988621623699 ) ) ;
#42652 = EDGE_LOOP ( 'NONE', ( #30707, #78035, #46721, #78429 ) ) ;
#42653 = DIRECTION ( 'NONE',  ( 0.000000000000000000, 0.9999999999976377785, 2.173523156925979975E-06 ) ) ;
#42654 = DIRECTION ( 'NONE',  ( -3.773278334453079618E-23, 0.9999999999976377785, 2.173523156925979975E-06 ) ) ;
#42655 = CARTESIAN_POINT ( 'NONE',  ( 12.99534586470982234, -14.87506298573330632, 11.49999999999999645 ) ) ;
#42656 = CARTESIAN_POINT ( 'NONE',  ( -126.6228709571500559, -23.48786465467242124, 11.44779295918253403 ) ) ;
#42657 = CARTESIAN_POINT ( 'NONE',  ( -67.63597519206453512, -24.15543982623906771, -0.2315651400026651485 ) ) ;
#42658 = ORIENTED_EDGE ( 'NONE', *, *, #42153, .F. ) ;
#42659 = CARTESIAN_POINT ( 'NONE',  ( -13.57581083383196940, -6.376774720514426953, 20.21213203435597094 ) ) ;
#42660 = CARTESIAN_POINT ( 'NONE',  ( -29.61081252053125112, -24.60094231151948208, 3.196431696360289010 ) ) ;
#42661 = AXIS2_PLACEMENT_3D ( 'NONE', #7646, #61446, #67561 ) ;
#42662 = CARTESIAN_POINT ( 'NONE',  ( -29.49875734969026198, 5.965225279485572685, 7.870022800118625206 ) ) ;
#42663 = CARTESIAN_POINT ( 'NONE',  ( -11.89702471719568244, -18.04982639819725776, 11.49999999999998934 ) ) ;
#42664 = CARTESIAN_POINT ( 'NONE',  ( -76.52287095715007581, -24.64898659630528854, 1.056161002820826145 ) ) ;
#42665 = CARTESIAN_POINT ( 'NONE',  ( -17.66094656686658482, 7.961706694365092041, -1.500000000000002220 ) ) ;
#42666 = DIRECTION ( 'NONE',  ( -0.1875268396392987258, -0.000000000000000000, -0.9822594791677485837 ) ) ;
#42667 = LINE ( 'NONE', #55498, #58833 ) ;
#42668 = CARTESIAN_POINT ( 'NONE',  ( 1.028332004353105233, 19.75660188889424518, 11.49999999999998934 ) ) ;
#42669 = ORIENTED_EDGE ( 'NONE', *, *, #63895, .F. ) ;
#42670 = AXIS2_PLACEMENT_3D ( 'NONE', #20677, #56901, #87835 ) ;
#42671 = CARTESIAN_POINT ( 'NONE',  ( 19.74221769882431587, -4.499994434135383692, 11.49999999999999645 ) ) ;
#42672 = DIRECTION ( 'NONE',  ( 0.000000000000000000, 0.000000000000000000, -1.000000000000000000 ) ) ;
#42673 = APPROVAL ( #33780, 'UNSPECIFIED' ) ;
#42674 = ORIENTED_EDGE ( 'NONE', *, *, #94194, .T. ) ;
#42675 = CARTESIAN_POINT ( 'NONE',  ( -100.0625863431822324, -25.30020101379185959, 4.636546911730082599 ) ) ;
#42676 = CYLINDRICAL_SURFACE ( 'NONE', #91418, 3.349999999999998757 ) ;
#42677 = CARTESIAN_POINT ( 'NONE',  ( 11.03981094302168842, -0.3587747205144256601, -28.06140118199223465 ) ) ;
#42678 = DIRECTION ( 'NONE',  ( 0.000000000000000000, 2.173523156925980399E-06, -0.9999999999976378895 ) ) ;
#42679 = FACE_OUTER_BOUND ( 'NONE', #52689, .T. ) ;
#42680 = CARTESIAN_POINT ( 'NONE',  ( 11.63622169266987783, 16.31392799894670631, -1.500000000000002220 ) ) ;
#42681 = CARTESIAN_POINT ( 'NONE',  ( -16.22218391600152643, 6.376774720514426953, -54.85883559227303863 ) ) ;
#42682 = ORIENTED_EDGE ( 'NONE', *, *, #47369, .F. ) ;
#42683 = ADVANCED_FACE ( 'NONE', ( #67473 ), #6214, .T. ) ;
#42684 = VECTOR ( 'NONE', #39731, 1000.000000000000114 ) ;
#42685 = CARTESIAN_POINT ( 'NONE',  ( -50.27385278553439463, -25.26258884680880712, 4.732894951404434281 ) ) ;
#42686 = LINE ( 'NONE', #74605, #8857 ) ;
#42687 = CARTESIAN_POINT ( 'NONE',  ( -80.36267167646580845, -25.30553951917087119, 4.968573168359604608 ) ) ;
#42688 = CYLINDRICAL_SURFACE ( 'NONE', #56259, 0.3000000000000016542 ) ;
#42689 = FACE_OUTER_BOUND ( 'NONE', #44205, .T. ) ;
#42690 = CARTESIAN_POINT ( 'NONE',  ( -89.40841769935768468, -25.18330262420952437, 6.757888864229147252 ) ) ;
#42691 = AXIS2_PLACEMENT_3D ( 'NONE', #59139, #82947, #75337 ) ;
#42692 = CARTESIAN_POINT ( 'NONE',  ( -116.6228709571500559, -24.65952944569305316, 1.056160979905706121 ) ) ;
#42693 = VERTEX_POINT ( 'NONE', #74574 ) ;
#42694 = CARTESIAN_POINT ( 'NONE',  ( -15.63206872509828571, 12.99414084278249071, -1.500000000000002220 ) ) ;
#42695 = VECTOR ( 'NONE', #100110, 1000.000000000000000 ) ;
#42696 = ORIENTED_EDGE ( 'NONE', *, *, #18083, .T. ) ;
#42697 = EDGE_CURVE ( 'NONE', #67032, #54301, #32208, .T. ) ;
#42698 = CARTESIAN_POINT ( 'NONE',  ( -22.60589916338503613, 3.847557683979087706, -1.500000000000002220 ) ) ;
#42699 = CARTESIAN_POINT ( 'NONE',  ( -32.65885280296615178, -23.73766607897670866, -1.055555164236442023 ) ) ;
#42700 = ORIENTED_EDGE ( 'NONE', *, *, #57122, .F. ) ;
#42701 = LINE ( 'NONE', #44185, #18517 ) ;
#42702 = CARTESIAN_POINT ( 'NONE',  ( 15.30286968208600307, 3.576092370626933636, -27.16555646467131524 ) ) ;
#42703 = LINE ( 'NONE', #4129, #5896 ) ;
#42704 = CARTESIAN_POINT ( 'NONE',  ( 7.804836024166685426, 19.70032748343534834, 11.49999999999999645 ) ) ;
#42705 = EDGE_CURVE ( 'NONE', #82541, #21005, #35531, .T. ) ;
#42706 = CARTESIAN_POINT ( 'NONE',  ( -22.11188964843745453, -1.696007508606716341, -1.500000000000002220 ) ) ;
#42707 = EDGE_CURVE ( 'NONE', #14471, #29214, #75062, .T. ) ;
#42708 = CARTESIAN_POINT ( 'NONE',  ( 6.154377932377651739, 19.64630176443789367, 11.49999999999998934 ) ) ;
#42709 = EDGE_LOOP ( 'NONE', ( #39024, #71404, #68329, #64072, #9859, #13548, #44840, #1668, #95886, #44561, #20098, #69134, #79153 ) ) ;
#42710 = CARTESIAN_POINT ( 'NONE',  ( -41.58699204436209129, -24.34968618360933590, 0.1864209137778856940 ) ) ;
#42711 = ORIENTED_EDGE ( 'NONE', *, *, #15306, .T. ) ;
#42712 = LINE ( 'NONE', #49324, #59298 ) ;
#42713 = LINE ( 'NONE', #97478, #95623 ) ;
#42714 = EDGE_LOOP ( 'NONE', ( #22692, #16214, #90855, #47347 ) ) ;
#42715 = ORIENTED_EDGE ( 'NONE', *, *, #11905, .T. ) ;
#42716 = APPLICATION_CONTEXT ( 'configuration controlled 3d designs of mechanical parts and assemblies' ) ;
#42717 = ORIENTED_EDGE ( 'NONE', *, *, #66892, .F. ) ;
#42718 = CARTESIAN_POINT ( 'NONE',  ( -59.62287095715004881, -29.50250243563736774, 8.947779886222145151 ) ) ;
#42719 = CARTESIAN_POINT ( 'NONE',  ( -28.55247368671063768, -23.80130948982615280, 10.65365253163527193 ) ) ;
#42720 = CARTESIAN_POINT ( 'NONE',  ( 14.66599494348457888, -4.455096676454772364, -28.01208847159967164 ) ) ;
#42721 = CARTESIAN_POINT ( 'NONE',  ( 8.056674255711671506, 19.11000797562349618, -1.500000000000002220 ) ) ;
#42722 = ADVANCED_FACE ( 'NONE', ( #13164 ), #89310, .F. ) ;
#42723 = CARTESIAN_POINT ( 'NONE',  ( -21.53672441135761773, -2.854535511010750870, 11.49999999999999645 ) ) ;
#42724 = ORIENTED_EDGE ( 'NONE', *, *, #38780, .F. ) ;
#42725 = AXIS2_PLACEMENT_3D ( 'NONE', #74671, #12766, #42262 ) ;
#42726 = DIRECTION ( 'NONE',  ( 0.000000000000000000, 1.000000000000000000, 0.000000000000000000 ) ) ;
#42727 = CARTESIAN_POINT ( 'NONE',  ( -115.5510445847871779, -24.83618233451450408, 1.606449574219536824 ) ) ;
#42728 = CARTESIAN_POINT ( 'NONE',  ( -21.57557905285345612, -6.117077608415351087, -1.500000000000002220 ) ) ;
#42729 = DIRECTION ( 'NONE',  ( 0.000000000000000000, 0.000000000000000000, 1.000000000000000000 ) ) ;
#42730 = CARTESIAN_POINT ( 'NONE',  ( -9.150000000000000355, -6.376774720514426953, -15.69999999999999929 ) ) ;
#42731 = VERTEX_POINT ( 'NONE', #5562 ) ;
#42732 = CARTESIAN_POINT ( 'NONE',  ( -25.92875734969025814, 3.316774720514426456, -0.08597719988137648983 ) ) ;
#42733 = CARTESIAN_POINT ( 'NONE',  ( -89.54303308397305727, -25.05712135967894838, 7.447789548357303779 ) ) ;
#42734 = CIRCLE ( 'NONE', #94563, 1.149999999999998135 ) ;
#42735 = VERTEX_POINT ( 'NONE', #50753 ) ;
#42736 = EDGE_LOOP ( 'NONE', ( #83687, #6424, #86870, #14968 ) ) ;
#42737 = DIRECTION ( 'NONE',  ( -3.773278334453079030E-23, 0.9999999999976377785, 2.173523156925979128E-06 ) ) ;
#42738 = EDGE_LOOP ( 'NONE', ( #39060, #19114, #32977, #38481 ) ) ;
#42739 = CARTESIAN_POINT ( 'NONE',  ( -16.85803360905838488, 12.98640638483674259, -1.500000000000002220 ) ) ;
#42740 = ORIENTED_EDGE ( 'NONE', *, *, #4649, .T. ) ;
#42741 = CARTESIAN_POINT ( 'NONE',  ( -68.62287095715008434, -24.34917612406838217, 0.1852690917426622341 ) ) ;
#42742 = CARTESIAN_POINT ( 'NONE',  ( 16.27406392464308027, 14.57352745747340172, 11.49999999999998934 ) ) ;
#42743 = DIRECTION ( 'NONE',  ( 0.000000000000000000, -0.9999999999976377785, -2.173523156925979128E-06 ) ) ;
#42744 = CARTESIAN_POINT ( 'NONE',  ( -5.639450322166912777, -21.95568564230989850, 11.49999999999998934 ) ) ;
#42745 = CARTESIAN_POINT ( 'NONE',  ( 7.448826589983275959, -6.376774720514420736, 21.05250386848070221 ) ) ;
#42746 = LINE ( 'NONE', #35123, #7662 ) ;
#42747 = CARTESIAN_POINT ( 'NONE',  ( -11.13288495942205536, 18.84158392345546318, -1.500000000000002220 ) ) ;
#42748 = PLANE ( 'NONE',  #70644 ) ;
#42749 = VERTEX_POINT ( 'NONE', #26909 ) ;
#42750 = LINE ( 'NONE', #73683, #59919 ) ;
#42751 = CARTESIAN_POINT ( 'NONE',  ( -75.52287095715006160, -24.99156044556120548, 7.747789690856173195 ) ) ;
#42752 = ORIENTED_EDGE ( 'NONE', *, *, #73559, .T. ) ;
#42753 = LINE ( 'NONE', #49872, #4172 ) ;
#42754 = ORIENTED_EDGE ( 'NONE', *, *, #18704, .T. ) ;
#42755 = CARTESIAN_POINT ( 'NONE',  ( -44.52287095715006160, -24.65952944569303895, 1.056160979905691910 ) ) ;
#42756 = CARTESIAN_POINT ( 'NONE',  ( -10.20961666403812096, -23.56687617480621455, 2.712351064733613537 ) ) ;
#42757 = CARTESIAN_POINT ( 'NONE',  ( 14.70648301983428397, -15.34743991077593250, -1.500000000000002220 ) ) ;
#42758 = CARTESIAN_POINT ( 'NONE',  ( 10.57556460110582286, 0.7139560615726621151, 8.999999999999994671 ) ) ;
#42759 = CARTESIAN_POINT ( 'NONE',  ( -26.48766330312332684, -24.75186131672143475, 3.017960868138962027 ) ) ;
#42760 = CARTESIAN_POINT ( 'NONE',  ( -85.65008181500884632, -23.48783264082476308, -1.443836473390099018 ) ) ;
#42761 = CARTESIAN_POINT ( 'NONE',  ( -68.50127936046202137, -24.34968618360933590, 0.1864209137778813363 ) ) ;
#42762 = AXIS2_PLACEMENT_3D ( 'NONE', #24290, #78054, #10064 ) ;
#42763 = ADVANCED_FACE ( 'NONE', ( #88818 ), #2263, .F. ) ;
#42764 = CARTESIAN_POINT ( 'NONE',  ( -44.62287095715004881, -24.64965695001468404, 8.947790433994187609 ) ) ;
#42765 = VERTEX_POINT ( 'NONE', #73588 ) ;
#42766 = CARTESIAN_POINT ( 'NONE',  ( -16.13938233076020268, 11.07636124087057183, 11.49999999999999645 ) ) ;
#42767 = CARTESIAN_POINT ( 'NONE',  ( -95.62287095715005592, -23.48783264082479150, -1.443836473390061936 ) ) ;
#42768 = AXIS2_PLACEMENT_3D ( 'NONE', #36773, #97174, #75817 ) ;
#42769 = B_SPLINE_CURVE_WITH_KNOTS ( 'NONE', 3,
 ( #68124, #99045, #29545, #60522 ),
 .UNSPECIFIED., .F., .F.,
 ( 4, 4 ),
 ( 0.000000000000000000, 0.0001000000000000028644 ),
 .UNSPECIFIED. ) ;
#42770 = CARTESIAN_POINT ( 'NONE',  ( -29.76915174891760429, -25.21382154147696042, 5.865244179202782959 ) ) ;
#42771 = VERTEX_POINT ( 'NONE', #66502 ) ;
#42772 = CARTESIAN_POINT ( 'NONE',  ( 4.332134589405623792, -6.376774720514427841, 21.69242924468134959 ) ) ;
#42773 = CARTESIAN_POINT ( 'NONE',  ( -99.74640623490535063, -25.31439576479845144, 5.397458638819514931 ) ) ;
#42774 = CARTESIAN_POINT ( 'NONE',  ( 21.57151214508649772, 0.000000000000000000, 0.000000000000000000 ) ) ;
#42775 = CARTESIAN_POINT ( 'NONE',  ( -81.01753736565918018, -25.03156042079280397, 7.476685952954507997 ) ) ;
#42776 = CARTESIAN_POINT ( 'NONE',  ( -13.08164486973500118, 14.69858247433046650, -1.500000000000002220 ) ) ;
#42777 = ORIENTED_EDGE ( 'NONE', *, *, #3278, .F. ) ;
#42778 = CARTESIAN_POINT ( 'NONE',  ( -91.62287095715004170, -29.50250243563736774, 8.947779886222139822 ) ) ;
#42779 = DIRECTION ( 'NONE',  ( -0.000000000000000000, 1.000000000000000000, -0.000000000000000000 ) ) ;
#42780 = EDGE_CURVE ( 'NONE', #80623, #47537, #44460, .T. ) ;
#42781 = DATE_TIME_ROLE ( 'classification_date' ) ;
#42782 = ORIENTED_EDGE ( 'NONE', *, *, #19817, .T. ) ;
#42783 = LINE ( 'NONE', #67122, #19195 ) ;
#42784 = LINE ( 'NONE', #2222, #40990 ) ;
#42785 = CARTESIAN_POINT ( 'NONE',  ( -55.66784212058755799, -23.48783264082475952, -1.443836473390099462 ) ) ;
#42786 = CARTESIAN_POINT ( 'NONE',  ( 19.75748517575715368, -5.965225279485572685, 28.87153971905864580 ) ) ;
#42787 = CARTESIAN_POINT ( 'NONE',  ( -80.91269838580346629, -25.14083923594767356, 2.947789366383930965 ) ) ;
#42788 = EDGE_CURVE ( 'NONE', #50770, #14217, #33478, .T. ) ;
#42789 = CARTESIAN_POINT ( 'NONE',  ( -69.34303308397305443, -25.31201785239418811, 6.209207263561717483 ) ) ;
#42790 = CARTESIAN_POINT ( 'NONE',  ( -79.52287095715006160, -24.65952944569304961, 1.056160979905698794 ) ) ;
#42791 = CARTESIAN_POINT ( 'NONE',  ( 13.74685606122050885, 14.44317598224977672, 11.49999999999998934 ) ) ;
#42792 = VECTOR ( 'NONE', #57544, 1000.000000000000000 ) ;
#42793 = CARTESIAN_POINT ( 'NONE',  ( -0.03481313173224404034, -22.59931665215008323, 1.725801405104978370 ) ) ;
#42794 = CARTESIAN_POINT ( 'NONE',  ( 7.614665684681447111, -18.39110272641453037, -1.500000000000002220 ) ) ;
#42795 = ORIENTED_EDGE ( 'NONE', *, *, #78039, .T. ) ;
#42796 = EDGE_CURVE ( 'NONE', #97929, #7781, #21273, .T. ) ;
#42797 = CARTESIAN_POINT ( 'NONE',  ( 16.89397143409390623, -5.876774720514426953, 16.89397143409405899 ) ) ;
#42798 = EDGE_CURVE ( 'NONE', #18086, #22543, #52249, .T. ) ;
#42799 = AXIS2_PLACEMENT_3D ( 'NONE', #87995, #89485, #50431 ) ;
#42800 = EDGE_CURVE ( 'NONE', #26418, #2990, #3867, .T. ) ;
#42801 = CYLINDRICAL_SURFACE ( 'NONE', #30087, 1.306876713926001354 ) ;
#42802 = CARTESIAN_POINT ( 'NONE',  ( 9.313311959400177642, -6.376774720514677419, -28.06297399545715976 ) ) ;
#42803 = DIRECTION ( 'NONE',  ( -1.000000000000000000, -0.000000000000000000, -0.000000000000000000 ) ) ;
#42804 = DIRECTION ( 'NONE',  ( -0.09824042138329590335, 0.9951627101165078093, 3.519298150595267489E-15 ) ) ;
#42805 = CARTESIAN_POINT ( 'NONE',  ( -51.15959938089677195, -25.22513071276370766, 3.603215203315445869 ) ) ;
#42806 = ORIENTED_EDGE ( 'NONE', *, *, #55786, .T. ) ;
#42807 = DIRECTION ( 'NONE',  ( -0.9978940991575084851, 0.000000000000000000, -0.06486421869277853025 ) ) ;
#42808 = CARTESIAN_POINT ( 'NONE',  ( -127.5894462411159225, -24.51314013834317151, 0.6176544820404252789 ) ) ;
#42809 = ORIENTED_EDGE ( 'NONE', *, *, #63272, .F. ) ;
#42810 = CARTESIAN_POINT ( 'NONE',  ( 20.17645099164838030, 1.678240329834772115, 11.49999999999998934 ) ) ;
#42811 = EDGE_CURVE ( 'NONE', #84010, #63074, #61357, .T. ) ;
#42812 = DIRECTION ( 'NONE',  ( 0.000000000000000000, -1.000000000000000000, 0.000000000000000000 ) ) ;
#42813 = B_SPLINE_CURVE_WITH_KNOTS ( 'NONE', 3,
 ( #62390, #93320, #54784, #49180 ),
 .UNSPECIFIED., .F., .F.,
 ( 4, 4 ),
 ( 0.5101502102554993368, 0.5191566415276147595 ),
 .UNSPECIFIED. ) ;
#42814 = DIRECTION ( 'NONE',  ( 0.000000000000000000, 0.000000000000000000, -1.000000000000000000 ) ) ;
#42815 = CYLINDRICAL_SURFACE ( 'NONE', #97884, 10.49999999999999289 ) ;
#42816 = VERTEX_POINT ( 'NONE', #61367 ) ;
#42817 = CARTESIAN_POINT ( 'NONE',  ( 30.43908124610669930, 1.684774720514424784, -13.86910542224428866 ) ) ;
#42818 = CARTESIAN_POINT ( 'NONE',  ( -2.243088942307695177, -5.876774720514407413, 19.14743589743590491 ) ) ;
#42819 = CARTESIAN_POINT ( 'NONE',  ( 7.608091486120485136, 18.53616061196756704, -1.500000000000002220 ) ) ;
#42820 = CARTESIAN_POINT ( 'NONE',  ( 16.07406896385161943, -13.52096256729613266, 11.49999999999999645 ) ) ;
#42821 = DIRECTION ( 'NONE',  ( -0.000000000000000000, -1.000000000000000000, -0.000000000000000000 ) ) ;
#42822 = CARTESIAN_POINT ( 'NONE',  ( -70.58658433434442259, -24.63419186844611275, 9.035850630976918652 ) ) ;
#42823 = CARTESIAN_POINT ( 'NONE',  ( -16.84257673422482426, -14.26466048179180568, 11.49999999999998934 ) ) ;
#42824 = EDGE_CURVE ( 'NONE', #909, #100104, #23768, .T. ) ;
#42825 = CARTESIAN_POINT ( 'NONE',  ( -28.98875734969026396, -5.965225279485572685, 10.11402280011862587 ) ) ;
#42826 = LINE ( 'NONE', #75248, #59775 ) ;
#42827 = LINE ( 'NONE', #11857, #67138 ) ;
#42828 = EDGE_CURVE ( 'NONE', #27734, #86526, #60100, .T. ) ;
#42829 = CARTESIAN_POINT ( 'NONE',  ( -72.60739634760311390, -23.48783264082477018, -1.443836473390095021 ) ) ;
#42830 = B_SPLINE_SURFACE_WITH_KNOTS ( 'NONE', 3, 3, ( 
 ( #82829, #7200, #30543, #44291 ),
 ( #14310, #67139, #75220, #45284 ),
 ( #76210, #37165, #53896, #13811 ),
 ( #45775, #67628, #98048, #6704 ),
 ( #13312, #76698, #38148, #44786 ),
 ( #60520, #46273, #59513, #5712 ),
 ( #98549, #37660, #29045, #68615 ) ),
 .UNSPECIFIED., .F., .F., .F.,
 ( 4, 3, 4 ),
 ( 4, 4 ),
 ( 0.0004766839783822517779, 0.1029713700210901639, 0.2054660560637980860 ),
 ( 0.1095218577375331737, 0.1105851154774898787 ),
 .UNSPECIFIED. ) ;
#42831 = FACE_OUTER_BOUND ( 'NONE', #93337, .T. ) ;
#42832 = ORIENTED_EDGE ( 'NONE', *, *, #56912, .T. ) ;
#42833 = EDGE_LOOP ( 'NONE', ( #68005, #94206, #5609, #86880 ) ) ;
#42834 = CARTESIAN_POINT ( 'NONE',  ( 15.58962545129234556, -1.684774720514426560, -26.91365498785467736 ) ) ;
#42835 = CARTESIAN_POINT ( 'NONE',  ( -61.59189125704995860, -25.07259839747099051, 7.371166918563575976 ) ) ;
#42836 = DIRECTION ( 'NONE',  ( -0.000000000000000000, -0.9513357669802769978, 0.3081562241202474572 ) ) ;
#42837 = CARTESIAN_POINT ( 'NONE',  ( 14.30100545221680441, -14.83292283143518375, -1.500000000000002220 ) ) ;
#42838 = ADVANCED_FACE ( 'NONE', ( #91789 ), #6060, .T. ) ;
#42839 = CARTESIAN_POINT ( 'NONE',  ( -0.8629811567608781653, -21.54619324973139172, 11.49999999999999645 ) ) ;
#42840 = ORIENTED_EDGE ( 'NONE', *, *, #97084, .T. ) ;
#42841 = PLANE ( 'NONE',  #49455 ) ;
#42842 = CARTESIAN_POINT ( 'NONE',  ( 6.658651924251966392, -5.876774720514415407, 20.11748569626183425 ) ) ;
#42843 = LINE ( 'NONE', #99088, #38345 ) ;
#42844 = CARTESIAN_POINT ( 'NONE',  ( -10.99827004860668822, -19.42154297629913628, 11.49999999999998934 ) ) ;
#42845 = EDGE_CURVE ( 'NONE', #42876, #38457, #77059, .T. ) ;
#42846 = CARTESIAN_POINT ( 'NONE',  ( -0.07959803473139406838, -22.01954088903999107, 0.3010598746230624956 ) ) ;
#42847 = DIRECTION ( 'NONE',  ( -1.000000000000000000, -3.773278334444166432E-23, -8.201307841325785021E-29 ) ) ;
#42848 = ORIENTED_EDGE ( 'NONE', *, *, #14761, .T. ) ;
#42849 = ADVANCED_FACE ( 'NONE', ( #15167 ), #77557, .F. ) ;
#42850 = CARTESIAN_POINT ( 'NONE',  ( -6.914873625533462409, 5.965225279485572685, 29.95171384920748281 ) ) ;
#42851 = CARTESIAN_POINT ( 'NONE',  ( -51.45240106148425241, -25.30046445047157633, 4.640179479081717240 ) ) ;
#42852 = CARTESIAN_POINT ( 'NONE',  ( 20.34438994040483806, -4.565235006643893811, -1.500000000000002220 ) ) ;
#42853 = EDGE_LOOP ( 'NONE', ( #43693, #39333, #74953, #35227 ) ) ;
#42854 = VECTOR ( 'NONE', #65902, 1000.000000000000114 ) ;
#42856 = ORIENTED_EDGE ( 'NONE', *, *, #47259, .T. ) ;
#42855 = CARTESIAN_POINT ( 'NONE',  ( 15.10352928271630724, -3.582999323269832725, -27.29968155418892195 ) ) ;
#42857 = ORIENTED_EDGE ( 'NONE', *, *, #56433, .F. ) ;
#42858 = DIRECTION ( 'NONE',  ( -0.000000000000000000, 2.173523156925979552E-06, -0.9999999999976378895 ) ) ;
#42859 = CARTESIAN_POINT ( 'NONE',  ( -14.96386864383857329, 14.77685607883014640, -1.500000000000002220 ) ) ;
#42860 = EDGE_LOOP ( 'NONE', ( #84731, #19635, #85238, #78021 ) ) ;
#42861 = DIRECTION ( 'NONE',  ( -0.000000000000000000, -0.000000000000000000, -1.000000000000000000 ) ) ;
#42862 = CARTESIAN_POINT ( 'NONE',  ( -48.97769291515528067, -25.29015023533645490, 5.627382122205519366 ) ) ;
#42863 = CARTESIAN_POINT ( 'NONE',  ( -120.5910566015817551, -24.15602025860899360, 10.28564288303534902 ) ) ;
#42864 = CARTESIAN_POINT ( 'NONE',  ( -80.96226385320382235, -25.13069340115295702, 2.947789388436138580 ) ) ;
#42865 = DIRECTION ( 'NONE',  ( 0.000000000000000000, 2.173523156925980399E-06, -0.9999999999976378895 ) ) ;
#42866 = CARTESIAN_POINT ( 'NONE',  ( -20.21959982808627032, -7.803091810188320210, -1.500000000000002220 ) ) ;
#42867 = CARTESIAN_POINT ( 'NONE',  ( -80.52846833935618065, -25.12224391807531987, 7.100555464394792793 ) ) ;
#42869 = ORIENTED_EDGE ( 'NONE', *, *, #89580, .F. ) ;
#42868 = CARTESIAN_POINT ( 'NONE',  ( 20.56042274393015035, -8.519965759701490171, 11.49999999999999645 ) ) ;
#42870 = CARTESIAN_POINT ( 'NONE',  ( -69.62287095715005592, -23.47596703998600631, 11.44779298504227683 ) ) ;
#42871 = CARTESIAN_POINT ( 'NONE',  ( 29.68479148105952703, 1.477225279485574028, -9.431263391055123790 ) ) ;
#42872 = FACE_OUTER_BOUND ( 'NONE', #94012, .T. ) ;
#42873 = ORIENTED_EDGE ( 'NONE', *, *, #93635, .F. ) ;
#42874 = AXIS2_PLACEMENT_3D ( 'NONE', #87123, #25725, #56702 ) ;
#42876 = VERTEX_POINT ( 'NONE', #46639 ) ;
#42875 = CARTESIAN_POINT ( 'NONE',  ( -40.62287095715004170, -24.63287334234176384, 0.9662140553045526215 ) ) ;
#42877 = ORIENTED_EDGE ( 'NONE', *, *, #13912, .T. ) ;
#42878 = CARTESIAN_POINT ( 'NONE',  ( -100.5775025149089572, -25.13380690292655828, 7.097842372401126809 ) ) ;
#42879 = CARTESIAN_POINT ( 'NONE',  ( 13.10664265030973930, -0.3587747205144256601, -27.62597719988137612 ) ) ;
#42880 = DIRECTION ( 'NONE',  ( 0.000000000000000000, 0.000000000000000000, -1.000000000000000000 ) ) ;
#42881 = CARTESIAN_POINT ( 'NONE',  ( -80.62287095715004170, -23.48783264082478439, -1.443836473390065489 ) ) ;
#42882 = EDGE_LOOP ( 'NONE', ( #67712, #80628, #86032, #43229 ) ) ;
#42883 = CARTESIAN_POINT ( 'NONE',  ( -130.5728709571500872, -24.91553454762389208, 1.571120308003612687 ) ) ;
#42884 = CARTESIAN_POINT ( 'NONE',  ( 9.841385673706204429, 20.17164819615926064, -1.500000000000002220 ) ) ;
#42885 = ORIENTED_EDGE ( 'NONE', *, *, #2706, .F. ) ;
#42886 = CARTESIAN_POINT ( 'NONE',  ( -99.29687923781919778, -29.50249635395236325, 6.149702963151822743 ) ) ;
#42887 = CARTESIAN_POINT ( 'NONE',  ( -94.60069879652984071, -23.48786465467241413, 11.44779295918254469 ) ) ;
#42888 = CARTESIAN_POINT ( 'NONE',  ( 7.732492002959944877, 5.356774720515138810, -27.16032169580908473 ) ) ;
#42889 = LINE ( 'NONE', #75807, #36869 ) ;
#42890 = CARTESIAN_POINT ( 'NONE',  ( -30.59799462776630108, -24.66513809378595568, 8.909134979017297340 ) ) ;
#42891 = CARTESIAN_POINT ( 'NONE',  ( 5.347671334029483248, -18.86178030415664963, 11.49999999999998934 ) ) ;
#42892 = CARTESIAN_POINT ( 'NONE',  ( -46.60715227236160274, -23.73766607897669800, -1.055555164236460008 ) ) ;
#42893 = ORIENTED_EDGE ( 'NONE', *, *, #56660, .T. ) ;
#42894 = AXIS2_PLACEMENT_3D ( 'NONE', #67863, #45524, #91179 ) ;
#42895 = CARTESIAN_POINT ( 'NONE',  ( -11.62584540149672385, -18.10649092712023389, 11.49999999999998934 ) ) ;
#42896 = B_SPLINE_CURVE_WITH_KNOTS ( 'NONE', 3,
 ( #15473, #22571, #31199, #6871 ),
 .UNSPECIFIED., .F., .F.,
 ( 4, 4 ),
 ( 0.000000000000000000, 9.999999999999592548E-05 ),
 .UNSPECIFIED. ) ;
#42897 = CARTESIAN_POINT ( 'NONE',  ( 13.74975846015576586, -5.965225279485572685, -27.72022515045486557 ) ) ;
#42898 = CARTESIAN_POINT ( 'NONE',  ( -71.19450251067907232, -25.12219042401383007, 6.630762628979895545 ) ) ;
#42899 = CARTESIAN_POINT ( 'NONE',  ( -100.5562042904833788, -23.48783264082478439, -1.443836473390062380 ) ) ;
#42900 = CARTESIAN_POINT ( 'NONE',  ( -8.376690734369036662, 11.49999999999999645, 2.100000000000000089 ) ) ;
#42901 = CARTESIAN_POINT ( 'NONE',  ( 22.64363655503811046, -4.068770074275382953, -1.500000000000002220 ) ) ;
#42902 = EDGE_CURVE ( 'NONE', #39331, #77715, #63851, .T. ) ;
#42903 = CALENDAR_DATE ( 2026, 9, 10 ) ;
#42904 = DIRECTION ( 'NONE',  ( 0.000000000000000000, 0.000000000000000000, 1.000000000000000000 ) ) ;
#42905 = CARTESIAN_POINT ( 'NONE',  ( -53.57809818791832157, -24.65952944569304250, 1.056160979905695463 ) ) ;
#42906 = CARTESIAN_POINT ( 'NONE',  ( 12.55954966114946458, -15.69740789531843461, 11.49999999999999645 ) ) ;
#42907 = CARTESIAN_POINT ( 'NONE',  ( -56.52287095715009002, -23.48783264082476308, -1.443836473390091690 ) ) ;
#42908 = CARTESIAN_POINT ( 'NONE',  ( -32.47727307158466914, -24.66019654487198665, 8.947790411086131712 ) ) ;
#42909 = ADVANCED_FACE ( 'NONE', ( #92295 ), #30394, .T. ) ;
#42910 = DIRECTION ( 'NONE',  ( -0.000000000000000000, 2.173523156925979552E-06, -0.9999999999976378895 ) ) ;
#42911 = CARTESIAN_POINT ( 'NONE',  ( -113.5895376238167103, -23.48783264082479150, -1.443836473390060160 ) ) ;
#42912 = CARTESIAN_POINT ( 'NONE',  ( -126.6228709571500559, -23.48786465467242124, 11.44779295918253403 ) ) ;
#42913 = CARTESIAN_POINT ( 'NONE',  ( 6.283368587668265448, -18.83516890145298106, -1.500000000000002220 ) ) ;
#42914 = CARTESIAN_POINT ( 'NONE',  ( -113.5222246106276884, -23.48783264082477373, -1.443836473390084807 ) ) ;
#42915 = CARTESIAN_POINT ( 'NONE',  ( -16.18664964019209052, -11.25563402961023662, -1.500000000000002220 ) ) ;
#42916 = EDGE_CURVE ( 'NONE', #16850, #63089, #37064, .T. ) ;
#42917 = CARTESIAN_POINT ( 'NONE',  ( 0.000000000000000000, -6.943225279485572443, 0.000000000000000000 ) ) ;
#42918 = EDGE_CURVE ( 'NONE', #64205, #67134, #14054, .T. ) ;
#42919 = B_SPLINE_CURVE_WITH_KNOTS ( 'NONE', 3,
 ( #14642, #76527, #7033, #86656, #9033, #38981, #39986, #22740 ),
 .UNSPECIFIED., .F., .F.,
 ( 4, 2, 2, 4 ),
 ( 0.000000000000000000, 0.002001079623178225828, 0.003001619434767337224, 0.004002159246356448187 ),
 .UNSPECIFIED. ) ;
#42920 = APPROVAL_DATE_TIME ( #48538, #9079 ) ;
#42921 = EDGE_CURVE ( 'NONE', #33110, #27352, #91519, .T. ) ;
#42922 = CARTESIAN_POINT ( 'NONE',  ( -4.926336369345164279, 5.965225279485592225, -28.61095484066304451 ) ) ;
#42923 = CARTESIAN_POINT ( 'NONE',  ( -79.52287095715004739, -24.33927499327855060, 9.819080762295811837 ) ) ;
#42924 = CARTESIAN_POINT ( 'NONE',  ( 20.46650637700042097, -2.330123182410055893, 11.49999999999999645 ) ) ;
#42925 = CIRCLE ( 'NONE', #21810, 0.8500000000000017542 ) ;
#42926 = CARTESIAN_POINT ( 'NONE',  ( -42.62287095715004881, -23.48783264082477373, -1.443836473390072817 ) ) ;
#42927 = CARTESIAN_POINT ( 'NONE',  ( -15.40814491850785650, 16.58152744545821022, 11.49999999999999645 ) ) ;
#42928 = VERTEX_POINT ( 'NONE', #446 ) ;
#42929 = CARTESIAN_POINT ( 'NONE',  ( 8.071512145086526147, -7.528487854913507249, -4.499999999999999112 ) ) ;
#42930 = CARTESIAN_POINT ( 'NONE',  ( -102.5562042904833788, -24.65952944569305316, 1.056160979905701236 ) ) ;
#42931 = CARTESIAN_POINT ( 'NONE',  ( -74.62287095715004170, -24.66019654487199375, 8.947790411086129936 ) ) ;
#42932 = EDGE_CURVE ( 'NONE', #51201, #42129, #24777, .T. ) ;
#42933 = CARTESIAN_POINT ( 'NONE',  ( -26.47413879005073056, -24.61460015870519058, 7.801149999016648628 ) ) ;
#42934 = AXIS2_PLACEMENT_3D ( 'NONE', #63177, #94103, #86497 ) ;
#42935 = DIRECTION ( 'NONE',  ( 0.000000000000000000, -0.9999999999976377785, -2.173523156925979128E-06 ) ) ;
#42936 = ORIENTED_EDGE ( 'NONE', *, *, #22208, .F. ) ;
#42937 = ORIENTED_EDGE ( 'NONE', *, *, #37342, .T. ) ;
#42938 = ADVANCED_FACE ( 'NONE', ( #31401 ), #56262, .T. ) ;
#42939 = CARTESIAN_POINT ( 'NONE',  ( -99.36343569840310863, -25.21460787793245117, 6.488302719685625775 ) ) ;
#42940 = CARTESIAN_POINT ( 'NONE',  ( 15.09361930729867574, -17.17024899132524496, -1.500000000000002220 ) ) ;
#42941 = DIRECTION ( 'NONE',  ( -0.000000000000000000, 1.000000000000000000, -0.000000000000000000 ) ) ;
#42942 = CARTESIAN_POINT ( 'NONE',  ( -17.67581969798968444, -12.36387604476075097, -1.500000000000002220 ) ) ;
#42943 = CARTESIAN_POINT ( 'NONE',  ( -19.69812919673063689, 0.3587747205143964613, -22.00173861453436430 ) ) ;
#42944 = CARTESIAN_POINT ( 'NONE',  ( -0.02075734969026423599, -5.965225279485572685, -29.05397719988136984 ) ) ;
#42945 = CARTESIAN_POINT ( 'NONE',  ( -8.307687032909205627, 20.95097986170506488, 11.49999999999999645 ) ) ;
#42946 = ORIENTED_EDGE ( 'NONE', *, *, #73179, .T. ) ;
#42947 = CARTESIAN_POINT ( 'NONE',  ( -43.50598925632350245, -23.96119346886880308, -0.6495511937831988103 ) ) ;
#42948 = CARTESIAN_POINT ( 'NONE',  ( -3.625624329714521643, -21.66436044012089468, 11.49999999999998934 ) ) ;
#42949 = EDGE_CURVE ( 'NONE', #3684, #52365, #8149, .T. ) ;
#42950 = DIRECTION ( 'NONE',  ( 0.000000000000000000, 0.000000000000000000, 1.000000000000000000 ) ) ;
#42951 = CARTESIAN_POINT ( 'NONE',  ( -118.5562042904834357, -23.48783264082479505, -1.443836473390058828 ) ) ;
#42952 = ORIENTED_EDGE ( 'NONE', *, *, #16891, .F. ) ;
#42953 = CARTESIAN_POINT ( 'NONE',  ( -63.62287095715003460, -24.33927499327854704, 9.819080762295815390 ) ) ;
#42954 = DIRECTION ( 'NONE',  ( 0.000000000000000000, 0.000000000000000000, -1.000000000000000000 ) ) ;
#42955 = EDGE_LOOP ( 'NONE', ( #33818, #79424, #40915, #61322, #29120, #2746 ) ) ;
#42956 = CARTESIAN_POINT ( 'NONE',  ( -77.62287095715005592, -23.72747288104441665, -1.053458166803662444 ) ) ;
#42957 = EDGE_LOOP ( 'NONE', ( #89876, #98710, #26714, #90982 ) ) ;
#42958 = VERTEX_POINT ( 'NONE', #48140 ) ;
#42959 = ORIENTED_EDGE ( 'NONE', *, *, #1325, .F. ) ;
#42960 = CARTESIAN_POINT ( 'NONE',  ( -49.44228279013045579, -25.29936970972777033, 5.641479429678947888 ) ) ;
#42961 = DIRECTION ( 'NONE',  ( -3.773278334453080206E-23, 0.9999999999976377785, 2.173523156925979975E-06 ) ) ;
#42962 = PLANE ( 'NONE',  #30935 ) ;
#42963 = CARTESIAN_POINT ( 'NONE',  ( 11.27307661227339430, 16.98952936956587934, -1.500000000000002220 ) ) ;
#42964 = ORIENTED_EDGE ( 'NONE', *, *, #87417, .T. ) ;
#42965 = CARTESIAN_POINT ( 'NONE',  ( -0.9827876235267493099, -5.876774720514415407, 19.81240905262004404 ) ) ;
#42966 = CARTESIAN_POINT ( 'NONE',  ( -29.48128483383218068, -24.42720452128061126, 9.386484716961749797 ) ) ;
#42967 = EDGE_CURVE ( 'NONE', #32974, #28046, #29888, .T. ) ;
#42968 = CARTESIAN_POINT ( 'NONE',  ( -105.6271250482996322, -24.63355581998386157, 0.9682620441943899925 ) ) ;
#42969 = LINE ( 'NONE', #64832, #96650 ) ;
#42970 = ORIENTED_EDGE ( 'NONE', *, *, #29050, .F. ) ;
#42971 = DIRECTION ( 'NONE',  ( 0.000000000000000000, -1.000000000000000000, 0.000000000000000000 ) ) ;
#42972 = CARTESIAN_POINT ( 'NONE',  ( -33.55620429048339304, -24.65952944569303895, 1.056160979905688801 ) ) ;
#42973 = CIRCLE ( 'NONE', #5713, 6.119803529381342422 ) ;
#42974 = ORIENTED_EDGE ( 'NONE', *, *, #49168, .F. ) ;
#42975 = CARTESIAN_POINT ( 'NONE',  ( -20.76960556195881225, -0.3855258213679747525, -1.500000000000002220 ) ) ;
#42976 = ADVANCED_FACE ( 'NONE', ( #62878 ), #93286, .T. ) ;
#42977 = ORIENTED_EDGE ( 'NONE', *, *, #36548, .F. ) ;
#42979 = ORIENTED_EDGE ( 'NONE', *, *, #90095, .F. ) ;
#42978 = CARTESIAN_POINT ( 'NONE',  ( -11.64875734969026233, 0.3587747205144265483, 31.02402280011862246 ) ) ;
#42980 = CARTESIAN_POINT ( 'NONE',  ( 5.097264368846952998, 6.475225279485573360, -27.56135813788808164 ) ) ;
#42981 = CARTESIAN_POINT ( 'NONE',  ( -51.90571684870070612, -25.27193873804239033, 5.908765195229332079 ) ) ;
#42982 = VERTEX_POINT ( 'NONE', #71478 ) ;
#42983 = ORIENTED_EDGE ( 'NONE', *, *, #6344, .T. ) ;
#42984 = PLANE ( 'NONE',  #73703 ) ;
#42985 = FACE_OUTER_BOUND ( 'NONE', #25554, .T. ) ;
#42986 = CARTESIAN_POINT ( 'NONE',  ( -4.495793269230770939, -5.876774720514410077, 19.27714342948718595 ) ) ;
#42987 = B_SPLINE_CURVE_WITH_KNOTS ( 'NONE', 3,
 ( #70366, #62264, #93189, #70876 ),
 .UNSPECIFIED., .F., .F.,
 ( 4, 4 ),
 ( 7.248525107586175442E-06, 0.001219383299454008997 ),
 .UNSPECIFIED. ) ;
#42988 = CARTESIAN_POINT ( 'NONE',  ( -43.59362069740146950, -24.15620529776627379, 10.23563542870661180 ) ) ;
#42990 = VERTEX_POINT ( 'NONE', #40013 ) ;
#42989 = CARTESIAN_POINT ( 'NONE',  ( 0.6065052782250800467, 22.08157775750015617, 11.49999999999999645 ) ) ;
#42991 = DIRECTION ( 'NONE',  ( -1.000000000000000000, 0.000000000000000000, 0.000000000000000000 ) ) ;
#42992 = CARTESIAN_POINT ( 'NONE',  ( -2.075279548881721947, -22.52154899835045043, 11.49999999999998934 ) ) ;
#42994 = EDGE_LOOP ( 'NONE', ( #89243, #75395, #15297, #59118 ) ) ;
#42993 = CARTESIAN_POINT ( 'NONE',  ( -115.5155043013981953, -24.63419186844613051, 9.035850630976920428 ) ) ;
#42995 = ORIENTED_EDGE ( 'NONE', *, *, #77247, .F. ) ;
#42996 = CARTESIAN_POINT ( 'NONE',  ( -80.60277405640064785, -25.31556075360760261, 4.974435291001888082 ) ) ;
#42997 = AXIS2_PLACEMENT_3D ( 'NONE', #4502, #75979, #12596 ) ;
#42998 = CARTESIAN_POINT ( 'NONE',  ( -42.52287095715005449, -24.64898659630367206, 1.056161002820819261 ) ) ;
#42999 = VERTEX_POINT ( 'NONE', #70972 ) ;
#43000 = CARTESIAN_POINT ( 'NONE',  ( -6.202713861520617655, -20.23501359363181962, 11.49999999999998934 ) ) ;
#43001 = CARTESIAN_POINT ( 'NONE',  ( 5.402409956206937203, -5.876774720514424288, 21.18719775722114917 ) ) ;
#43002 = DIRECTION ( 'NONE',  ( -3.773278334453079030E-23, 0.9999999999976377785, 2.173523156925979128E-06 ) ) ;
#43003 = CARTESIAN_POINT ( 'NONE',  ( 17.40631026334068565, 13.93540124644318645, -1.500000000000002220 ) ) ;
#43004 = PLANE ( 'NONE',  #85693 ) ;
#43005 = AXIS2_PLACEMENT_3D ( 'NONE', #85010, #15494, #22107 ) ;
#43006 = ORIENTED_EDGE ( 'NONE', *, *, #46226, .T. ) ;
#43007 = CARTESIAN_POINT ( 'NONE',  ( -78.55620429048339304, -23.47593901973091235, -1.443836447539004642 ) ) ;
#43008 = CARTESIAN_POINT ( 'NONE',  ( -48.55620429048338593, -24.65952944569304606, 1.056160979905694797 ) ) ;
#43009 = AXIS2_PLACEMENT_3D ( 'NONE', #32830, #54675, #17603 ) ;
#43010 = CARTESIAN_POINT ( 'NONE',  ( -29.52287095715006160, -23.38909342368989641, 11.44779306042727285 ) ) ;
#43011 = B_SPLINE_CURVE_WITH_KNOTS ( 'NONE', 3,
 ( #69846, #9940, #1340, #40398, #1840, #71854 ),
 .UNSPECIFIED., .F., .F.,
 ( 4, 2, 4 ),
 ( 6.384118694913733240E-06, 0.001386860460836522764, 0.002767336802978131484 ),
 .UNSPECIFIED. ) ;
#43012 = CARTESIAN_POINT ( 'NONE',  ( -45.22287095715005023, -23.47596703998600276, 11.44779298504227683 ) ) ;
#43013 = CARTESIAN_POINT ( 'NONE',  ( 10.93668938013857783, -16.14717738681254033, 11.49999999999998934 ) ) ;
#43014 = CARTESIAN_POINT ( 'NONE',  ( 21.23773461148298836, -3.020459416520930862, 11.49999999999998934 ) ) ;
#43015 = CARTESIAN_POINT ( 'NONE',  ( -0.6735982426299428338, -5.876774720514410077, 19.16400979764068069 ) ) ;
#43016 = CARTESIAN_POINT ( 'NONE',  ( -108.6228709571500417, -23.48786465467242479, 11.44779295918253759 ) ) ;
#43017 = CARTESIAN_POINT ( 'NONE',  ( -77.59210467935486122, -24.15543982623907482, -0.2315651400026658147 ) ) ;
#43018 = CARTESIAN_POINT ( 'NONE',  ( -19.65108876255925807, -11.61119296138784662, -1.500000000000002220 ) ) ;
#43019 = CARTESIAN_POINT ( 'NONE',  ( -39.52287095715007581, -23.72747288104470087, -1.053458166803227680 ) ) ;
#43020 = DIRECTION ( 'NONE',  ( 3.773278334444167608E-23, -1.000000000000000000, 0.000000000000000000 ) ) ;
#43021 = CARTESIAN_POINT ( 'NONE',  ( 7.614665684681447111, -18.39110272641453037, 11.49999999999999645 ) ) ;
#43022 = CARTESIAN_POINT ( 'NONE',  ( -104.5196659495136657, -23.73766607897670866, -1.055555164236449572 ) ) ;
#43023 = EDGE_CURVE ( 'NONE', #65522, #82260, #54754, .T. ) ;
#43024 = ADVANCED_FACE ( 'NONE', ( #1462 ), #16669, .T. ) ;
#43025 = LINE ( 'NONE', #87190, #95950 ) ;
#43026 = CARTESIAN_POINT ( 'NONE',  ( -76.58953762381673869, -23.47596703998600276, 11.44779298504227683 ) ) ;
#43027 = EDGE_LOOP ( 'NONE', ( #28310, #54967, #56570, #82748 ) ) ;
#43028 = DIRECTION ( 'NONE',  ( 3.773278334444167608E-23, -1.000000000000000000, 0.000000000000000000 ) ) ;
#43029 = CARTESIAN_POINT ( 'NONE',  ( -31.22214303690239134, -25.16202561908117730, 2.791798636425737445 ) ) ;
#43030 = EDGE_CURVE ( 'NONE', #50095, #881, #88099, .T. ) ;
#43031 = CARTESIAN_POINT ( 'NONE',  ( -6.179238894844691465, -20.81818906610659425, 11.49999999999998934 ) ) ;
#43032 = DIRECTION ( 'NONE',  ( -0.1478094111296165691, 0.9890158633619158257, -0.000000000000000000 ) ) ;
#43033 = CARTESIAN_POINT ( 'NONE',  ( 10.86043079284791091, -16.25897383129715834, -1.500000000000002220 ) ) ;
#43034 = ADVANCED_FACE ( 'NONE', ( #40527 ), #47138, .T. ) ;
#43035 = CARTESIAN_POINT ( 'NONE',  ( -55.66784890944978059, -23.48786465467241058, 11.44779295918254647 ) ) ;
#43036 = ORIENTED_EDGE ( 'NONE', *, *, #2351, .T. ) ;
#43037 = PERSON_AND_ORGANIZATION ( #88765, #76544 ) ;
#43038 = AXIS2_PLACEMENT_3D ( 'NONE', #85209, #38536, #61892 ) ;
#43039 = CARTESIAN_POINT ( 'NONE',  ( -112.5228709571500616, -29.50250243563736774, 8.947779886222136270 ) ) ;
#43040 = CARTESIAN_POINT ( 'NONE',  ( 9.418145840992488971, -18.15903486995133065, 11.49999999999999645 ) ) ;
#43041 = CARTESIAN_POINT ( 'NONE',  ( 11.44401587981593060, -6.475225279485572472, -27.05278809890034353 ) ) ;
#43042 = CARTESIAN_POINT ( 'NONE',  ( -86.52287095715006160, -24.64965694238575011, 8.947790433994196491 ) ) ;
#43043 = EDGE_CURVE ( 'NONE', #61226, #96695, #52895, .T. ) ;
#43044 = ORIENTED_EDGE ( 'NONE', *, *, #63206, .F. ) ;
#43045 = DIRECTION ( 'NONE',  ( 0.000000000000000000, 0.000000000000000000, 1.000000000000000000 ) ) ;
#43046 = DIRECTION ( 'NONE',  ( 0.8369330630277727057, 0.000000000000000000, -0.5473052603538087757 ) ) ;
#43047 = DIRECTION ( 'NONE',  ( -1.000000000000000000, -3.773278334444166432E-23, -8.201307841325785021E-29 ) ) ;
#43048 = B_SPLINE_CURVE_WITH_KNOTS ( 'NONE', 3,
 ( #59356, #20771, #36011, #90301, #60865, #7062 ),
 .UNSPECIFIED., .F., .F.,
 ( 4, 2, 4 ),
 ( 6.391158118964604309E-06, 0.001387004593080786580, 0.002767618028042608501 ),
 .UNSPECIFIED. ) ;
#43049 = CARTESIAN_POINT ( 'NONE',  ( -108.5228709571500616, -23.48786465467241769, 11.44779295918253936 ) ) ;
#43050 = EDGE_LOOP ( 'NONE', ( #49179, #42321, #28749, #2951 ) ) ;
#43051 = CARTESIAN_POINT ( 'NONE',  ( 5.730633878096764278, -6.376774720514418959, 20.45679216967608838 ) ) ;
#43052 = CARTESIAN_POINT ( 'NONE',  ( 22.97298546869389568, 1.202750762487129199, 11.49999999999999645 ) ) ;
#43053 = CARTESIAN_POINT ( 'NONE',  ( 0.9741843557120299923, -22.74547949729550922, -1.500000000000002220 ) ) ;
#43054 = CARTESIAN_POINT ( 'NONE',  ( 3.879810481058463711, -6.376774720514427841, 21.83835767234735670 ) ) ;
#43055 = CARTESIAN_POINT ( 'NONE',  ( -93.92287095715012413, -23.47593901973090880, -1.443836447538997314 ) ) ;
#43056 = CARTESIAN_POINT ( 'NONE',  ( 2.499999999999988454, 22.00000000000000000, 2.100000000000000089 ) ) ;
#43057 = DIRECTION ( 'NONE',  ( -2.352173255807796056E-16, 0.000000000000000000, 1.000000000000000000 ) ) ;
#43058 = CARTESIAN_POINT ( 'NONE',  ( -63.52287095715006160, -29.50248528299804818, 1.056150453629034924 ) ) ;
#43059 = CARTESIAN_POINT ( 'NONE',  ( -21.47987282208850601, -4.139150239982721580, -1.500000000000002220 ) ) ;
#43060 = CARTESIAN_POINT ( 'NONE',  ( 8.500000000000000000, 0.000000000000000000, 3.750000000000000000 ) ) ;
#43061 = CIRCLE ( 'NONE', #26828, 0.2999999999999981570 ) ;
#43062 = CARTESIAN_POINT ( 'NONE',  ( -34.62287095715005592, -24.64965695001467694, 8.947790433994189385 ) ) ;
#43063 = CARTESIAN_POINT ( 'NONE',  ( 25.05730599792488178, -500000.0000000000582, -18.59674224247031304 ) ) ;
#43064 = CARTESIAN_POINT ( 'NONE',  ( -58.63232380827055579, -24.34968618360933945, 0.1864209137778795045 ) ) ;
#43065 = EDGE_LOOP ( 'NONE', ( #1329, #73290, #30199, #14055 ) ) ;
#43066 = CARTESIAN_POINT ( 'NONE',  ( -15.93830457579706739, -12.76012858937699335, -1.500000000000002220 ) ) ;
#43067 = ORIENTED_EDGE ( 'NONE', *, *, #31016, .T. ) ;
#43068 = VECTOR ( 'NONE', #54860, 1000.000000000000114 ) ;
#43069 = ORIENTED_EDGE ( 'NONE', *, *, #19127, .F. ) ;
#43070 = EDGE_LOOP ( 'NONE', ( #11533, #69880, #60314, #28457 ) ) ;
#43071 = ORIENTED_EDGE ( 'NONE', *, *, #89960, .F. ) ;
#43072 = CARTESIAN_POINT ( 'NONE',  ( -1.973530150111237003, 22.95712487800313539, 11.49999999999998934 ) ) ;
#43073 = DIRECTION ( 'NONE',  ( 0.000000000000000000, 1.000000000000000000, 0.000000000000000000 ) ) ;
#43074 = CARTESIAN_POINT ( 'NONE',  ( 14.71488472389458124, -13.84269218943631508, -1.500000000000002220 ) ) ;
#43075 = VECTOR ( 'NONE', #43057, 1000.000000000000000 ) ;
#43076 = ORIENTED_EDGE ( 'NONE', *, *, #48085, .F. ) ;
#43077 = EDGE_CURVE ( 'NONE', #65310, #35855, #52707, .T. ) ;
#43078 = LINE ( 'NONE', #96356, #94704 ) ;
#43079 = CARTESIAN_POINT ( 'NONE',  ( 8.071512145086529699, -9.528487854913505473, 4.500000000000002665 ) ) ;
#43080 = VECTOR ( 'NONE', #90832, 999.9999999999998863 ) ;
#43081 = CARTESIAN_POINT ( 'NONE',  ( -95.63175277689521181, -24.40034930558991633, 0.3402023900116099009 ) ) ;
#43082 = PLANE ( 'NONE',  #31834 ) ;
#43084 = ORIENTED_EDGE ( 'NONE', *, *, #28242, .T. ) ;
#43083 = CARTESIAN_POINT ( 'NONE',  ( 6.831138157384286203, 20.27010762675863731, 11.49999999999999645 ) ) ;
#43085 = DIRECTION ( 'NONE',  ( 1.000000000000000000, 4.476705744456278313E-16, 0.000000000000000000 ) ) ;
#43086 = ORIENTED_EDGE ( 'NONE', *, *, #99459, .T. ) ;
#43087 = CARTESIAN_POINT ( 'NONE',  ( 5.670930919660429836, -21.52877996283707418, 11.49999999999998934 ) ) ;
#43088 = B_SPLINE_CURVE_WITH_KNOTS ( 'NONE', 3,
 ( #86471, #57048, #63152, #1250 ),
 .UNSPECIFIED., .F., .F.,
 ( 4, 4 ),
 ( 0.000000000000000000, 9.999999999998897304E-05 ),
 .UNSPECIFIED. ) ;
#43089 = CARTESIAN_POINT ( 'NONE',  ( -20.55277978778089576, -2.218614319624547360, -1.500000000000002220 ) ) ;
#43090 = EDGE_CURVE ( 'NONE', #35820, #36659, #44349, .T. ) ;
#43091 = ORIENTED_EDGE ( 'NONE', *, *, #53893, .T. ) ;
#43092 = CARTESIAN_POINT ( 'NONE',  ( -2.499999999999993339, 4.999999999999997335, 2.100000000000000089 ) ) ;
#43093 = ORIENTED_EDGE ( 'NONE', *, *, #67681, .F. ) ;
#43094 = CARTESIAN_POINT ( 'NONE',  ( -129.5228709571499905, -24.50216790748206819, 0.6166512839542598323 ) ) ;
#43095 = ORIENTED_EDGE ( 'NONE', *, *, #70924, .T. ) ;
#43096 = CARTESIAN_POINT ( 'NONE',  ( 10.22568704553358643, -3.316774720514425567, -27.02513721610328901 ) ) ;
#43097 = CARTESIAN_POINT ( 'NONE',  ( -15.06743543786183714, 14.52697759824333090, -1.500000000000002220 ) ) ;
#43098 = CARTESIAN_POINT ( 'NONE',  ( -21.55542221127511482, -4.010009934288176758, 11.49999999999999645 ) ) ;
#43099 = CARTESIAN_POINT ( 'NONE',  ( -37.52762035705108445, -24.66019654487199730, 8.947790411086113949 ) ) ;
#43100 = CARTESIAN_POINT ( 'NONE',  ( -1.797493081057526032, -22.44471576765463183, 11.49999999999998934 ) ) ;
#43101 = CARTESIAN_POINT ( 'NONE',  ( 5.581485548573628996, 20.18083795961418403, -1.500000000000002220 ) ) ;
#43102 = CARTESIAN_POINT ( 'NONE',  ( -26.09708441595108397, -24.88148730279706911, 5.016021623328582812 ) ) ;
#43103 = CARTESIAN_POINT ( 'NONE',  ( -57.62287095715004881, -29.50247984919015209, -1.443849546365056913 ) ) ;
#43104 = CARTESIAN_POINT ( 'NONE',  ( -119.6241211350181715, -24.51419770103158768, 9.386484678747159194 ) ) ;
#43105 = FACE_OUTER_BOUND ( 'NONE', #79995, .T. ) ;
#43106 = VERTEX_POINT ( 'NONE', #8568 ) ;
#43107 = VERTEX_POINT ( 'NONE', #55256 ) ;
#43108 = ORIENTED_EDGE ( 'NONE', *, *, #62915, .T. ) ;
#43109 = CARTESIAN_POINT ( 'NONE',  ( -66.63133949696768354, -24.34968618360933235, 0.1864209137778773395 ) ) ;
#43110 = ORIENTED_EDGE ( 'NONE', *, *, #60776, .T. ) ;
#43111 = CARTESIAN_POINT ( 'NONE',  ( -7.042111407433782055, -20.27750348750624099, -1.500000000000002220 ) ) ;
#43112 = PLANE ( 'NONE',  #86157 ) ;
#43113 = EDGE_LOOP ( 'NONE', ( #83999, #19252, #62424, #69665 ) ) ;
#43114 = CARTESIAN_POINT ( 'NONE',  ( -12.45680796028966597, 17.00782699154285638, -1.500000000000002220 ) ) ;
#43115 = CARTESIAN_POINT ( 'NONE',  ( -115.6228709571500701, -25.00158670708909625, 2.256160236439165967 ) ) ;
#43116 = DIRECTION ( 'NONE',  ( 0.000000000000000000, 0.000000000000000000, -1.000000000000000000 ) ) ;
#43117 = CARTESIAN_POINT ( 'NONE',  ( -50.62120248232606912, -23.48786465467240347, 11.44779295918255002 ) ) ;
#43118 = DIRECTION ( 'NONE',  ( -0.000000000000000000, 1.000000000000000000, -0.000000000000000000 ) ) ;
#43119 = CARTESIAN_POINT ( 'NONE',  ( -100.5895376238167245, -24.99132157543167310, 2.256160258750668390 ) ) ;
#43120 = CARTESIAN_POINT ( 'NONE',  ( 19.10104996495751450, -11.12853483292915691, -1.500000000000002220 ) ) ;
#43121 = ORIENTED_EDGE ( 'NONE', *, *, #47630, .T. ) ;
#43122 = FACE_OUTER_BOUND ( 'NONE', #65656, .T. ) ;
#43123 = CARTESIAN_POINT ( 'NONE',  ( -3.071531057816138333, -6.376774720514413630, 19.86545874326175110 ) ) ;
#43124 = CARTESIAN_POINT ( 'NONE',  ( -40.49165087243459737, -25.31624741777496013, 5.543942831290165074 ) ) ;
#43125 = VECTOR ( 'NONE', #80966, 1000.000000000000114 ) ;
#43126 = EDGE_CURVE ( 'NONE', #46989, #30992, #97788, .T. ) ;
#43127 = CARTESIAN_POINT ( 'NONE',  ( -62.62365721985609213, -24.66019654487199730, 8.947790411086124607 ) ) ;
#43128 = LINE ( 'NONE', #65990, #33605 ) ;
#43129 = CARTESIAN_POINT ( 'NONE',  ( 5.124585555570928541, 20.71496159572455653, 11.49999999999998934 ) ) ;
#43130 = CARTESIAN_POINT ( 'NONE',  ( -68.94617923632279144, -25.23882047181962918, 6.370111357818270648 ) ) ;
#43131 = CARTESIAN_POINT ( 'NONE',  ( -48.85424939675955613, -25.30060005375480969, 6.009289253917325269 ) ) ;
#43132 = LINE ( 'NONE', #20270, #26018 ) ;
#43133 = CARTESIAN_POINT ( 'NONE',  ( -67.62287095715004170, -24.66019654487199020, 8.947790411086131712 ) ) ;
#43134 = CARTESIAN_POINT ( 'NONE',  ( -6.441999407266626676, 21.70310835763521595, -1.500000000000002220 ) ) ;
#43135 = VECTOR ( 'NONE', #240, 1000.000000000000000 ) ;
#43136 = B_SPLINE_CURVE_WITH_KNOTS ( 'NONE', 3,
 ( #76991, #69897, #1399, #46563, #61799, #47574 ),
 .UNSPECIFIED., .F., .F.,
 ( 4, 2, 4 ),
 ( 0.000000000000000000, 0.001380764517854764966, 0.002761529035709529931 ),
 .UNSPECIFIED. ) ;
#43137 = DIRECTION ( 'NONE',  ( -3.773278334453080206E-23, 0.9999999999976377785, 2.173523156925979975E-06 ) ) ;
#43138 = ORIENTED_EDGE ( 'NONE', *, *, #94359, .T. ) ;
#43139 = AXIS2_PLACEMENT_3D ( 'NONE', #15746, #77634, #8145 ) ;
#43140 = CARTESIAN_POINT ( 'NONE',  ( 8.026968004785691946, 3.316774720514427344, -28.15626605682496830 ) ) ;
#43141 = CARTESIAN_POINT ( 'NONE',  ( 5.271800844963591359, 3.316774720514426456, -28.56638892015329034 ) ) ;
#43142 = CARTESIAN_POINT ( 'NONE',  ( -18.24397684793207830, 7.494555614300850266, 11.49999999999999645 ) ) ;
#43143 = FACE_OUTER_BOUND ( 'NONE', #27245, .T. ) ;
#43144 = EDGE_CURVE ( 'NONE', #71294, #34495, #73466, .T. ) ;
#43145 = AXIS2_PLACEMENT_3D ( 'NONE', #81824, #3714, #66628 ) ;
#43146 = CARTESIAN_POINT ( 'NONE',  ( -73.52287095715006160, -24.50321055353805733, 9.387540953477529371 ) ) ;
#43147 = VERTEX_POINT ( 'NONE', #43520 ) ;
#43148 = CIRCLE ( 'NONE', #82039, 84.48086791635432746 ) ;
#43149 = CARTESIAN_POINT ( 'NONE',  ( -45.52287095715006160, -29.50250243563736774, 8.947779886222146928 ) ) ;
#43150 = CARTESIAN_POINT ( 'NONE',  ( -70.52287095715007581, -24.52323809116983711, 9.355190652339418378 ) ) ;
#43151 = ADVANCED_FACE ( 'NONE', ( #59239 ), #28280, .T. ) ;
#43152 = CARTESIAN_POINT ( 'NONE',  ( -75.52287095715007581, -24.63345952396255356, 9.038047939301504741 ) ) ;
#43153 = CARTESIAN_POINT ( 'NONE',  ( 7.158504886898216846, -20.39052948596947346, 11.49999999999998934 ) ) ;
#43154 = FACE_OUTER_BOUND ( 'NONE', #14092, .T. ) ;
#43156 = CARTESIAN_POINT ( 'NONE',  ( 7.305494252837257285, 17.95555029072639286, -1.500000000000002220 ) ) ;
#43155 = VECTOR ( 'NONE', #86468, 1000.000000000000000 ) ;
#43157 = EDGE_CURVE ( 'NONE', #61766, #75155, #71951, .T. ) ;
#43158 = CARTESIAN_POINT ( 'NONE',  ( -10.35374248095108030, -5.304213687372781649, 27.98611676734227771 ) ) ;
#43159 = PLANE ( 'NONE',  #13398 ) ;
#43160 = CARTESIAN_POINT ( 'NONE',  ( 2.545096341412688812, 19.61957628810408849, -1.500000000000002220 ) ) ;
#43161 = ORIENTED_EDGE ( 'NONE', *, *, #63767, .F. ) ;
#43162 = EDGE_CURVE ( 'NONE', #20729, #86101, #12555, .T. ) ;
#43163 = CARTESIAN_POINT ( 'NONE',  ( 14.61151973098085222, 14.07909450314327771, 11.49999999999999645 ) ) ;
#43164 = DIRECTION ( 'NONE',  ( -0.9890158633619159367, -0.1478094111296165969, 0.000000000000000000 ) ) ;
#43165 = EDGE_CURVE ( 'NONE', #95461, #99483, #27292, .T. ) ;
#43166 = CARTESIAN_POINT ( 'NONE',  ( 6.377880655330028681, -6.376774720514424288, 21.48000012937543346 ) ) ;
#43167 = ORIENTED_EDGE ( 'NONE', *, *, #79311, .F. ) ;
#43168 = LINE ( 'NONE', #19802, #62085 ) ;
#43169 = CARTESIAN_POINT ( 'NONE',  ( 0.02224039135773590858, -0.3828044741864804479, 0.3828044741864790601 ) ) ;
#43170 = DIRECTION ( 'NONE',  ( -3.773278334444166432E-23, 1.000000000000000000, 0.000000000000000000 ) ) ;
#43171 = DIRECTION ( 'NONE',  ( -0.000000000000000000, -1.000000000000000000, -0.000000000000000000 ) ) ;
#43172 = CARTESIAN_POINT ( 'NONE',  ( -31.52287095715006160, -23.47596703998600631, 11.44779298504229459 ) ) ;
#43173 = CARTESIAN_POINT ( 'NONE',  ( 8.743921044546416610, -18.04861246754477477, 11.49999999999998934 ) ) ;
#43174 = EDGE_CURVE ( 'NONE', #93973, #13349, #42532, .T. ) ;
#43175 = CARTESIAN_POINT ( 'NONE',  ( 32.59332756141819232, -1.682774720514426114, -11.41404606144471146 ) ) ;
#43176 = EDGE_LOOP ( 'NONE', ( #4156, #23973, #73406, #96383 ) ) ;
#43177 = CIRCLE ( 'NONE', #13953, 5.000000000000001776 ) ;
#43178 = PLANE ( 'NONE',  #69624 ) ;
#43179 = CARTESIAN_POINT ( 'NONE',  ( -115.5562042904833646, -23.48783264082478794, -1.443836473390058384 ) ) ;
#43180 = DIRECTION ( 'NONE',  ( 1.000000000000000000, 3.773278334444166432E-23, 8.201307841325785021E-29 ) ) ;
#43181 = B_SPLINE_CURVE_WITH_KNOTS ( 'NONE', 3,
 ( #10562, #19663, #2970, #96800 ),
 .UNSPECIFIED., .F., .F.,
 ( 4, 4 ),
 ( 1.387778780781445521E-17, 9.999999999997510880E-05 ),
 .UNSPECIFIED. ) ;
#43182 = LINE ( 'NONE', #57417, #30220 ) ;
#43183 = B_SPLINE_CURVE_WITH_KNOTS ( 'NONE', 3,
 ( #27236, #58191, #67298, #21099, #68288, #74884 ),
 .UNSPECIFIED., .F., .F.,
 ( 4, 2, 4 ),
 ( 6.391158118967745954E-06, 0.001387004593080788098, 0.002767618028042608501 ),
 .UNSPECIFIED. ) ;
#43184 = CARTESIAN_POINT ( 'NONE',  ( -120.6228709571500417, -23.48783264082479505, -1.443836473390058384 ) ) ;
#43185 = CARTESIAN_POINT ( 'NONE',  ( -93.55620429048336462, -24.64898659630528854, 1.056161002820828143 ) ) ;
#43186 = VERTEX_POINT ( 'NONE', #74456 ) ;
#43187 = CARTESIAN_POINT ( 'NONE',  ( 16.70477854660759931, 11.60849435585976153, -1.500000000000002220 ) ) ;
#43188 = ORIENTED_EDGE ( 'NONE', *, *, #59167, .F. ) ;
#43189 = EDGE_CURVE ( 'NONE', #48082, #37098, #26528, .T. ) ;
#43190 = CARTESIAN_POINT ( 'NONE',  ( -22.24355531667433539, 5.575215412481045796, -1.500000000000002220 ) ) ;
#43191 = CARTESIAN_POINT ( 'NONE',  ( 14.76093561896379214, -6.475225279485574248, -26.55548769130089681 ) ) ;
#43192 = ORIENTED_EDGE ( 'NONE', *, *, #32290, .F. ) ;
#43193 = CARTESIAN_POINT ( 'NONE',  ( -111.6228709571500559, -24.64898659630368627, 1.056161002820831474 ) ) ;
#43194 = CIRCLE ( 'NONE', #27034, 84.48086791635432746 ) ;
#43196 = EDGE_CURVE ( 'NONE', #60911, #36333, #50626, .T. ) ;
#43195 = CARTESIAN_POINT ( 'NONE',  ( -76.52287095715006160, -23.72747288104470087, -1.053458166803226348 ) ) ;
#43197 = CARTESIAN_POINT ( 'NONE',  ( -87.58953762381671027, -24.64898659630528854, 1.056161002820826811 ) ) ;
#43198 = CARTESIAN_POINT ( 'NONE',  ( -1.563627757057377110, -21.15500258984412696, 11.49999999999999645 ) ) ;
#43199 = CARTESIAN_POINT ( 'NONE',  ( -14.73459587841175633, -16.56598928932902837, -1.500000000000002220 ) ) ;
#43200 = CARTESIAN_POINT ( 'NONE',  ( 15.34425395324244867, 13.73259486114767114, 11.49999999999998934 ) ) ;
#43201 = AXIS2_PLACEMENT_3D ( 'NONE', #99541, #52901, #77206 ) ;
#43202 = ORIENTED_EDGE ( 'NONE', *, *, #7100, .T. ) ;
#43203 = VERTEX_POINT ( 'NONE', #64886 ) ;
#43204 = LINE ( 'NONE', #66564, #44668 ) ;
#43205 = EDGE_CURVE ( 'NONE', #40372, #56438, #33041, .T. ) ;
#43206 = CARTESIAN_POINT ( 'NONE',  ( -50.52287095715006160, -24.91570333825769978, 8.075032458260348989 ) ) ;
#43207 = ORIENTED_EDGE ( 'NONE', *, *, #92352, .T. ) ;
#43208 = CIRCLE ( 'NONE', #99885, 1.649999999999998579 ) ;
#43209 = ORIENTED_EDGE ( 'NONE', *, *, #78635, .F. ) ;
#43210 = AXIS2_PLACEMENT_3D ( 'NONE', #93983, #18370, #80269 ) ;
#43211 = EDGE_LOOP ( 'NONE', ( #16119, #11242, #77360, #1892 ) ) ;
#43212 = DIRECTION ( 'NONE',  ( 0.9951627101165076983, 0.000000000000000000, 0.09824042138329622254 ) ) ;
#43213 = CARTESIAN_POINT ( 'NONE',  ( -28.53657574427005272, -24.19026137835766121, 9.817618374534074377 ) ) ;
#43214 = CARTESIAN_POINT ( 'NONE',  ( 15.12110981444473623, -4.119741627009104512, -28.36351442485851138 ) ) ;
#43215 = CARTESIAN_POINT ( 'NONE',  ( 3.485566553294195291, 20.44204155273375889, -1.500000000000002220 ) ) ;
#43217 = EDGE_CURVE ( 'NONE', #25435, #32470, #82069, .T. ) ;
#43216 = CARTESIAN_POINT ( 'NONE',  ( 12.24854465327799424, 17.96525243877979605, 11.49999999999999645 ) ) ;
#43218 = ORIENTED_EDGE ( 'NONE', *, *, #11867, .T. ) ;
#43219 = LINE ( 'NONE', #51827, #23979 ) ;
#43220 = CARTESIAN_POINT ( 'NONE',  ( -119.6228709571500559, -23.73934037231757799, 11.05740245334327554 ) ) ;
#43221 = CARTESIAN_POINT ( 'NONE',  ( 21.09243369641204069, 7.689775423913054908, -1.500000000000002220 ) ) ;
#43222 = VECTOR ( 'NONE', #98181, 1000.000000000000114 ) ;
#43223 = DIRECTION ( 'NONE',  ( -1.000000000000000000, 0.000000000000000000, 0.000000000000000000 ) ) ;
#43224 = CARTESIAN_POINT ( 'NONE',  ( 27.86270917940689174, 0.3587747205144265483, 29.49402280011862487 ) ) ;
#43225 = ORIENTED_EDGE ( 'NONE', *, *, #31566, .T. ) ;
#43226 = FACE_OUTER_BOUND ( 'NONE', #39136, .T. ) ;
#43227 = DIRECTION ( 'NONE',  ( 0.000000000000000000, -2.173523156925979552E-06, 0.9999999999976378895 ) ) ;
#43228 = ORIENTED_EDGE ( 'NONE', *, *, #82647, .T. ) ;
#43229 = ORIENTED_EDGE ( 'NONE', *, *, #85675, .T. ) ;
#43230 = DIRECTION ( 'NONE',  ( 1.000000000000000000, 3.491481338843133355E-15, 2.352173255807796056E-16 ) ) ;
#43231 = CC_DESIGN_PERSON_AND_ORGANIZATION_ASSIGNMENT ( #41786, #79819, ( #65234 ) ) ;
#43232 = ORIENTED_EDGE ( 'NONE', *, *, #48669, .F. ) ;
#43233 = CARTESIAN_POINT ( 'NONE',  ( -20.86817740539179056, 4.147639786170328691, -1.500000000000002220 ) ) ;
#43234 = ORIENTED_EDGE ( 'NONE', *, *, #13810, .T. ) ;
#43235 = CARTESIAN_POINT ( 'NONE',  ( -103.6228709571500559, -23.48786465467241769, 11.44779295918254114 ) ) ;
#43236 = CARTESIAN_POINT ( 'NONE',  ( 19.95399986947220583, -8.914707708046476498, -1.500000000000002220 ) ) ;
#43237 = DIRECTION ( 'NONE',  ( -0.000000000000000000, -0.000000000000000000, -1.000000000000000000 ) ) ;
#43238 = CARTESIAN_POINT ( 'NONE',  ( 22.47986593085892437, -3.190245585651162230, -1.500000000000002220 ) ) ;
#43239 = B_SPLINE_CURVE_WITH_KNOTS ( 'NONE', 3,
 ( #20929, #61514, #36173, #75708 ),
 .UNSPECIFIED., .F., .F.,
 ( 4, 4 ),
 ( 0.7603288567031503131, 0.7693352879752661799 ),
 .UNSPECIFIED. ) ;
#43240 = DIRECTION ( 'NONE',  ( 0.000000000000000000, 0.9999999999976377785, 2.173523156925979128E-06 ) ) ;
#43241 = DIRECTION ( 'NONE',  ( 3.773278334444167608E-23, -1.000000000000000000, 0.000000000000000000 ) ) ;
#43242 = CARTESIAN_POINT ( 'NONE',  ( 14.12621959167996977, 16.79361087625908056, -1.500000000000002220 ) ) ;
#43243 = CARTESIAN_POINT ( 'NONE',  ( 6.887358010905132666, -6.376774720514426065, 21.32574817943157086 ) ) ;
#43244 = ORIENTED_EDGE ( 'NONE', *, *, #13657, .F. ) ;
#43245 = CARTESIAN_POINT ( 'NONE',  ( -122.5551195424030340, -24.15620529776629510, 10.23563542870659582 ) ) ;
#43246 = CARTESIAN_POINT ( 'NONE',  ( -127.6228709571500559, -29.50247984919015209, -1.443849546365044922 ) ) ;
#43247 = AXIS2_PLACEMENT_3D ( 'NONE', #12989, #28226, #41975 ) ;
#43248 = ORIENTED_EDGE ( 'NONE', *, *, #41131, .T. ) ;
#43249 = CARTESIAN_POINT ( 'NONE',  ( -30.64751926837171325, -23.47596703998600631, 11.44779298504228038 ) ) ;
#43250 = CARTESIAN_POINT ( 'NONE',  ( 30.53060340732036337, -4.751397487713028944, 17.08790783164733895 ) ) ;
#43251 = VECTOR ( 'NONE', #19517, 1000.000000000000000 ) ;
#43252 = CARTESIAN_POINT ( 'NONE',  ( -30.58080508546457210, -25.30587485921815016, 3.856996771330998719 ) ) ;
#43253 = CARTESIAN_POINT ( 'NONE',  ( 14.70648301983428397, -15.34743991077593250, 11.49999999999998934 ) ) ;
#43254 = CARTESIAN_POINT ( 'NONE',  ( -112.6299549673751272, -23.73766607897671577, -1.055555164236427590 ) ) ;
#43255 = CARTESIAN_POINT ( 'NONE',  ( -26.92257395956520938, -24.97064456621790640, 2.526139883312569889 ) ) ;
#43256 = PLANE ( 'NONE',  #71299 ) ;
#43257 = CARTESIAN_POINT ( 'NONE',  ( -84.62287095715009855, -24.35013146730204525, 9.818937971375111928 ) ) ;
#43258 = CARTESIAN_POINT ( 'NONE',  ( -35.52287095715006870, -29.50250786944525672, 11.44777988621624232 ) ) ;
#43259 = ORIENTED_EDGE ( 'NONE', *, *, #60356, .T. ) ;
#43260 = CARTESIAN_POINT ( 'NONE',  ( 6.425176733589397671, 18.50107501292125178, 11.49999999999999645 ) ) ;
#43261 = CARTESIAN_POINT ( 'NONE',  ( -130.5728709571500588, -23.47593901973090524, -1.443836447538995982 ) ) ;
#43262 = EDGE_CURVE ( 'NONE', #85507, #81379, #79288, .T. ) ;
#43263 = CARTESIAN_POINT ( 'NONE',  ( -8.160000000000000142, -10.15233964170348457, 0.003711184059992174607 ) ) ;
#43264 = ORIENTED_EDGE ( 'NONE', *, *, #92979, .F. ) ;
#43265 = CARTESIAN_POINT ( 'NONE',  ( 4.189750619059152470, -6.376774720514427841, 21.76591699724029283 ) ) ;
#43266 = CARTESIAN_POINT ( 'NONE',  ( -99.29884676835234814, -25.25095974635953056, 6.107783339703508396 ) ) ;
#43267 = AXIS2_PLACEMENT_3D ( 'NONE', #92888, #46733, #47232 ) ;
#43268 = CARTESIAN_POINT ( 'NONE',  ( -62.52287095715006160, -23.48786465467241058, 11.44779295918254824 ) ) ;
#43269 = CARTESIAN_POINT ( 'NONE',  ( 13.91401389203221406, -5.965225279485572685, 158.0376437107427137 ) ) ;
#43270 = CARTESIAN_POINT ( 'NONE',  ( 11.88433821776028942, -15.71472908967258242, 11.49999999999998934 ) ) ;
#43271 = ORIENTED_EDGE ( 'NONE', *, *, #21343, .F. ) ;
#43272 = EDGE_CURVE ( 'NONE', #51886, #63566, #33901, .T. ) ;
#43273 = CARTESIAN_POINT ( 'NONE',  ( 10.73203334292264088, 3.902996417034998000, -26.95265065337511601 ) ) ;
#43274 = FACE_OUTER_BOUND ( 'NONE', #83964, .T. ) ;
#43275 = EDGE_CURVE ( 'NONE', #28558, #55465, #27374, .T. ) ;
#43276 = VECTOR ( 'NONE', #87612, 1000.000000000000114 ) ;
#43277 = PERSON_AND_ORGANIZATION ( #70597, #27821 ) ;
#43278 = ORIENTED_EDGE ( 'NONE', *, *, #31347, .F. ) ;
#43279 = CARTESIAN_POINT ( 'NONE',  ( 8.809764260727238394, -0.02602732333167948400, 3.697389739420775534 ) ) ;
#43280 = CARTESIAN_POINT ( 'NONE',  ( -105.6228709571500417, -24.99156045073393173, 7.747789690856161648 ) ) ;
#43281 = CARTESIAN_POINT ( 'NONE',  ( -69.62287095715005592, -23.47593901973091235, -1.443836447539006196 ) ) ;
#43282 = CARTESIAN_POINT ( 'NONE',  ( 32.76111974776238611, -3.316774720514426900, -3.850861272813261849 ) ) ;
#43283 = CARTESIAN_POINT ( 'NONE',  ( -49.62287095715005592, -24.64965695001467694, 8.947790433994185832 ) ) ;
#43284 = VECTOR ( 'NONE', #33235, 1000.000000000000000 ) ;
#43285 = AXIS2_PLACEMENT_3D ( 'NONE', #59582, #50971, #90513 ) ;
#43286 = CARTESIAN_POINT ( 'NONE',  ( 30.93860345374796594, -6.475225279485573360, 20.86760796525322093 ) ) ;
#43287 = DIRECTION ( 'NONE',  ( -3.773278334453079618E-23, 0.9999999999976377785, 2.173523156925979975E-06 ) ) ;
#43288 = CARTESIAN_POINT ( 'NONE',  ( 16.68016870136555596, 10.92824754362290385, 11.49999999999998934 ) ) ;
#43289 = EDGE_CURVE ( 'NONE', #64548, #64559, #20068, .T. ) ;
#43290 = CARTESIAN_POINT ( 'NONE',  ( 8.071512145086506607, -2.028487854913506805, -5.500000000000000000 ) ) ;
#43291 = CARTESIAN_POINT ( 'NONE',  ( -0.07754179015905204864, -22.04616059090901103, 0.1112944789973146359 ) ) ;
#43292 = ORIENTED_EDGE ( 'NONE', *, *, #48972, .F. ) ;
#43293 = CARTESIAN_POINT ( 'NONE',  ( 7.347880794884120722E-16, 1.826774720514426464, -6.000000000000000888 ) ) ;
#43294 = CARTESIAN_POINT ( 'NONE',  ( 4.628547153713393314, -6.376774720514418959, 20.50654586986123817 ) ) ;
#43295 = CARTESIAN_POINT ( 'NONE',  ( 8.817327481845893544, -6.376774720514593930, -28.08864864928871086 ) ) ;
#43296 = CARTESIAN_POINT ( 'NONE',  ( -45.62287095715004881, -23.47596703998600276, 11.44779298504227505 ) ) ;
#43297 = CARTESIAN_POINT ( 'NONE',  ( -35.92287095715005307, -23.47593901973090169, -1.443836447538997980 ) ) ;
#43298 = CARTESIAN_POINT ( 'NONE',  ( -100.6814946224345562, -25.31603993156367949, 4.890060501307835317 ) ) ;
#43299 = CARTESIAN_POINT ( 'NONE',  ( -51.29010191576745115, -25.25452040107872520, 3.888211261899670035 ) ) ;
#43300 = ORIENTED_EDGE ( 'NONE', *, *, #62784, .T. ) ;
#43301 = CARTESIAN_POINT ( 'NONE',  ( -62.62287095715004881, -23.47593901973091235, -1.443836447539007972 ) ) ;
#43302 = CARTESIAN_POINT ( 'NONE',  ( -52.52287095715006870, -29.50250243563736774, 8.947779886222146928 ) ) ;
#43303 = ORIENTED_EDGE ( 'NONE', *, *, #60832, .F. ) ;
#43304 = CARTESIAN_POINT ( 'NONE',  ( 20.17645099164838030, 1.678240329834772115, -1.500000000000002220 ) ) ;
#43305 = CARTESIAN_POINT ( 'NONE',  ( -70.09747585296138084, -25.31475305677228249, 4.859175633302561970 ) ) ;
#43306 = DIRECTION ( 'NONE',  ( 0.1489078231574191002, 0.000000000000000000, -0.9888510809027407644 ) ) ;
#43307 = VECTOR ( 'NONE', #4173, 1000.000000000000227 ) ;
#43308 = DIRECTION ( 'NONE',  ( 0.000000000000000000, 0.000000000000000000, 1.000000000000000000 ) ) ;
#43309 = ORIENTED_EDGE ( 'NONE', *, *, #55639, .T. ) ;
#43311 = EDGE_CURVE ( 'NONE', #43385, #58528, #81819, .T. ) ;
#43310 = CARTESIAN_POINT ( 'NONE',  ( -46.62287095715006302, -24.33927499327855060, 9.819080762295818943 ) ) ;
#43312 = FACE_OUTER_BOUND ( 'NONE', #23824, .T. ) ;
#43313 = CARTESIAN_POINT ( 'NONE',  ( -18.39468835979788608, -8.022455445098881199, -1.500000000000002220 ) ) ;
#43314 = CARTESIAN_POINT ( 'NONE',  ( 20.92198360912786015, -1.804805560479522342, 11.49999999999999645 ) ) ;
#43315 = AXIS2_PLACEMENT_3D ( 'NONE', #89058, #56624, #40877 ) ;
#43316 = CARTESIAN_POINT ( 'NONE',  ( 30.54440242517687665, -0.2147811518489095850, 23.45430928465147247 ) ) ;
#43317 = CARTESIAN_POINT ( 'NONE',  ( -70.64337588465900808, -24.15602025860896518, 10.28564288303534724 ) ) ;
#43318 = CARTESIAN_POINT ( 'NONE',  ( -19.65368394218270254, -10.04821906498216499, 11.49999999999998934 ) ) ;
#43319 = EDGE_CURVE ( 'NONE', #46585, #13448, #96301, .T. ) ;
#43320 = CARTESIAN_POINT ( 'NONE',  ( -127.6228709571500559, -23.47596703998600631, 11.44779298504227860 ) ) ;
#43321 = EDGE_CURVE ( 'NONE', #37593, #5624, #26789, .T. ) ;
#43322 = CARTESIAN_POINT ( 'NONE',  ( -96.52287095715006160, -24.65952944569304606, 1.056160979905702346 ) ) ;
#43323 = DIRECTION ( 'NONE',  ( 0.000000000000000000, -1.000000000000000000, 0.000000000000000000 ) ) ;
#43324 = EDGE_LOOP ( 'NONE', ( #70599, #54450, #19216, #60420 ) ) ;
#43325 = CARTESIAN_POINT ( 'NONE',  ( -35.52287095715007581, -24.92604778743017135, 8.074972756849357225 ) ) ;
#43326 = CARTESIAN_POINT ( 'NONE',  ( -31.53772339877937370, -24.34968618360933590, 0.1864209137778850556 ) ) ;
#43327 = ORIENTED_EDGE ( 'NONE', *, *, #28030, .T. ) ;
#43328 = ORIENTED_EDGE ( 'NONE', *, *, #29252, .T. ) ;
#43329 = DIRECTION ( 'NONE',  ( -0.000000000000000000, 1.000000000000000000, -0.000000000000000000 ) ) ;
#43330 = DIRECTION ( 'NONE',  ( 0.000000000000000000, -0.9967269304714136968, -0.08084198211964954695 ) ) ;
#43331 = CARTESIAN_POINT ( 'NONE',  ( -89.62287095715007013, -24.34917612406837861, 0.1852690917426663697 ) ) ;
#43332 = CARTESIAN_POINT ( 'NONE',  ( 1.582324178664715975, -20.54890914157308401, -1.500000000000002220 ) ) ;
#43333 = CARTESIAN_POINT ( 'NONE',  ( -5.754811884962036217, -20.78327508566754389, 11.49999999999999645 ) ) ;
#43334 = EDGE_LOOP ( 'NONE', ( #10364, #73522, #41112, #40489 ) ) ;
#43335 = DIRECTION ( 'NONE',  ( 0.000000000000000000, 0.000000000000000000, -1.000000000000000000 ) ) ;
#43336 = CARTESIAN_POINT ( 'NONE',  ( -71.62287095715005592, -29.50247984919015209, -1.443849546365055359 ) ) ;
#43337 = CARTESIAN_POINT ( 'NONE',  ( -97.62287095715005592, -23.48783264082478794, -1.443836473390061936 ) ) ;
#43338 = CARTESIAN_POINT ( 'NONE',  ( -14.53400517605410158, 16.95891092046126403, 11.49999999999998934 ) ) ;
#43339 = AXIS2_PLACEMENT_3D ( 'NONE', #30250, #53114, #45502 ) ;
#43340 = CARTESIAN_POINT ( 'NONE',  ( 32.33408272158504815, -4.458032690740698634, 0.9207958043952065852 ) ) ;
#43341 = CARTESIAN_POINT ( 'NONE',  ( -127.6228709571500559, -24.64898659630368627, 1.056161002820834804 ) ) ;
#43342 = ORIENTED_EDGE ( 'NONE', *, *, #51614, .F. ) ;
#43343 = CARTESIAN_POINT ( 'NONE',  ( -94.52287095715003318, -24.51283580621365488, 0.6167428607019757036 ) ) ;
#43344 = CARTESIAN_POINT ( 'NONE',  ( -89.40841769935767047, -29.50249691823240994, 6.409318347766594037 ) ) ;
#43345 = CARTESIAN_POINT ( 'NONE',  ( -19.94048968823238255, 6.179419890754223488, -1.500000000000002220 ) ) ;
#43346 = ORIENTED_EDGE ( 'NONE', *, *, #36890, .T. ) ;
#43347 = ADVANCED_FACE ( 'NONE', ( #52620 ), #23143, .T. ) ;
#43349 = VERTEX_POINT ( 'NONE', #83049 ) ;
#43348 = CARTESIAN_POINT ( 'NONE',  ( 15.22325621495362391, -3.582999323269832725, -27.23549315679322547 ) ) ;
#43350 = AXIS2_PLACEMENT_3D ( 'NONE', #37831, #53575, #47948 ) ;
#43351 = EDGE_CURVE ( 'NONE', #27247, #95575, #90266, .T. ) ;
#43352 = ORIENTED_EDGE ( 'NONE', *, *, #49113, .F. ) ;
#43353 = FACE_OUTER_BOUND ( 'NONE', #15397, .T. ) ;
#43354 = CARTESIAN_POINT ( 'NONE',  ( 14.88031740681034698, -14.96734982212533183, -1.500000000000002220 ) ) ;
#43355 = VERTEX_POINT ( 'NONE', #75940 ) ;
#43356 = CARTESIAN_POINT ( 'NONE',  ( -28.52287095715006515, -23.56402623438133404, -1.053577192903873527 ) ) ;
#43357 = CARTESIAN_POINT ( 'NONE',  ( -124.6228709571500559, -23.48786465467241769, 11.44779295918253759 ) ) ;
#43358 = CARTESIAN_POINT ( 'NONE',  ( -61.62287095715004881, -23.48786465467240347, 11.44779295918254824 ) ) ;
#43359 = CIRCLE ( 'NONE', #27127, 251.4258649670780699 ) ;
#43360 = CARTESIAN_POINT ( 'NONE',  ( -76.49746590141513991, -24.66019654487199375, 8.947790411086119278 ) ) ;
#43361 = DIRECTION ( 'NONE',  ( 0.000000000000000000, 0.9999999999976377785, 2.173523156925979975E-06 ) ) ;
#43362 = CARTESIAN_POINT ( 'NONE',  ( 0.2638585030419089428, -21.76204025362994798, -1.500000000000002220 ) ) ;
#43363 = CARTESIAN_POINT ( 'NONE',  ( -81.29833273411215089, -25.24759724262089833, 6.730504689138452790 ) ) ;
#43365 = VERTEX_POINT ( 'NONE', #76434 ) ;
#43364 = CARTESIAN_POINT ( 'NONE',  ( 22.08996893241407378, 3.065900275835479860, 11.49999999999999645 ) ) ;
#43366 = CARTESIAN_POINT ( 'NONE',  ( -33.52287095715007581, -23.48783264083359512, -1.443836473376374441 ) ) ;
#43367 = CARTESIAN_POINT ( 'NONE',  ( 15.30881860688521989, 3.493868136757170451, -27.16033061360459300 ) ) ;
#43368 = CARTESIAN_POINT ( 'NONE',  ( -57.62287095715004881, -29.50247984919015209, -1.443849546365056913 ) ) ;
#43369 = ORIENTED_EDGE ( 'NONE', *, *, #93085, .T. ) ;
#43370 = ADVANCED_FACE ( 'NONE', ( #60745 ), #98778, .T. ) ;
#43371 = EDGE_CURVE ( 'NONE', #69024, #37139, #87749, .T. ) ;
#43373 = EDGE_LOOP ( 'NONE', ( #62956, #90823, #37268, #16820 ) ) ;
#43372 = CARTESIAN_POINT ( 'NONE',  ( -54.52287095715005449, -23.47593901973090169, -1.443836447538997092 ) ) ;
#43374 = ORIENTED_EDGE ( 'NONE', *, *, #37292, .F. ) ;
#43375 = B_SPLINE_CURVE_WITH_KNOTS ( 'NONE', 3,
 ( #69342, #45022, #98780, #21160 ),
 .UNSPECIFIED., .F., .F.,
 ( 4, 4 ),
 ( 0.000000000000000000, 1.000000000000000000 ),
 .UNSPECIFIED. ) ;
#43376 = CARTESIAN_POINT ( 'NONE',  ( -30.64427850938830389, -23.56000036390796737, -1.497999999999532594 ) ) ;
#43377 = DIRECTION ( 'NONE',  ( 1.000000000000000000, 1.387778780781445429E-16, 0.000000000000000000 ) ) ;
#43378 = DIRECTION ( 'NONE',  ( -0.000000000000000000, 0.000000000000000000, -1.000000000000000000 ) ) ;
#43379 = CARTESIAN_POINT ( 'NONE',  ( 31.52236416363829363, 4.132774720514426292, -3.023391441407382807 ) ) ;
#43380 = CARTESIAN_POINT ( 'NONE',  ( -51.04357394935764347, -25.31543073408252553, 4.940877929217665887 ) ) ;
#43381 = ORIENTED_EDGE ( 'NONE', *, *, #60048, .T. ) ;
#43382 = CARTESIAN_POINT ( 'NONE',  ( -11.15089393765527959, -15.82809448842462885, 11.49999999999999645 ) ) ;
#43383 = DIRECTION ( 'NONE',  ( -0.000000000000000000, 0.000000000000000000, -1.000000000000000000 ) ) ;
#43384 = ADVANCED_FACE ( 'NONE', ( #37893 ), #68348, .T. ) ;
#43385 = VERTEX_POINT ( 'NONE', #21158 ) ;
#43386 = CARTESIAN_POINT ( 'NONE',  ( 2.968164339864655332, -5.876774720514408301, 19.33154224050496595 ) ) ;
#43387 = CARTESIAN_POINT ( 'NONE',  ( 2.589743589743596086, -5.876774720514416295, 20.00140224358974095 ) ) ;
#43388 = CARTESIAN_POINT ( 'NONE',  ( -30.47287095715007510, -23.47596703474403768, 11.44538124590455830 ) ) ;
#43389 = CARTESIAN_POINT ( 'NONE',  ( 26.73860345374794534, -5.356774720514427379, -3.111611894936215705 ) ) ;
#43390 = CARTESIAN_POINT ( 'NONE',  ( -11.77723790057865116, -15.68276428244051779, -1.500000000000002220 ) ) ;
#43391 = B_SPLINE_SURFACE_WITH_KNOTS ( 'NONE', 3, 3, ( 
 ( #92994, #46333, #77758, #55457 ),
 ( #15370, #32608, #47340, #55962 ),
 ( #157, #39713, #70672, #23470 ),
 ( #94000, #63583, #1669, #94506 ),
 ( #46840, #8272, #32101, #62070 ),
 ( #24987, #54451, #16374, #9770 ),
 ( #33111, #31602, #63075, #86891 ),
 ( #17384, #85385, #77264, #48346 ),
 ( #86395, #24489, #79276, #95006 ),
 ( #85894, #16878, #47841, #40724 ) ),
 .UNSPECIFIED., .F., .F., .F.,
 ( 4, 3, 3, 4 ),
 ( 4, 4 ),
 ( 0.0004766839783815776210, 0.1491231665100171133, 0.2234464077758348821, 0.2977696490416526509 ),
 ( 0.7995905709435781050, 0.8010797674005437630 ),
 .UNSPECIFIED. ) ;
#43392 = DIRECTION ( 'NONE',  ( -0.000000000000000000, -1.000000000000000000, 0.000000000000000000 ) ) ;
#43393 = ORIENTED_EDGE ( 'NONE', *, *, #45034, .T. ) ;
#43394 = CARTESIAN_POINT ( 'NONE',  ( -18.53595284743415661, 10.95218985133829825, 11.49999999999998934 ) ) ;
#43395 = CARTESIAN_POINT ( 'NONE',  ( -89.40841769935764205, -25.12049752546738191, 2.832404795212221327 ) ) ;
#43396 = CARTESIAN_POINT ( 'NONE',  ( -80.46709582760330193, -25.30394759373683655, 4.967766255445141610 ) ) ;
#43397 = FACE_OUTER_BOUND ( 'NONE', #74217, .T. ) ;
#43398 = CARTESIAN_POINT ( 'NONE',  ( -99.52924129105133488, -25.27473359744577408, 3.929520238420538103 ) ) ;
#43399 = CARTESIAN_POINT ( 'NONE',  ( -8.204236019480731557, -21.45505762417899831, -1.500000000000002220 ) ) ;
#43400 = EDGE_CURVE ( 'NONE', #11305, #47218, #6685, .T. ) ;
#43401 = ADVANCED_FACE ( 'NONE', ( #84060 ), #67857, .F. ) ;
#43402 = PERSON_AND_ORGANIZATION ( #70597, #27821 ) ;
#43403 = DIRECTION ( 'NONE',  ( 0.000000000000000000, 0.000000000000000000, 1.000000000000000000 ) ) ;
#43404 = CARTESIAN_POINT ( 'NONE',  ( -53.48693110046856702, -24.65952944569304250, 1.056160979905695463 ) ) ;
#43405 = CARTESIAN_POINT ( 'NONE',  ( -18.82377384687745447, 7.257840063761761051, 11.49999999999999645 ) ) ;
#43406 = LINE ( 'NONE', #98161, #88398 ) ;
#43407 = CARTESIAN_POINT ( 'NONE',  ( -51.62287095715005592, -24.64965695001468404, 8.947790433994185832 ) ) ;
#43408 = PRODUCT_DEFINITION_SHAPE ( 'NONE', 'NONE',  #100430 ) ;
#43409 = DIRECTION ( 'NONE',  ( -3.773278334453079618E-23, 0.9999999999976377785, 2.173523156925979975E-06 ) ) ;
#43410 = LINE ( 'NONE', #19552, #74796 ) ;
#43411 = CARTESIAN_POINT ( 'NONE',  ( -30.57287095715004099, -23.47593903913510260, -1.434903445928520149 ) ) ;
#43412 = CARTESIAN_POINT ( 'NONE',  ( -19.08307359429613825, -5.530936995296134917, -1.500000000000002220 ) ) ;
#43413 = EDGE_CURVE ( 'NONE', #54573, #44858, #14545, .T. ) ;
#43414 = DIRECTION ( 'NONE',  ( 0.000000000000000000, 0.000000000000000000, 1.000000000000000000 ) ) ;
#43415 = CARTESIAN_POINT ( 'NONE',  ( 19.63295818312489871, -1.572306604260808260, -1.500000000000002220 ) ) ;
#43416 = CIRCLE ( 'NONE', #75835, 3.060000000000000053 ) ;
#43417 = CARTESIAN_POINT ( 'NONE',  ( 30.53060340732035982, 1.477225279485574028, -1.272392034746785860 ) ) ;
#43418 = EDGE_CURVE ( 'NONE', #100230, #99338, #14039, .T. ) ;
#43419 = B_SPLINE_CURVE_WITH_KNOTS ( 'NONE', 3,
 ( #58500, #89434, #12292, #74211 ),
 .UNSPECIFIED., .F., .F.,
 ( 4, 4 ),
 ( 0.000000000000000000, 9.999999999998897304E-05 ),
 .UNSPECIFIED. ) ;
#43420 = LINE ( 'NONE', #74352, #98565 ) ;
#43421 = DIRECTION ( 'NONE',  ( -0.000000000000000000, 1.000000000000000000, -0.000000000000000000 ) ) ;
#43422 = CARTESIAN_POINT ( 'NONE',  ( -20.60850594246137035, -0.7621957659720622891, 11.49999999999999645 ) ) ;
#43423 = CARTESIAN_POINT ( 'NONE',  ( -48.62287095715004881, -23.47596703998600276, 11.44779298504227505 ) ) ;
#43424 = VECTOR ( 'NONE', #51321, 1000.000000000000114 ) ;
#43425 = DIRECTION ( 'NONE',  ( -0.000000000000000000, -1.000000000000000000, -0.000000000000000000 ) ) ;
#43426 = CARTESIAN_POINT ( 'NONE',  ( -9.675873947287982446, 20.46574270456686406, 11.49999999999999645 ) ) ;
#43427 = ORIENTED_EDGE ( 'NONE', *, *, #67457, .T. ) ;
#43428 = DIRECTION ( 'NONE',  ( 1.000000000000000000, 0.000000000000000000, 0.000000000000000000 ) ) ;
#43429 = CARTESIAN_POINT ( 'NONE',  ( 30.60111574538730039, 4.387371784078713866, 26.76015704162893627 ) ) ;
#43430 = VECTOR ( 'NONE', #39510, 1000.000000000000114 ) ;
#43431 = B_SPLINE_CURVE_WITH_KNOTS ( 'NONE', 3,
 ( #92014, #13886, #92508, #61588 ),
 .UNSPECIFIED., .F., .F.,
 ( 4, 4 ),
 ( 0.000000000000000000, 9.999999999998897304E-05 ),
 .UNSPECIFIED. ) ;
#43432 = CARTESIAN_POINT ( 'NONE',  ( -63.62745468079150868, -24.51314013834316796, 0.6176544820404160641 ) ) ;
#43433 = DIRECTION ( 'NONE',  ( 0.000000000000000000, -0.9999999999976377785, -2.173523156925979128E-06 ) ) ;
#43434 = ORIENTED_EDGE ( 'NONE', *, *, #16675, .F. ) ;
#43435 = ORIENTED_EDGE ( 'NONE', *, *, #96283, .T. ) ;
#43436 = EDGE_CURVE ( 'NONE', #29097, #10925, #68845, .T. ) ;
#43437 = CARTESIAN_POINT ( 'NONE',  ( -99.42972581403923016, -25.19882830581870792, 6.611274056847894265 ) ) ;
#43438 = CARTESIAN_POINT ( 'NONE',  ( 22.22072617242880455, -5.352622178732230118, -1.500000000000002220 ) ) ;
#43439 = CARTESIAN_POINT ( 'NONE',  ( -74.62287095715007013, -24.34917612406838217, 0.1852690917426618733 ) ) ;
#43440 = CARTESIAN_POINT ( 'NONE',  ( -4.019545577234938882, 21.20919285897865336, -1.500000000000002220 ) ) ;
#43441 = AXIS2_PLACEMENT_3D ( 'NONE', #29161, #53016, #4835 ) ;
#43442 = DIRECTION ( 'NONE',  ( 0.06975647374412546897, 0.9975640502598241977, 0.000000000000000000 ) ) ;
#43443 = DIRECTION ( 'NONE',  ( -0.8246584009594636333, 0.000000000000000000, -0.5656310827093756766 ) ) ;
#43444 = CARTESIAN_POINT ( 'NONE',  ( 15.50834587592193259, -16.38432980155966590, 11.49999999999999645 ) ) ;
#43445 = VERTEX_POINT ( 'NONE', #85056 ) ;
#43446 = CARTESIAN_POINT ( 'NONE',  ( -70.13845683480205651, -25.24754246629652599, 4.855284388605379142 ) ) ;
#43447 = CARTESIAN_POINT ( 'NONE',  ( 21.30657626330824783, 5.479626006175059239, -1.500000000000002220 ) ) ;
#43448 = PLANE ( 'NONE',  #73838 ) ;
#43449 = CARTESIAN_POINT ( 'NONE',  ( -128.6228709571500417, -29.50250786944525672, 11.44777988621622633 ) ) ;
#43450 = VERTEX_POINT ( 'NONE', #60249 ) ;
#43451 = CARTESIAN_POINT ( 'NONE',  ( 5.109298100548420152, 3.316774720514426456, -27.55941679637948383 ) ) ;
#43452 = DIRECTION ( 'NONE',  ( -0.000000000000000000, -1.000000000000000000, -0.000000000000000000 ) ) ;
#43453 = ORIENTED_EDGE ( 'NONE', *, *, #2463, .F. ) ;
#43454 = CARTESIAN_POINT ( 'NONE',  ( -53.52287095715006870, -29.50248528299804818, 1.056150453629033370 ) ) ;
#43455 = EDGE_LOOP ( 'NONE', ( #51137, #52445, #66446, #78687 ) ) ;
#43456 = ORIENTED_EDGE ( 'NONE', *, *, #85089, .T. ) ;
#43457 = CARTESIAN_POINT ( 'NONE',  ( -65.52287095715006160, -24.99132157543083821, 2.256160258750667502 ) ) ;
#43458 = FACE_OUTER_BOUND ( 'NONE', #79748, .T. ) ;
#43459 = LINE ( 'NONE', #60683, #8197 ) ;
#43460 = CARTESIAN_POINT ( 'NONE',  ( -20.22731604866883970, -2.807383831903240257, -1.500000000000002220 ) ) ;
#43461 = ORIENTED_EDGE ( 'NONE', *, *, #9373, .F. ) ;
#43462 = CARTESIAN_POINT ( 'NONE',  ( -70.34543693012690824, -25.03284467579916495, 7.563174216508125269 ) ) ;
#43463 = CARTESIAN_POINT ( 'NONE',  ( -30.64427850938830389, -23.56000036390796737, -1.497999999999532594 ) ) ;
#43464 = CARTESIAN_POINT ( 'NONE',  ( -105.6347239592964087, -23.85016227208580730, -0.8807180028928328630 ) ) ;
#43465 = CARTESIAN_POINT ( 'NONE',  ( -71.70841769935766763, -25.25855084132322048, 6.192981418235004476 ) ) ;
#43466 = ORIENTED_EDGE ( 'NONE', *, *, #19174, .T. ) ;
#43467 = DIRECTION ( 'NONE',  ( 0.000000000000000000, 0.9999999999976377785, 2.173523156925979128E-06 ) ) ;
#43468 = CARTESIAN_POINT ( 'NONE',  ( -27.85310238079214784, -24.63646064164220206, 8.249332086164569589 ) ) ;
#43469 = ORIENTED_EDGE ( 'NONE', *, *, #69873, .T. ) ;
#43470 = CARTESIAN_POINT ( 'NONE',  ( 10.19739565540945492, -18.13666118385682680, -1.500000000000002220 ) ) ;
#43471 = VERTEX_POINT ( 'NONE', #52126 ) ;
#43473 = ORIENTED_EDGE ( 'NONE', *, *, #10457, .T. ) ;
#43472 = CARTESIAN_POINT ( 'NONE',  ( -39.99567047530755559, -25.30560115809254285, 5.008336357703472075 ) ) ;
#43474 = EDGE_CURVE ( 'NONE', #49798, #61594, #98694, .T. ) ;
#43475 = B_SPLINE_SURFACE_WITH_KNOTS ( 'NONE', 3, 3, ( 
 ( #16694, #54778, #23805, #979 ),
 ( #77085, #16193, #47161, #78081 ),
 ( #8592, #84203, #47663, #39541 ),
 ( #100410, #31931, #7586, #40040 ),
 ( #62900, #14693, #30921, #7086 ),
 ( #93823, #78579, #61891, #9086 ),
 ( #68987, #69494, #92814, #60889 ),
 ( #91817, #99910, #53777, #92318 ),
 ( #30422, #23295, #22789, #15195 ),
 ( #54281, #85207, #15697, #88225 ) ),
 .UNSPECIFIED., .F., .F., .F.,
 ( 4, 3, 3, 4 ),
 ( 4, 4 ),
 ( 0.7022005934544804928, 0.7765311282028795059, 0.8508616629512786300, 0.9995227324480767672 ),
 ( 0.8996025664823215084, 0.9011514415367618547 ),
 .UNSPECIFIED. ) ;
#43476 = CARTESIAN_POINT ( 'NONE',  ( -51.52764846858840997, -25.25854370750454336, 6.187572764404343673 ) ) ;
#43477 = CARTESIAN_POINT ( 'NONE',  ( -115.5228709571500190, -24.82558206586144678, 1.605769216559448598 ) ) ;
#43478 = VERTEX_POINT ( 'NONE', #59745 ) ;
#43479 = ORIENTED_EDGE ( 'NONE', *, *, #94951, .T. ) ;
#43480 = CARTESIAN_POINT ( 'NONE',  ( -114.6228709571500701, -24.51283580621365132, 0.6167428607019879161 ) ) ;
#43481 = CARTESIAN_POINT ( 'NONE',  ( -76.52287095715007581, -23.47596703998600631, 11.44779298504228571 ) ) ;
#43482 = DIRECTION ( 'NONE',  ( -0.000000000000000000, 2.173523156925979552E-06, -0.9999999999976378895 ) ) ;
#43483 = CARTESIAN_POINT ( 'NONE',  ( -70.35895856474229504, -25.31201590484430142, 5.313173609717680712 ) ) ;
#43485 = VERTEX_POINT ( 'NONE', #6444 ) ;
#43484 = CARTESIAN_POINT ( 'NONE',  ( -14.46940225681120396, -16.66540133702554272, 11.49999999999999645 ) ) ;
#43486 = CARTESIAN_POINT ( 'NONE',  ( -108.6235312761321552, -24.65952944569305316, 1.056160979905706121 ) ) ;
#43487 = CARTESIAN_POINT ( 'NONE',  ( 1.383477600506065164, -22.57338898373578218, 11.49999999999998934 ) ) ;
#43488 = EDGE_CURVE ( 'NONE', #83993, #87855, #16635, .T. ) ;
#43489 = EDGE_CURVE ( 'NONE', #92742, #41074, #84558, .T. ) ;
#43490 = VECTOR ( 'NONE', #54513, 1000.000000000000227 ) ;
#43491 = EDGE_CURVE ( 'NONE', #56620, #94842, #84142, .T. ) ;
#43493 = ORIENTED_EDGE ( 'NONE', *, *, #48774, .T. ) ;
#43492 = CARTESIAN_POINT ( 'NONE',  ( -57.52287095715003318, -24.66019654487198665, 8.947790411086121054 ) ) ;
#43494 = ORIENTED_EDGE ( 'NONE', *, *, #41905, .F. ) ;
#43495 = EDGE_CURVE ( 'NONE', #90831, #73894, #17663, .T. ) ;
#43496 = LINE ( 'NONE', #90648, #70984 ) ;
#43497 = CARTESIAN_POINT ( 'NONE',  ( -57.50306194990486119, -24.15620529776628089, 10.23563542870660470 ) ) ;
#43498 = EDGE_LOOP ( 'NONE', ( #78880, #84276, #89040, #70296 ) ) ;
#43499 = VECTOR ( 'NONE', #36657, 1000.000000000000114 ) ;
#43500 = CARTESIAN_POINT ( 'NONE',  ( -40.49165087243459737, -25.30507958278164793, 5.543942855563713579 ) ) ;
#43501 = CARTESIAN_POINT ( 'NONE',  ( -10.38793682863964563, 19.71736701935523683, -1.500000000000002220 ) ) ;
#43502 = PLANE ( 'NONE',  #21066 ) ;
#43503 = EDGE_CURVE ( 'NONE', #89617, #84065, #43011, .T. ) ;
#43504 = EDGE_LOOP ( 'NONE', ( #391, #30851, #48845, #52083 ) ) ;
#43505 = LINE ( 'NONE', #29258, #7615 ) ;
#43506 = DIRECTION ( 'NONE',  ( -3.773278334453079618E-23, 0.9999999999976377785, 2.173523156925979975E-06 ) ) ;
#43507 = CARTESIAN_POINT ( 'NONE',  ( -108.6228709571500417, -24.65952944569305316, 1.056160979905705011 ) ) ;
#43508 = CARTESIAN_POINT ( 'NONE',  ( -29.49875734969026198, -5.965225279485572685, 0.1180228001186258285 ) ) ;
#43509 = EDGE_CURVE ( 'NONE', #14950, #83990, #86564, .T. ) ;
#43511 = CIRCLE ( 'NONE', #6188, 84.48086791635432746 ) ;
#43510 = CARTESIAN_POINT ( 'NONE',  ( -14.81708852449743929, -12.69844354874750181, -1.500000000000002220 ) ) ;
#43512 = CARTESIAN_POINT ( 'NONE',  ( 0.5228555243449846124, 21.43159495547403282, 11.49999999999998934 ) ) ;
#43513 = CARTESIAN_POINT ( 'NONE',  ( -1.292025413547811308, -6.376774720514413630, 19.72913074730690752 ) ) ;
#43514 = CARTESIAN_POINT ( 'NONE',  ( -107.5562042904834072, -23.48786465467241769, 11.44779295918253936 ) ) ;
#43515 = FACE_OUTER_BOUND ( 'NONE', #54417, .T. ) ;
#43516 = CARTESIAN_POINT ( 'NONE',  ( 9.298244000614250382, 20.81247324795305431, -1.500000000000002220 ) ) ;
#43517 = ADVANCED_FACE ( 'NONE', ( #46505 ), #17554, .T. ) ;
#43518 = APPLICATION_PROTOCOL_DEFINITION ( 'international standard', 'config_control_design', 1994, #25210 ) ;
#43519 = DIRECTION ( 'NONE',  ( 0.000000000000000000, -2.173523156925980399E-06, 0.9999999999976378895 ) ) ;
#43520 = CARTESIAN_POINT ( 'NONE',  ( -29.49875734969025842, -0.3587747205144262708, 15.62202280011862321 ) ) ;
#43521 = CARTESIAN_POINT ( 'NONE',  ( -8.876215969300202957, 17.89991547088461488, 11.49999999999999645 ) ) ;
#43522 = CARTESIAN_POINT ( 'NONE',  ( -54.62287095715005592, -29.50247984919015209, -1.443849546365058689 ) ) ;
#43523 = CARTESIAN_POINT ( 'NONE',  ( -91.62287095715004170, -24.66019654487199730, 8.947790411086124607 ) ) ;
#43524 = CARTESIAN_POINT ( 'NONE',  ( -128.6228709571500417, -24.66019654487200441, 8.947790411086121054 ) ) ;
#43525 = ORIENTED_EDGE ( 'NONE', *, *, #58977, .T. ) ;
#43526 = CARTESIAN_POINT ( 'NONE',  ( -25.85421410313377066, -24.77680504942480866, 2.948317657866410535 ) ) ;
#43527 = CARTESIAN_POINT ( 'NONE',  ( 10.54812756816019892, -3.634129942730893070, -27.00766266717979747 ) ) ;
#43528 = EDGE_CURVE ( 'NONE', #18101, #84750, #39402, .T. ) ;
#43529 = CARTESIAN_POINT ( 'NONE',  ( 5.343276940429747768, -21.04383479052346217, 11.49999999999998934 ) ) ;
#43530 = DIRECTION ( 'NONE',  ( -3.773278334453080206E-23, 0.9999999999976377785, 2.173523156925979975E-06 ) ) ;
#43531 = CARTESIAN_POINT ( 'NONE',  ( -11.52932745282126703, -15.74164922852205173, -1.500000000000002220 ) ) ;
#43532 = DIRECTION ( 'NONE',  ( 0.000000000000000000, 0.000000000000000000, -1.000000000000000000 ) ) ;
#43533 = ADVANCED_FACE ( 'NONE', ( #94169 ), #99401, .T. ) ;
#43534 = ORIENTED_EDGE ( 'NONE', *, *, #25845, .T. ) ;
#43535 = SECURITY_CLASSIFICATION_LEVEL ( 'unclassified' ) ;
#43536 = CARTESIAN_POINT ( 'NONE',  ( 13.74975846015576586, -5.965225279485572685, -27.72022515045486557 ) ) ;
#43537 = CARTESIAN_POINT ( 'NONE',  ( -20.16212974941129588, 3.559051167911782887, 11.49999999999999645 ) ) ;
#43538 = CARTESIAN_POINT ( 'NONE',  ( 15.99960863614631101, 3.577630190450212577, -27.91116951066581819 ) ) ;
#43539 = CARTESIAN_POINT ( 'NONE',  ( -39.62287095715007723, -23.95044443724991012, 10.65354141964650125 ) ) ;
#43540 = EDGE_LOOP ( 'NONE', ( #34079, #47567 ) ) ;
#43541 = CARTESIAN_POINT ( 'NONE',  ( 8.063330319165388005, -10.15233964170352898, 1.310587897985993955 ) ) ;
#43542 = CARTESIAN_POINT ( 'NONE',  ( -106.6228709571500275, -23.72773821059536559, 11.05748984161097681 ) ) ;
#43543 = CARTESIAN_POINT ( 'NONE',  ( -78.62287095715005592, -24.33832256526968862, 0.1851278514119878704 ) ) ;
#43544 = B_SPLINE_CURVE_WITH_KNOTS ( 'NONE', 3,
 ( #68075, #5171, #5666, #29000, #68572, #45239 ),
 .UNSPECIFIED., .F., .F.,
 ( 4, 2, 4 ),
 ( 1.570755371634111329E-05, 0.001396183895866089271, 0.002776660238015837747 ),
 .UNSPECIFIED. ) ;
#43545 = CARTESIAN_POINT ( 'NONE',  ( -127.5228709571500616, -29.50250243563736774, 8.947779886222132717 ) ) ;
#43546 = ORIENTED_EDGE ( 'NONE', *, *, #84278, .F. ) ;
#43547 = DIRECTION ( 'NONE',  ( -3.773278334453079030E-23, 0.9999999999976377785, 2.173523156925979128E-06 ) ) ;
#43548 = CIRCLE ( 'NONE', #24043, 20.00000000000000000 ) ;
#43549 = CARTESIAN_POINT ( 'NONE',  ( -22.90524134523018773, 2.401388714834002069, 11.49999999999999645 ) ) ;
#43550 = CARTESIAN_POINT ( 'NONE',  ( 6.015242202445381992, 21.98585358372262633, -1.500000000000002220 ) ) ;
#43551 = CARTESIAN_POINT ( 'NONE',  ( -70.27422298781921484, -25.31517373419701755, 4.851635141314512900 ) ) ;
#43552 = DIRECTION ( 'NONE',  ( 0.000000000000000000, 0.9999999999976377785, 2.173523156925979975E-06 ) ) ;
#43553 = DIRECTION ( 'NONE',  ( -0.000000000000000000, 1.000000000000000000, 1.084202172485504434E-16 ) ) ;
#43554 = AXIS2_PLACEMENT_3D ( 'NONE', #75705, #14307, #60517 ) ;
#43555 = CARTESIAN_POINT ( 'NONE',  ( -124.6228709571500559, -23.47593901973091235, -1.443836447538997536 ) ) ;
#43556 = CARTESIAN_POINT ( 'NONE',  ( -110.5904913666769005, -24.40034930558991633, 0.3402023900116072364 ) ) ;
#43557 = CARTESIAN_POINT ( 'NONE',  ( -5.132426408838210108, -21.30661980433056968, 11.49999999999998934 ) ) ;
#43558 = LINE ( 'NONE', #12091, #38113 ) ;
#43559 = CARTESIAN_POINT ( 'NONE',  ( -103.5228709571500474, -24.66019654487200441, 8.947790411086119278 ) ) ;
#43560 = CARTESIAN_POINT ( 'NONE',  ( -120.6228709571500417, -23.47593901973091235, -1.443836447538997536 ) ) ;
#43561 = CARTESIAN_POINT ( 'NONE',  ( 30.61643171304413613, 6.475225279485573360, 27.37433008668288181 ) ) ;
#43562 = VERTEX_POINT ( 'NONE', #72854 ) ;
#43563 = VECTOR ( 'NONE', #91201, 1000.000000000000114 ) ;
#43564 = CARTESIAN_POINT ( 'NONE',  ( 10.07161678670223637, 17.78519941539584792, -1.500000000000002220 ) ) ;
#43565 = ORIENTED_EDGE ( 'NONE', *, *, #35868, .T. ) ;
#43566 = ORIENTED_EDGE ( 'NONE', *, *, #63910, .F. ) ;
#43567 = ORIENTED_EDGE ( 'NONE', *, *, #67550, .F. ) ;
#43568 = ORIENTED_EDGE ( 'NONE', *, *, #97272, .T. ) ;
#43569 = CARTESIAN_POINT ( 'NONE',  ( -3.733506833432379768, 22.73668382284982314, 11.49999999999998934 ) ) ;
#43570 = DIRECTION ( 'NONE',  ( -3.773278334453079618E-23, 0.9999999999976377785, 2.173523156925979975E-06 ) ) ;
#43571 = CARTESIAN_POINT ( 'NONE',  ( 19.26017855675105750, 6.235128648364509196, -1.500000000000002220 ) ) ;
#43572 = VERTEX_POINT ( 'NONE', #27674 ) ;
#43573 = CARTESIAN_POINT ( 'NONE',  ( -69.58953762381672448, -23.47596703998600276, 11.44779298504227505 ) ) ;
#43574 = CARTESIAN_POINT ( 'NONE',  ( -48.52287095715006160, -23.48786465467241769, 11.44779295918255002 ) ) ;
#43575 = CARTESIAN_POINT ( 'NONE',  ( -51.62287095715008434, -23.95044443724992433, 10.65354141964650125 ) ) ;
#43576 = DIRECTION ( 'NONE',  ( 0.000000000000000000, -2.173523156925980399E-06, 0.9999999999976378895 ) ) ;
#43578 = ORIENTED_EDGE ( 'NONE', *, *, #8987, .T. ) ;
#43577 = CARTESIAN_POINT ( 'NONE',  ( 3.659817510876246960, 21.07357064420920878, 11.49999999999999645 ) ) ;
#43579 = CARTESIAN_POINT ( 'NONE',  ( -55.52287095715006160, -24.62226745350438861, 0.9660975649728085202 ) ) ;
#43580 = ORIENTED_EDGE ( 'NONE', *, *, #92413, .T. ) ;
#43581 = CARTESIAN_POINT ( 'NONE',  ( 20.56042274393015035, -8.519965759701490171, 11.49999999999998934 ) ) ;
#43582 = CARTESIAN_POINT ( 'NONE',  ( -19.40337959798338119, 7.141409694766009508, -1.500000000000002220 ) ) ;
#43584 = EDGE_LOOP ( 'NONE', ( #86987, #47685, #76147, #36190 ) ) ;
#43583 = CLOSED_SHELL ( 'NONE', ( #78306, #95076, #59944, #38654, #34047, #75319, #23448, #37294, #14268, #93958, #67830, #13326, #20263, #14273, #11832, #75509, #30113, #2042, #64988, #64703, #25479, #89774 ) ) ;
#43585 = LINE ( 'NONE', #49214, #51803 ) ;
#43586 = ORIENTED_EDGE ( 'NONE', *, *, #88387, .T. ) ;
#43587 = EDGE_CURVE ( 'NONE', #1165, #51313, #28016, .T. ) ;
#43588 = CARTESIAN_POINT ( 'NONE',  ( -129.5228709571500758, -24.64898659630529920, 1.056161002820834804 ) ) ;
#43589 = VERTEX_POINT ( 'NONE', #80957 ) ;
#43590 = ADVANCED_FACE ( 'NONE', ( #4832 ), #89071, .T. ) ;
#43591 = CARTESIAN_POINT ( 'NONE',  ( 13.96602909953038640, 15.60522523583095200, -1.500000000000002220 ) ) ;
#43592 = CARTESIAN_POINT ( 'NONE',  ( -12.46176837856299002, 18.05058065364367792, 11.49999999999999645 ) ) ;
#43593 = EDGE_CURVE ( 'NONE', #30864, #96155, #26351, .T. ) ;
#43594 = LINE ( 'NONE', #28356, #4235 ) ;
#43595 = CARTESIAN_POINT ( 'NONE',  ( -20.59131556071872282, -9.131246169528550283, -1.500000000000002220 ) ) ;
#43596 = ADVANCED_FACE ( 'NONE', ( #50022 ), #73351, .T. ) ;
#43597 = CARTESIAN_POINT ( 'NONE',  ( -7.049398010371669798, 19.71092172866906012, -1.500000000000002220 ) ) ;
#43598 = PLANE ( 'NONE',  #2650 ) ;
#43599 = ADVANCED_FACE ( 'NONE', ( #88575 ), #87568, .F. ) ;
#43600 = CARTESIAN_POINT ( 'NONE',  ( -29.62287095715006302, -23.88397930277545456, 10.65359469698177541 ) ) ;
#43601 = CARTESIAN_POINT ( 'NONE',  ( 15.63605935613269438, -5.965225279485572685, -27.55169773172585934 ) ) ;
#43602 = VERTEX_POINT ( 'NONE', #19547 ) ;
#43603 = EDGE_LOOP ( 'NONE', ( #72433, #69247, #22701, #3276 ) ) ;
#43604 = ORIENTED_EDGE ( 'NONE', *, *, #11312, .T. ) ;
#43605 = CARTESIAN_POINT ( 'NONE',  ( -66.53647785511840596, -24.65952944569304250, 1.056160979905692798 ) ) ;
#43606 = CARTESIAN_POINT ( 'NONE',  ( -19.99255411920323056, 7.849732829375159149, -1.500000000000002220 ) ) ;
#43607 = B_SPLINE_CURVE_WITH_KNOTS ( 'NONE', 3,
 ( #64771, #19053, #79452, #87573, #88081, #71858 ),
 .UNSPECIFIED., .F., .F.,
 ( 4, 2, 4 ),
 ( 6.384118696740187843E-06, 0.001386860460837440866, 0.002767336802978141459 ),
 .UNSPECIFIED. ) ;
#43608 = CARTESIAN_POINT ( 'NONE',  ( -113.6228709571500559, -29.50250243563736774, 8.947779886222136270 ) ) ;
#43609 = ORIENTED_EDGE ( 'NONE', *, *, #89330, .T. ) ;
#43610 = CARTESIAN_POINT ( 'NONE',  ( -14.90395405082875335, 14.90835605916499418, 11.49999999999998934 ) ) ;
#43611 = CARTESIAN_POINT ( 'NONE',  ( -60.55620429048339304, -25.00182538069145011, 7.747789668545098429 ) ) ;
#43612 = AXIS2_PLACEMENT_3D ( 'NONE', #35443, #43553, #83088 ) ;
#43613 = PLANE ( 'NONE',  #65760 ) ;
#43615 = CARTESIAN_POINT ( 'NONE',  ( -96.92287095715006728, -23.47596703998600631, 11.44779298504227860 ) ) ;
#43614 = CIRCLE ( 'NONE', #74389, 1.699999999999999289 ) ;
#43616 = CARTESIAN_POINT ( 'NONE',  ( 10.62437663934349530, -6.475225279485576024, -27.03002426119959978 ) ) ;
#43617 = CARTESIAN_POINT ( 'NONE',  ( -129.5561478186664601, -23.48786465467241769, 11.44779295918253759 ) ) ;
#43618 = CARTESIAN_POINT ( 'NONE',  ( -21.51168160490077952, -5.175097382202364926, -1.500000000000002220 ) ) ;
#43619 = CYLINDRICAL_SURFACE ( 'NONE', #72735, 0.3000000000000016542 ) ;
#43620 = ADVANCED_FACE ( 'NONE', ( #81464 ), #62193, .T. ) ;
#43621 = CARTESIAN_POINT ( 'NONE',  ( -108.9545715455115129, -25.27705962214097113, 4.170144839539424275 ) ) ;
#43622 = CARTESIAN_POINT ( 'NONE',  ( -83.58953762381672448, -23.47593901973091235, -1.443836447539004642 ) ) ;
#43623 = VECTOR ( 'NONE', #87512, 1000.000000000000000 ) ;
#43624 = FACE_OUTER_BOUND ( 'NONE', #31322, .T. ) ;
#43625 = EDGE_CURVE ( 'NONE', #922, #26773, #99646, .T. ) ;
#43626 = VECTOR ( 'NONE', #14927, 1000.000000000000000 ) ;
#43627 = CARTESIAN_POINT ( 'NONE',  ( 7.684279652734260502, -19.92951104315265809, 11.49999999999998934 ) ) ;
#43628 = CARTESIAN_POINT ( 'NONE',  ( -26.09993462008742426, -24.96876793076006251, 5.209353322998722113 ) ) ;
#43629 = LINE ( 'NONE', #97407, #56036 ) ;
#43630 = LINE ( 'NONE', #57380, #69767 ) ;
#43631 = DIRECTION ( 'NONE',  ( -0.000000000000000000, -0.000000000000000000, -1.000000000000000000 ) ) ;
#43632 = CARTESIAN_POINT ( 'NONE',  ( -15.40814491850785650, 16.58152744545821022, -1.500000000000002220 ) ) ;
#43633 = ORIENTED_EDGE ( 'NONE', *, *, #90792, .F. ) ;
#43634 = DIRECTION ( 'NONE',  ( -3.773278334444166432E-23, 1.000000000000000000, 0.000000000000000000 ) ) ;
#43635 = CARTESIAN_POINT ( 'NONE',  ( -13.19171355488933983, -14.64934158388261665, 11.49999999999999645 ) ) ;
#43636 = CARTESIAN_POINT ( 'NONE',  ( -5.366453405989236813, -2.000000000000001776, 18.24068255301867936 ) ) ;
#43637 = AXIS2_PLACEMENT_3D ( 'NONE', #19701, #18706, #80616 ) ;
#43638 = B_SPLINE_CURVE_WITH_KNOTS ( 'NONE', 3,
 ( #85468, #738, #16961, #95092, #86475, #32184 ),
 .UNSPECIFIED., .F., .F.,
 ( 4, 2, 4 ),
 ( 0.000000000000000000, 0.001380901958385380088, 0.002761803916770760176 ),
 .UNSPECIFIED. ) ;
#43639 = CARTESIAN_POINT ( 'NONE',  ( -119.5228709571501469, -24.34917612406838217, 0.1852690917426614570 ) ) ;
#43640 = VERTEX_POINT ( 'NONE', #90558 ) ;
#43641 = CARTESIAN_POINT ( 'NONE',  ( -8.749999999999767297, 18.74999999999999645, 0.000000000000000000 ) ) ;
#43642 = CARTESIAN_POINT ( 'NONE',  ( -29.02540380353726590, -24.60094009216138744, 2.175343837210148124 ) ) ;
#43643 = DIRECTION ( 'NONE',  ( -0.8246584009594635223, 0.5656310827093757876, 1.065814103640150279E-14 ) ) ;
#43644 = CARTESIAN_POINT ( 'NONE',  ( -19.46174652491427182, -9.421329337880418819, 11.49999999999998934 ) ) ;
#43645 = CARTESIAN_POINT ( 'NONE',  ( -29.49875734969026198, 5.965225279485572685, 7.870022800118625206 ) ) ;
#43646 = CARTESIAN_POINT ( 'NONE',  ( -4.359330469889163950, 18.88329184224734192, -1.500000000000002220 ) ) ;
#43647 = DIRECTION ( 'NONE',  ( -0.9994733861282923959, -0.000000000000000000, -0.03244919754393515293 ) ) ;
#43648 = CARTESIAN_POINT ( 'NONE',  ( -81.31915660432444781, -25.09456864601564519, 7.311523710026984091 ) ) ;
#43649 = EDGE_CURVE ( 'NONE', #47809, #48068, #21530, .T. ) ;
#43650 = CARTESIAN_POINT ( 'NONE',  ( 19.60560811685724403, 2.727087469661350738, -1.500000000000002220 ) ) ;
#43651 = VERTEX_POINT ( 'NONE', #51511 ) ;
#43652 = CARTESIAN_POINT ( 'NONE',  ( 18.08294815051442583, 9.098846914115775064, 11.49999999999999645 ) ) ;
#43653 = DIRECTION ( 'NONE',  ( -0.000000000000000000, 1.000000000000000000, -0.000000000000000000 ) ) ;
#43654 = B_SPLINE_CURVE_WITH_KNOTS ( 'NONE', 3,
 ( #48729, #24366, #16746, #2544, #34487, #71052 ),
 .UNSPECIFIED., .F., .F.,
 ( 4, 2, 4 ),
 ( 0.000000000000000000, 0.001380764517853248600, 0.002761529035706497201 ),
 .UNSPECIFIED. ) ;
#43655 = EDGE_CURVE ( 'NONE', #65722, #21736, #5821, .T. ) ;
#43656 = B_SPLINE_CURVE_WITH_KNOTS ( 'NONE', 3,
 ( #26540, #41264, #57504, #72718, #3216, #86429, #48882, #26028 ),
 .UNSPECIFIED., .F., .F.,
 ( 4, 2, 2, 4 ),
 ( -0.001224873891641426295, -0.0002244903592271089293, 0.0007758931731872084365, 0.002776660238015842518 ),
 .UNSPECIFIED. ) ;
#43657 = VECTOR ( 'NONE', #92055, 1000.000000000000000 ) ;
#43658 = EDGE_LOOP ( 'NONE', ( #91318, #61794, #78780, #66197, #99186, #19858, #91520, #24642, #57108, #87331, #70295 ) ) ;
#43659 = B_SPLINE_SURFACE_WITH_KNOTS ( 'NONE', 3, 3, ( 
 ( #76490, #68893, #61301, #92227 ),
 ( #39451, #8501, #86120, #32840 ),
 ( #55692, #17106, #92718, #78999 ),
 ( #15105, #23206, #62810, #23712 ) ),
 .UNSPECIFIED., .F., .F., .F.,
 ( 4, 4 ),
 ( 4, 4 ),
 ( 0.3743040175512771239, 0.5066054860718446351 ),
 ( 0.8909579831155240992, 0.9113928628922632891 ),
 .UNSPECIFIED. ) ;
#43660 = CARTESIAN_POINT ( 'NONE',  ( -28.98875734969026396, 5.965225279485572685, -0.08597719988137648983 ) ) ;
#43661 = CARTESIAN_POINT ( 'NONE',  ( 31.61049571213237641, 4.540774720514426654, 26.28206907949443050 ) ) ;
#43662 = CARTESIAN_POINT ( 'NONE',  ( -71.52287095715007581, -23.48786465467241058, 11.44779295918254647 ) ) ;
#43663 = DIRECTION ( 'NONE',  ( 0.000000000000000000, 0.9967269304714136968, 0.08084198211964954695 ) ) ;
#43664 = CARTESIAN_POINT ( 'NONE',  ( -1.304987980769231948, -6.376774720514413630, 19.76512419871795245 ) ) ;
#43665 = CARTESIAN_POINT ( 'NONE',  ( 0.1258803491696451060, 20.03332480481931199, 11.49999999999998934 ) ) ;
#43666 = PLANE ( 'NONE',  #9440 ) ;
#43667 = ORIENTED_EDGE ( 'NONE', *, *, #69398, .F. ) ;
#43668 = CARTESIAN_POINT ( 'NONE',  ( -102.5228709571500758, -24.64898659630367916, 1.056161002820829697 ) ) ;
#43669 = CARTESIAN_POINT ( 'NONE',  ( -82.55620429048337883, -24.65952944569304606, 1.056160979905699460 ) ) ;
#43670 = PLANE ( 'NONE',  #32224 ) ;
#43671 = CARTESIAN_POINT ( 'NONE',  ( -113.5228709571500758, -24.33832256527049154, 0.1851278514138635367 ) ) ;
#43672 = DIRECTION ( 'NONE',  ( -1.000000000000000000, -3.773278334444167608E-23, -8.201307810031802745E-29 ) ) ;
#43673 = DIRECTION ( 'NONE',  ( -1.000000000000000000, -0.000000000000000000, -0.000000000000000000 ) ) ;
#43674 = ORIENTED_EDGE ( 'NONE', *, *, #84833, .T. ) ;
#43675 = VECTOR ( 'NONE', #41966, 1000.000000000000114 ) ;
#43676 = CARTESIAN_POINT ( 'NONE',  ( -18.23349369547262810, -8.965252873808195133, -1.500000000000002220 ) ) ;
#43677 = ORIENTED_EDGE ( 'NONE', *, *, #67328, .T. ) ;
#43678 = CARTESIAN_POINT ( 'NONE',  ( 22.25235761598246143, -5.642936543268669780, 11.49999999999998934 ) ) ;
#43679 = CARTESIAN_POINT ( 'NONE',  ( -65.52287095715006160, -23.47593901973090169, -1.443836447538996870 ) ) ;
#43680 = ORIENTED_EDGE ( 'NONE', *, *, #6591, .F. ) ;
#43681 = AXIS2_PLACEMENT_3D ( 'NONE', #84258, #84762, #60944 ) ;
#43682 = CARTESIAN_POINT ( 'NONE',  ( -27.25988310792305214, 0.3587747205144265483, 30.32664379231667695 ) ) ;
#43683 = CARTESIAN_POINT ( 'NONE',  ( -49.29494865489761679, -25.26264011037805801, 6.331091240045351398 ) ) ;
#43684 = AXIS2_PLACEMENT_3D ( 'NONE', #4242, #28077, #88981 ) ;
#43685 = CARTESIAN_POINT ( 'NONE',  ( 33.74607884027702909, 5.965225279485572685, -4.999864028243830916 ) ) ;
#43687 = ORIENTED_EDGE ( 'NONE', *, *, #94550, .F. ) ;
#43686 = CARTESIAN_POINT ( 'NONE',  ( -19.34623641613454836, -8.721557147202650739, 11.49999999999999645 ) ) ;
#43688 = VECTOR ( 'NONE', #69110, 1000.000000000000114 ) ;
#43689 = ORIENTED_EDGE ( 'NONE', *, *, #17714, .T. ) ;
#43690 = CARTESIAN_POINT ( 'NONE',  ( -19.06252244145942498, 11.34236556261432405, -1.500000000000002220 ) ) ;
#43691 = CARTESIAN_POINT ( 'NONE',  ( 16.39479758508079144, -12.47777281027006424, 11.49999999999998934 ) ) ;
#43693 = ORIENTED_EDGE ( 'NONE', *, *, #46692, .F. ) ;
#43692 = AXIS2_PLACEMENT_3D ( 'NONE', #37852, #8395, #7388 ) ;
#43694 = ORIENTED_EDGE ( 'NONE', *, *, #43275, .F. ) ;
#43695 = CARTESIAN_POINT ( 'NONE',  ( 13.74975846015576586, 5.965225279485572685, -27.72022515045486557 ) ) ;
#43696 = PLANE ( 'NONE',  #80991 ) ;
#43697 = EDGE_LOOP ( 'NONE', ( #24400, #75612, #13747, #5585, #68895, #13478, #49937, #68038, #49170, #27481, #77984, #24149, #65825, #15256, #64738, #99524, #63912 ) ) ;
#43699 = VERTEX_POINT ( 'NONE', #44901 ) ;
#43698 = EDGE_CURVE ( 'NONE', #3121, #94573, #80560, .T. ) ;
#43700 = ORIENTED_EDGE ( 'NONE', *, *, #45488, .F. ) ;
#43701 = CARTESIAN_POINT ( 'NONE',  ( -111.7692696073655156, -25.28511524806629041, 4.136510707875227233 ) ) ;
#43702 = CARTESIAN_POINT ( 'NONE',  ( -28.48666779331410481, -24.18640622799667028, 9.817618374534074377 ) ) ;
#43703 = CARTESIAN_POINT ( 'NONE',  ( 14.83405752585475135, -4.881907540128472611, -27.54622755360324859 ) ) ;
#43704 = CARTESIAN_POINT ( 'NONE',  ( -4.307737697753418082, 20.33289072680551968, -1.500000000000002220 ) ) ;
#43705 = CARTESIAN_POINT ( 'NONE',  ( -17.03913561245058261, -13.47071831616118942, 11.49999999999999645 ) ) ;
#43706 = ORIENTED_EDGE ( 'NONE', *, *, #17773, .T. ) ;
#43707 = ADVANCED_FACE ( 'NONE', ( #59626 ), #91297, .T. ) ;
#43708 = CARTESIAN_POINT ( 'NONE',  ( -40.81961785418572930, -25.27806125868308484, 5.018035830796276464 ) ) ;
#43709 = CARTESIAN_POINT ( 'NONE',  ( -34.55620429048339304, -23.47596703998600276, 11.44779298504227505 ) ) ;
#43710 = CARTESIAN_POINT ( 'NONE',  ( -115.5568011907884483, -23.85016227208580730, -0.8807180028928282001 ) ) ;
#43711 = CARTESIAN_POINT ( 'NONE',  ( -19.61019785865472542, -10.87575402790796453, -1.500000000000002220 ) ) ;
#43712 = EDGE_CURVE ( 'NONE', #30369, #2649, #22522, .T. ) ;
#43713 = CARTESIAN_POINT ( 'NONE',  ( -51.19090461678316473, -25.26334662982828405, 4.328065714047625079 ) ) ;
#43714 = CARTESIAN_POINT ( 'NONE',  ( -65.49582848406727464, -24.52300882791528736, 0.6510814631126250474 ) ) ;
#43715 = VERTEX_POINT ( 'NONE', #60631 ) ;
#43716 = CARTESIAN_POINT ( 'NONE',  ( -71.20541289166536103, -25.31502801509702749, 4.885889949323629189 ) ) ;
#43717 = CARTESIAN_POINT ( 'NONE',  ( 18.72495633783376334, -0.5000000000000000000, 2.346898003627108320 ) ) ;
#43718 = EDGE_CURVE ( 'NONE', #2778, #26032, #100134, .T. ) ;
#43719 = ORIENTED_EDGE ( 'NONE', *, *, #89436, .F. ) ;
#43720 = MANIFOLD_SOLID_BREP ( 'Kes-Ekstr\X2\00fc\X0\zyon1', #58224 ) ;
#43721 = EDGE_CURVE ( 'NONE', #27242, #75066, #20538, .T. ) ;
#43722 = ORIENTED_EDGE ( 'NONE', *, *, #45186, .T. ) ;
#43723 = CARTESIAN_POINT ( 'NONE',  ( -10.34999999999999254, 3.983606557377048940, 3.319672131147540561 ) ) ;
#43724 = ORIENTED_EDGE ( 'NONE', *, *, #46793, .T. ) ;
#43725 = CARTESIAN_POINT ( 'NONE',  ( 15.78869406909177897, -14.30566568001193950, -1.500000000000002220 ) ) ;
#43726 = VERTEX_POINT ( 'NONE', #53013 ) ;
#43727 = CARTESIAN_POINT ( 'NONE',  ( -5.891837592278976743, -5.876774720514418959, 20.62654306927474934 ) ) ;
#43728 = CARTESIAN_POINT ( 'NONE',  ( 17.34737195785526609, 13.27887811287985187, -1.500000000000002220 ) ) ;
#43729 = DIRECTION ( 'NONE',  ( -1.000000000000000000, 0.000000000000000000, 0.000000000000000000 ) ) ;
#43730 = CARTESIAN_POINT ( 'NONE',  ( 21.55457256799317278, 7.124301260279622738, -1.500000000000002220 ) ) ;
#43731 = CARTESIAN_POINT ( 'NONE',  ( -112.6228709571500417, -24.65952944569304961, 1.056160979905702346 ) ) ;
#43732 = CARTESIAN_POINT ( 'NONE',  ( 10.86264265030973952, -5.965225279485574461, -28.05717073599341305 ) ) ;
#43733 = CARTESIAN_POINT ( 'NONE',  ( 18.29167757401336303, -12.14499471347784798, -1.500000000000002220 ) ) ;
#43734 = CARTESIAN_POINT ( 'NONE',  ( -87.63200249025274502, -24.15543982623908548, -0.2315651400026449980 ) ) ;
#43735 = VERTEX_POINT ( 'NONE', #83943 ) ;
#43736 = EDGE_CURVE ( 'NONE', #44198, #55557, #43895, .T. ) ;
#43737 = CARTESIAN_POINT ( 'NONE',  ( -40.05769137787242329, -25.29480120415430733, 5.514493779961309627 ) ) ;
#43738 = PLANE ( 'NONE',  #86449 ) ;
#43739 = EDGE_CURVE ( 'NONE', #96245, #89859, #76809, .T. ) ;
#43740 = EDGE_LOOP ( 'NONE', ( #70241, #52822, #51570, #76520 ) ) ;
#43741 = CARTESIAN_POINT ( 'NONE',  ( -28.98875734969026396, 0.3587747205144262708, 7.870022800118625206 ) ) ;
#43742 = CARTESIAN_POINT ( 'NONE',  ( -130.5728709571501156, -24.75152770810921510, 1.363349870542273523 ) ) ;
#43743 = CARTESIAN_POINT ( 'NONE',  ( -30.58711349467732532, -25.14094028198826436, 2.712351064733613537 ) ) ;
#43744 = CARTESIAN_POINT ( 'NONE',  ( -18.64022381217131397, 10.26305532446727753, -1.500000000000002220 ) ) ;
#43745 = FACE_OUTER_BOUND ( 'NONE', #24709, .T. ) ;
#43746 = CARTESIAN_POINT ( 'NONE',  ( -26.42246413733907673, -24.97064590431050846, 3.141772897168136236 ) ) ;
#43747 = AXIS2_PLACEMENT_3D ( 'NONE', #92940, #47791, #78215 ) ;
#43748 = FACE_OUTER_BOUND ( 'NONE', #83924, .T. ) ;
#43749 = PLANE ( 'NONE',  #47542 ) ;
#43750 = CARTESIAN_POINT ( 'NONE',  ( -90.62287095715004170, -24.99132157543084531, 2.256160258750667502 ) ) ;
#43751 = EDGE_LOOP ( 'NONE', ( #25747, #47310, #50112, #5227 ) ) ;
#43752 = CARTESIAN_POINT ( 'NONE',  ( -14.26233628608129855, 13.40890954296891024, 11.49999999999999645 ) ) ;
#43753 = CARTESIAN_POINT ( 'NONE',  ( -58.62287095715005592, -24.51387760970723662, 9.387446482453421837 ) ) ;
#43754 = AXIS2_PLACEMENT_3D ( 'NONE', #87877, #56944, #86864 ) ;
#43755 = CARTESIAN_POINT ( 'NONE',  ( -29.78631988578491629, -25.22684763970347888, 5.682124227929016058 ) ) ;
#43756 = VERTEX_POINT ( 'NONE', #28664 ) ;
#43757 = CARTESIAN_POINT ( 'NONE',  ( -117.5228709571500758, -23.47596703998600631, 11.44779298504227860 ) ) ;
#43758 = CARTESIAN_POINT ( 'NONE',  ( -101.7073711143522416, -25.15401000799511522, 6.923429918029315289 ) ) ;
#43759 = VECTOR ( 'NONE', #79785, 1000.000000000000000 ) ;
#43760 = CARTESIAN_POINT ( 'NONE',  ( -27.06750426676058296, -24.63035931427080882, 8.145542352137882247 ) ) ;
#43761 = CARTESIAN_POINT ( 'NONE',  ( -40.62287095715005592, -23.47596703998600276, 11.44779298504227505 ) ) ;
#43762 = CARTESIAN_POINT ( 'NONE',  ( -11.91260469445801995, 15.66180005371307260, -1.500000000000002220 ) ) ;
#43763 = AXIS2_PLACEMENT_3D ( 'NONE', #25081, #49447, #10871 ) ;
#43764 = ORIENTED_EDGE ( 'NONE', *, *, #85741, .T. ) ;
#43765 = CIRCLE ( 'NONE', #59927, 1.000000000000000000 ) ;
#43766 = B_SPLINE_CURVE_WITH_KNOTS ( 'NONE', 3,
 ( #21284, #68478, #14172, #5073, #98911, #99411, #45147, #76074, #36518, #36023, #37024, #13670, #6070, #6573, #37524, #82692 ),
 .UNSPECIFIED., .F., .F.,
 ( 4, 2, 2, 2, 2, 2, 2, 4 ),
 ( 0.000000000000000000, 0.0002294183186423333083, 0.0004588366372846666165, 0.0006882549559270000061, 0.0009176732745693332331, 0.001376509911854000012, 0.001605928230496330746, 0.001835346549138661262 ),
 .UNSPECIFIED. ) ;
#43767 = CARTESIAN_POINT ( 'NONE',  ( 10.84340024150424497, 4.021317321268781164, -26.91457715659927175 ) ) ;
#43768 = CARTESIAN_POINT ( 'NONE',  ( 30.61238849909758031, -3.934983946744459171, 27.21775687185679615 ) ) ;
#43769 = AXIS2_PLACEMENT_3D ( 'NONE', #35991, #65978, #20256 ) ;
#43770 = DATE_TIME_ROLE ( 'creation_date' ) ;
#43771 = ADVANCED_FACE ( 'NONE', ( #38261 ), #69219, .T. ) ;
#43772 = EDGE_LOOP ( 'NONE', ( #17983, #12810, #27599, #37200 ) ) ;
#43773 = CARTESIAN_POINT ( 'NONE',  ( 8.097539468418187170, -0.7382521156407163554, 3.736985260579222867 ) ) ;
#43774 = CARTESIAN_POINT ( 'NONE',  ( -45.62287095715004881, -24.15516710230293995, 10.28746687063725318 ) ) ;
#43775 = CARTESIAN_POINT ( 'NONE',  ( -47.65343445879282314, -23.73766607897670866, -1.055555164236438914 ) ) ;
#43776 = CARTESIAN_POINT ( 'NONE',  ( -62.62287095715004881, -23.47593901973091235, -1.443836447539007972 ) ) ;
#43777 = DIRECTION ( 'NONE',  ( 0.000000000000000000, 0.000000000000000000, -1.000000000000000000 ) ) ;
#43778 = DIRECTION ( 'NONE',  ( 0.000000000000000000, -2.173523156925980399E-06, 0.9999999999976378895 ) ) ;
#43779 = CARTESIAN_POINT ( 'NONE',  ( -107.5890209867514642, -24.34968618360934300, 0.1864209137778969627 ) ) ;
#43780 = CARTESIAN_POINT ( 'NONE',  ( 8.914523860536577970, -17.85282776015759154, -1.500000000000002220 ) ) ;
#43781 = EDGE_CURVE ( 'NONE', #93033, #68551, #68518, .T. ) ;
#43782 = CARTESIAN_POINT ( 'NONE',  ( -37.52287095715008292, -23.48783264083359512, -1.443836473376374885 ) ) ;
#43783 = CARTESIAN_POINT ( 'NONE',  ( -0.1141154322660206111, -21.57268605278876805, 10.89591856040522266 ) ) ;
#43784 = ORIENTED_EDGE ( 'NONE', *, *, #87111, .T. ) ;
#43785 = FACE_OUTER_BOUND ( 'NONE', #22329, .T. ) ;
#43786 = DIRECTION ( 'NONE',  ( 0.000000000000000000, 0.000000000000000000, 1.000000000000000000 ) ) ;
#43787 = SHAPE_REPRESENTATION_RELATIONSHIP ( 'NONE' , 'NONE' ,  #37291, #30696 ) ;
#43788 = LINE ( 'NONE', #61515, #83192 ) ;
#43789 = DIRECTION ( 'NONE',  ( 0.000000000000000000, 0.000000000000000000, 1.000000000000000000 ) ) ;
#43790 = CARTESIAN_POINT ( 'NONE',  ( -39.60860462615423927, -23.73766607897669800, -1.055555164236461341 ) ) ;
#43791 = CARTESIAN_POINT ( 'NONE',  ( -64.52287095715007581, -23.96127896941631619, -0.6493128931038050222 ) ) ;
#43792 = CC_DESIGN_PERSON_AND_ORGANIZATION_ASSIGNMENT ( #49537, #96686, ( #19911 ) ) ;
#43793 = CARTESIAN_POINT ( 'NONE',  ( -51.19681519762799127, -25.26280088862281659, 4.857314488523241991 ) ) ;
#43794 = ORIENTED_EDGE ( 'NONE', *, *, #7856, .F. ) ;
#43795 = CARTESIAN_POINT ( 'NONE',  ( -71.62287095715005592, -24.65952944569304606, 1.056160979905699016 ) ) ;
#43796 = CARTESIAN_POINT ( 'NONE',  ( -127.5896358177784862, -24.34968618360935011, 0.1864209137778924386 ) ) ;
#43797 = VERTEX_POINT ( 'NONE', #62120 ) ;
#43798 = CARTESIAN_POINT ( 'NONE',  ( -0.9278407348523283193, 20.21260682001012654, 11.49999999999998934 ) ) ;
#43799 = CARTESIAN_POINT ( 'NONE',  ( -105.6228709571500559, -23.48786465467241769, 11.44779295918253759 ) ) ;
#43800 = CARTESIAN_POINT ( 'NONE',  ( 25.61870917940689196, 5.965225279485572685, 29.49402280011862487 ) ) ;
#43801 = CARTESIAN_POINT ( 'NONE',  ( -80.62287095715005592, -29.50247984919015209, -1.443849546365053582 ) ) ;
#43802 = ORIENTED_EDGE ( 'NONE', *, *, #23191, .F. ) ;
#43803 = DIRECTION ( 'NONE',  ( -1.250792852327444499E-32, -1.571307496355802709E-16, -1.000000000000000000 ) ) ;
#43804 = CARTESIAN_POINT ( 'NONE',  ( 22.02124265030973760, 6.143225279485574397, 19.55402280011862004 ) ) ;
#43805 = CARTESIAN_POINT ( 'NONE',  ( -19.29710791919172053, 5.528754708966634901, -1.500000000000002220 ) ) ;
#43806 = CARTESIAN_POINT ( 'NONE',  ( 3.785439364192078937, -20.66625369722972749, 11.49999999999999645 ) ) ;
#43807 = FACE_OUTER_BOUND ( 'NONE', #67422, .T. ) ;
#43808 = CARTESIAN_POINT ( 'NONE',  ( -32.52287095715004739, -23.96127896942119051, -0.6493128930941857169 ) ) ;
#43809 = CARTESIAN_POINT ( 'NONE',  ( -13.58966412916292299, 17.40808962483262690, -1.500000000000002220 ) ) ;
#43810 = AXIS2_PLACEMENT_3D ( 'NONE', #100189, #78367, #99697 ) ;
#43811 = DIRECTION ( 'NONE',  ( -3.773278334444168195E-23, 1.000000000000000000, 0.000000000000000000 ) ) ;
#43812 = CARTESIAN_POINT ( 'NONE',  ( -34.58953762381672448, -23.47593901973091235, -1.443836447539013301 ) ) ;
#43813 = DIRECTION ( 'NONE',  ( -1.000000000000000000, -3.773278334444167608E-23, -8.201307833595939069E-29 ) ) ;
#43814 = ORIENTED_EDGE ( 'NONE', *, *, #35751, .T. ) ;
#43815 = LINE ( 'NONE', #6736, #62415 ) ;
#43816 = CARTESIAN_POINT ( 'NONE',  ( -31.62935866127120832, -24.51314013834316086, 0.6176544820404139546 ) ) ;
#43817 = EDGE_LOOP ( 'NONE', ( #56345, #36847, #17400, #14326 ) ) ;
#43818 = B_SPLINE_CURVE_WITH_KNOTS ( 'NONE', 3,
 ( #84719, #22801, #37551, #70504, #45669, #77596 ),
 .UNSPECIFIED., .F., .F.,
 ( 4, 2, 4 ),
 ( 6.390294094803335792E-06, 0.001387608157368792720, 0.002768826020642782028 ),
 .UNSPECIFIED. ) ;
#43819 = ORIENTED_EDGE ( 'NONE', *, *, #90665, .T. ) ;
#43820 = DIRECTION ( 'NONE',  ( 1.000000000000000000, 0.000000000000000000, 0.000000000000000000 ) ) ;
#43821 = LINE ( 'NONE', #67173, #34046 ) ;
#43822 = CARTESIAN_POINT ( 'NONE',  ( -76.56415044752040444, -23.48783264082477373, -1.443836473390089026 ) ) ;
#43823 = CARTESIAN_POINT ( 'NONE',  ( 17.26003113218828489, 11.23261964116016642, -1.500000000000002220 ) ) ;
#43824 = CARTESIAN_POINT ( 'NONE',  ( -14.35963886870962192, 16.04489112172382903, 11.49999999999999645 ) ) ;
#43825 = ORIENTED_EDGE ( 'NONE', *, *, #13007, .F. ) ;
#43826 = CARTESIAN_POINT ( 'NONE',  ( -91.55809077531434070, -23.73766607897670156, -1.055555164236454235 ) ) ;
#43827 = DIRECTION ( 'NONE',  ( 1.000000000000000000, 4.015954566446630556E-15, 0.000000000000000000 ) ) ;
#43828 = CARTESIAN_POINT ( 'NONE',  ( -4.401146115524053215, -6.376774720514411854, 19.34190049657481936 ) ) ;
#43829 = CARTESIAN_POINT ( 'NONE',  ( 21.44611857939883137, 6.294191480875499067, -1.500000000000002220 ) ) ;
#43830 = CARTESIAN_POINT ( 'NONE',  ( 1.461421362798841272, 13.73150565671347678, 0.000000000000000000 ) ) ;
#43831 = DIRECTION ( 'NONE',  ( 0.000000000000000000, -0.8183310589170136318, 0.5747471426738539613 ) ) ;
#43832 = EDGE_LOOP ( 'NONE', ( #65399, #3703, #73312, #72320 ) ) ;
#43833 = CARTESIAN_POINT ( 'NONE',  ( -67.52287095715006160, -24.64965694238407323, 8.947790433994200043 ) ) ;
#43834 = AXIS2_PLACEMENT_3D ( 'NONE', #15149, #51728, #35993 ) ;
#43835 = CARTESIAN_POINT ( 'NONE',  ( 3.557932825399831689, -5.876774720514428729, 21.44518044978141091 ) ) ;
#43836 = ADVANCED_FACE ( 'NONE', ( #46381 ), #1215, .T. ) ;
#43837 = AXIS2_PLACEMENT_3D ( 'NONE', #4865, #43927, #22064 ) ;
#43838 = CARTESIAN_POINT ( 'NONE',  ( 6.973883220674568229, 19.69035807221911938, 11.49999999999998934 ) ) ;
#43839 = EDGE_CURVE ( 'NONE', #82501, #2671, #25036, .T. ) ;
#43840 = ORIENTED_EDGE ( 'NONE', *, *, #80136, .T. ) ;
#43841 = B_SPLINE_CURVE_WITH_KNOTS ( 'NONE', 3,
 ( #38870, #54119, #1323, #69829, #86047, #70330 ),
 .UNSPECIFIED., .F., .F.,
 ( 4, 2, 4 ),
 ( 0.000000000000000000, 0.001380901958385393966, 0.002761803916770787931 ),
 .UNSPECIFIED. ) ;
#43843 = VERTEX_POINT ( 'NONE', #94050 ) ;
#43842 = DIRECTION ( 'NONE',  ( 1.000000000000000000, 3.773278334444167608E-23, 8.201307833595939069E-29 ) ) ;
#43844 = EDGE_LOOP ( 'NONE', ( #5728, #92950, #266, #92140 ) ) ;
#43845 = AXIS2_PLACEMENT_3D ( 'NONE', #48757, #56875, #10178 ) ;
#43846 = CARTESIAN_POINT ( 'NONE',  ( -100.5450565129023062, -24.92592662359561473, 8.075495903018000021 ) ) ;
#43847 = CARTESIAN_POINT ( 'NONE',  ( -13.65698368949537311, 16.12507722524849996, -1.500000000000002220 ) ) ;
#43848 = ORIENTED_EDGE ( 'NONE', *, *, #2203, .T. ) ;
#43849 = CARTESIAN_POINT ( 'NONE',  ( -117.6235066561394973, -24.65952944569305316, 1.056160979905706343 ) ) ;
#43850 = CARTESIAN_POINT ( 'NONE',  ( -102.6228709571500701, -23.72773821059536559, 11.05748984161097503 ) ) ;
#43851 = CARTESIAN_POINT ( 'NONE',  ( -98.52287095715006160, -29.50250786944525672, 11.44777988621623166 ) ) ;
#43852 = LINE ( 'NONE', #80910, #74477 ) ;
#43853 = CARTESIAN_POINT ( 'NONE',  ( -129.6228709571500417, -23.47596703998600631, 11.44779298504227683 ) ) ;
#43854 = CARTESIAN_POINT ( 'NONE',  ( -12.78816955685674372, 17.57309652720472570, -1.500000000000002220 ) ) ;
#43855 = CARTESIAN_POINT ( 'NONE',  ( -80.09821655188528666, -25.05200611405530609, 7.521384686245699669 ) ) ;
#43857 = ORIENTED_EDGE ( 'NONE', *, *, #90940, .F. ) ;
#43856 = CARTESIAN_POINT ( 'NONE',  ( -3.941980378682776287, 21.93750326593198352, 11.49999999999999645 ) ) ;
#43858 = EDGE_CURVE ( 'NONE', #76458, #86377, #71764, .T. ) ;
#43859 = LINE ( 'NONE', #21988, #6455 ) ;
#43860 = CARTESIAN_POINT ( 'NONE',  ( -95.52287095715006160, -23.48786465467241769, 11.44779295918254114 ) ) ;
#43861 = CARTESIAN_POINT ( 'NONE',  ( -88.88918693012689687, -25.22391110550272941, 6.409327647371936720 ) ) ;
#43862 = ORIENTED_EDGE ( 'NONE', *, *, #58876, .T. ) ;
#43863 = ORIENTED_EDGE ( 'NONE', *, *, #74063, .T. ) ;
#43864 = ORIENTED_EDGE ( 'NONE', *, *, #77232, .T. ) ;
#43865 = DIRECTION ( 'NONE',  ( -1.000000000000000000, 0.000000000000000000, 0.000000000000000000 ) ) ;
#43866 = CARTESIAN_POINT ( 'NONE',  ( -86.52287095715006160, -23.47596703998600631, 11.44779298504228393 ) ) ;
#43867 = DIRECTION ( 'NONE',  ( 3.773278334444166432E-23, -1.000000000000000000, 0.000000000000000000 ) ) ;
#43868 = LINE ( 'NONE', #35760, #98875 ) ;
#43869 = CARTESIAN_POINT ( 'NONE',  ( -12.28997142660015740, 14.97987746540053422, -1.500000000000002220 ) ) ;
#43870 = CARTESIAN_POINT ( 'NONE',  ( -36.62287095715005592, -24.66019654487199020, 8.947790411086138818 ) ) ;
#43871 = ORIENTED_EDGE ( 'NONE', *, *, #80151, .T. ) ;
#43872 = CARTESIAN_POINT ( 'NONE',  ( 11.07193147992585835, -15.93265361536492364, 11.49999999999999645 ) ) ;
#43873 = CYLINDRICAL_SURFACE ( 'NONE', #84379, 9.999999999999991118 ) ;
#43874 = B_SPLINE_CURVE_WITH_KNOTS ( 'NONE', 3,
 ( #89226, #80110, #4499, #35444, #20197, #12592, #72514, #74491 ),
 .UNSPECIFIED., .F., .F.,
 ( 4, 2, 2, 4 ),
 ( 6.384118678612269921E-06, 0.002007151183507259289, 0.003007534715921582943, 0.004007918248335905730 ),
 .UNSPECIFIED. ) ;
#43875 = ORIENTED_EDGE ( 'NONE', *, *, #23087, .F. ) ;
#43876 = CARTESIAN_POINT ( 'NONE',  ( 3.296033061219842519, -5.876774720514406525, 18.71226942120119574 ) ) ;
#43877 = CARTESIAN_POINT ( 'NONE',  ( 8.720390671778812219, 3.316774720514306996, -27.07197491306147086 ) ) ;
#43878 = CARTESIAN_POINT ( 'NONE',  ( -102.6228709571500275, -24.34917612406837861, 0.1852690917426659811 ) ) ;
#43879 = B_SPLINE_CURVE_WITH_KNOTS ( 'NONE', 3,
 ( #54514, #8330, #38777, #63642 ),
 .UNSPECIFIED., .F., .F.,
 ( 4, 4 ),
 ( 0.6402431064082777512, 0.6492495376803931739 ),
 .UNSPECIFIED. ) ;
#43880 = CARTESIAN_POINT ( 'NONE',  ( -87.62287095715001328, -23.95044443724992078, 10.65354141964649415 ) ) ;
#43881 = ADVANCED_FACE ( 'NONE', ( #17428 ), #39262, .T. ) ;
#43882 = CARTESIAN_POINT ( 'NONE',  ( 19.52168601723349894, 1.684101417132040979, -1.500000000000002220 ) ) ;
#43883 = DIRECTION ( 'NONE',  ( 0.000000000000000000, 0.000000000000000000, 1.000000000000000000 ) ) ;
#43884 = VERTEX_POINT ( 'NONE', #16416 ) ;
#43885 = CARTESIAN_POINT ( 'NONE',  ( -0.8629811567608781653, -21.54619324973139172, -1.500000000000002220 ) ) ;
#43886 = DIRECTION ( 'NONE',  ( -3.773278334453079030E-23, 0.9999999999976377785, 2.173523156925979128E-06 ) ) ;
#43887 = LINE ( 'NONE', #44895, #96701 ) ;
#43888 = CARTESIAN_POINT ( 'NONE',  ( -62.52287095715006160, -24.64965694238406613, 8.947790433994201820 ) ) ;
#43889 = AXIS2_PLACEMENT_3D ( 'NONE', #15871, #8269, #9260 ) ;
#43890 = CARTESIAN_POINT ( 'NONE',  ( -10.59832330691884117, -6.376774720514425177, -27.05373799718301697 ) ) ;
#43891 = CARTESIAN_POINT ( 'NONE',  ( 3.792298468851710069, -22.70151372599487871, -1.500000000000002220 ) ) ;
#43892 = EDGE_CURVE ( 'NONE', #50986, #50194, #34560, .T. ) ;
#43893 = PERSON_AND_ORGANIZATION ( #70597, #27821 ) ;
#43894 = CARTESIAN_POINT ( 'NONE',  ( 30.45304879119406039, -1.682774720514426114, -10.07140455160086390 ) ) ;
#43895 = LINE ( 'NONE', #45398, #15033 ) ;
#43896 = CARTESIAN_POINT ( 'NONE',  ( 9.271505649751263789, 17.87650053469100087, 11.49999999999999645 ) ) ;
#43897 = CARTESIAN_POINT ( 'NONE',  ( -108.9585383990916796, -25.10927658323717537, 4.038060707102717473 ) ) ;
#43898 = DIRECTION ( 'NONE',  ( -1.000000000000000000, -0.000000000000000000, -0.000000000000000000 ) ) ;
#43899 = LINE ( 'NONE', #4345, #16552 ) ;
#43900 = DIRECTION ( 'NONE',  ( 0.000000000000000000, 0.000000000000000000, -1.000000000000000000 ) ) ;
#43901 = CARTESIAN_POINT ( 'NONE',  ( -110.6372435692922664, -25.18425590734490171, 3.331084500688020977 ) ) ;
#43902 = CARTESIAN_POINT ( 'NONE',  ( -9.044204435542846809, 17.70297415775587169, -1.500000000000002220 ) ) ;
#43903 = DIRECTION ( 'NONE',  ( -1.000000000000000000, 0.000000000000000000, 0.000000000000000000 ) ) ;
#43904 = CARTESIAN_POINT ( 'NONE',  ( 13.37688099249405127, 14.58279310912311111, -1.500000000000002220 ) ) ;
#43905 = CARTESIAN_POINT ( 'NONE',  ( -126.5558601108541836, -23.96169478059714208, 10.65365249895716637 ) ) ;
#43906 = VECTOR ( 'NONE', #70824, 1000.000000000000114 ) ;
#43907 = DESIGN_CONTEXT ( 'detailed design', #23272, 'design' ) ;
#43908 = CARTESIAN_POINT ( 'NONE',  ( -1.012926118674504883, -6.376774720514415407, 19.92818918856637822 ) ) ;
#43909 = CARTESIAN_POINT ( 'NONE',  ( 2.905472630834636139, -6.376774720514415407, 19.87563926270137671 ) ) ;
#43910 = CARTESIAN_POINT ( 'NONE',  ( 6.115004186001010922, -19.73231167505474559, 11.49999999999999645 ) ) ;
#43911 = CARTESIAN_POINT ( 'NONE',  ( 20.57455539870795036, -2.682774720514426559, -18.22080502500658739 ) ) ;
#43912 = EDGE_CURVE ( 'NONE', #4511, #2525, #34372, .T. ) ;
#43913 = CARTESIAN_POINT ( 'NONE',  ( 31.73616390345410920, 3.909076239803030539, -3.851095480477756627 ) ) ;
#43914 = CARTESIAN_POINT ( 'NONE',  ( -63.52287095715004739, -23.47593901973090169, -1.443836447538996870 ) ) ;
#43915 = CARTESIAN_POINT ( 'NONE',  ( 22.31954755298990278, 3.869410565987296380, 11.49999999999999645 ) ) ;
#43916 = ORIENTED_EDGE ( 'NONE', *, *, #87470, .F. ) ;
#43917 = DIRECTION ( 'NONE',  ( -1.000000000000000000, -0.000000000000000000, -0.000000000000000000 ) ) ;
#43918 = CARTESIAN_POINT ( 'NONE',  ( 30.64109437917162637, 3.603390417177663174, 28.31981403122773955 ) ) ;
#43919 = FACE_OUTER_BOUND ( 'NONE', #70875, .T. ) ;
#43920 = B_SPLINE_CURVE_WITH_KNOTS ( 'NONE', 3,
 ( #40268, #7811, #14914, #71221 ),
 .UNSPECIFIED., .F., .F.,
 ( 4, 4 ),
 ( 0.000000000000000000, 9.999999999998897304E-05 ),
 .UNSPECIFIED. ) ;
#43921 = CARTESIAN_POINT ( 'NONE',  ( 29.80070917940689412, 5.965225279485572685, 27.39560796525321607 ) ) ;
#43922 = EDGE_CURVE ( 'NONE', #40589, #73004, #46601, .T. ) ;
#43923 = ORIENTED_EDGE ( 'NONE', *, *, #21236, .T. ) ;
#43924 = EDGE_LOOP ( 'NONE', ( #2686, #14526, #95868, #36551 ) ) ;
#43925 = CARTESIAN_POINT ( 'NONE',  ( 0.3849403830293018358, -6.376774720514418959, 20.45311193189268906 ) ) ;
#43926 = CARTESIAN_POINT ( 'NONE',  ( -21.74799678179195794, 7.114197580472080951, 11.49999999999998934 ) ) ;
#43927 = DIRECTION ( 'NONE',  ( -0.09824042138329623641, -2.980407940728110405E-17, 0.9951627101165078093 ) ) ;
#43928 = CARTESIAN_POINT ( 'NONE',  ( 18.62697458635512859, 10.92912097662538251, -1.500000000000002220 ) ) ;
#43929 = CARTESIAN_POINT ( 'NONE',  ( -113.5190789393543156, -23.96169478059713853, 10.65365249895717348 ) ) ;
#43930 = CARTESIAN_POINT ( 'NONE',  ( -76.58953762381673869, -23.48786465467241058, 11.44779295918254469 ) ) ;
#43931 = CARTESIAN_POINT ( 'NONE',  ( 1.525329354412473970, -22.51392980886878448, 11.49999999999999645 ) ) ;
#43932 = ORIENTED_EDGE ( 'NONE', *, *, #85743, .T. ) ;
#43933 = CARTESIAN_POINT ( 'NONE',  ( -28.60206680416888858, -24.93038538096085688, 2.636305656040084600 ) ) ;
#43934 = CARTESIAN_POINT ( 'NONE',  ( 16.16784302627978320, -14.93143893958281154, -1.500000000000002220 ) ) ;
#43935 = CARTESIAN_POINT ( 'NONE',  ( -9.299999999999991829, 12.00000000000002309, 2.100000000000000089 ) ) ;
#43936 = DIRECTION ( 'NONE',  ( 0.9951627101165076983, -0.09824042138329622254, 0.000000000000000000 ) ) ;
#43937 = ORIENTED_EDGE ( 'NONE', *, *, #60330, .F. ) ;
#43938 = PLANE ( 'NONE',  #99418 ) ;
#43939 = CARTESIAN_POINT ( 'NONE',  ( -90.50597553108265458, -24.52399227489126687, 9.353111116836531735 ) ) ;
#43940 = EDGE_LOOP ( 'NONE', ( #82474, #83482, #16544, #33455 ) ) ;
#43941 = CARTESIAN_POINT ( 'NONE',  ( -29.52287095715006515, -23.65290397102212339, -1.053491145022395603 ) ) ;
#43942 = EDGE_LOOP ( 'NONE', ( #24558, #79510, #18753, #56880 ) ) ;
#43943 = ORIENTED_EDGE ( 'NONE', *, *, #4984, .T. ) ;
#43944 = ADVANCED_FACE ( 'NONE', ( #9306 ), #70719, .F. ) ;
#43945 = CARTESIAN_POINT ( 'NONE',  ( -65.52287095715007581, -24.14321612903117042, -0.2833117244521693445 ) ) ;
#43946 = DIRECTION ( 'NONE',  ( 0.000000000000000000, 0.000000000000000000, -1.000000000000000000 ) ) ;
#43947 = CARTESIAN_POINT ( 'NONE',  ( -36.60922706349395384, -23.73766607897670156, -1.055555164236459120 ) ) ;
#43948 = CARTESIAN_POINT ( 'NONE',  ( -12.60687543931603471, -16.05746371069360379, -1.500000000000002220 ) ) ;
#43949 = ORIENTED_EDGE ( 'NONE', *, *, #2028, .T. ) ;
#43950 = CARTESIAN_POINT ( 'NONE',  ( -3.095730855174848362, -6.376774720514413630, 20.04377961306771638 ) ) ;
#43951 = PLANE ( 'NONE',  #74123 ) ;
#43952 = CARTESIAN_POINT ( 'NONE',  ( -105.6251635957058710, -24.83618233451450408, 1.606449574219534826 ) ) ;
#43953 = DIRECTION ( 'NONE',  ( 3.773278334444167608E-23, -1.000000000000000000, 0.000000000000000000 ) ) ;
#43954 = ORIENTED_EDGE ( 'NONE', *, *, #11130, .F. ) ;
#43955 = CYLINDRICAL_SURFACE ( 'NONE', #20854, 12.65241003308275758 ) ;
#43956 = CARTESIAN_POINT ( 'NONE',  ( -90.52287095715006160, -23.47593901973090524, -1.443836447538996426 ) ) ;
#43957 = B_SPLINE_CURVE_WITH_KNOTS ( 'NONE', 3,
 ( #28097, #30076, #15346, #53435 ),
 .UNSPECIFIED., .F., .F.,
 ( 4, 4 ),
 ( 2.163172446012162672E-11, 0.001212141367717853692 ),
 .UNSPECIFIED. ) ;
#43958 = CARTESIAN_POINT ( 'NONE',  ( 19.92439739378097840, -5.974006126113303949, 11.49999999999998934 ) ) ;
#43959 = CIRCLE ( 'NONE', #97408, 1.306876713926001354 ) ;
#43960 = EDGE_CURVE ( 'NONE', #21736, #88376, #39197, .T. ) ;
#43961 = VERTEX_POINT ( 'NONE', #50890 ) ;
#43963 = ORIENTED_EDGE ( 'NONE', *, *, #60257, .F. ) ;
#43962 = CARTESIAN_POINT ( 'NONE',  ( -65.05438548721848235, 5.356774720514425603, 0.7300228001186309656 ) ) ;
#43964 = EDGE_CURVE ( 'NONE', #20017, #57039, #50693, .T. ) ;
#43965 = CARTESIAN_POINT ( 'NONE',  ( -28.62287095715004881, -23.57201582636175274, 11.05761041841422454 ) ) ;
#43966 = LINE ( 'NONE', #38704, #6531 ) ;
#43967 = ORIENTED_EDGE ( 'NONE', *, *, #81227, .F. ) ;
#43968 = ORIENTED_EDGE ( 'NONE', *, *, #9000, .T. ) ;
#43969 = DIRECTION ( 'NONE',  ( -0.000000000000000000, 2.173523156925979552E-06, -0.9999999999976378895 ) ) ;
#43970 = CARTESIAN_POINT ( 'NONE',  ( 13.87573923102662121, -3.316774720514425123, -28.27006591627376508 ) ) ;
#43971 = DIRECTION ( 'NONE',  ( 0.000000000000000000, 0.9999999999976377785, 2.173523156925979128E-06 ) ) ;
#43972 = CARTESIAN_POINT ( 'NONE',  ( -71.24017339641436308, -25.24515161739355307, 5.863458295308564772 ) ) ;
#43974 = VERTEX_POINT ( 'NONE', #18923 ) ;
#43973 = CARTESIAN_POINT ( 'NONE',  ( 9.107982344273736430, -20.20341329189913537, 11.49999999999999645 ) ) ;
#43975 = EDGE_CURVE ( 'NONE', #20665, #22695, #98500, .T. ) ;
#43976 = CARTESIAN_POINT ( 'NONE',  ( -108.5148114596531599, -24.34968618360934656, 0.1864209137778971292 ) ) ;
#43977 = CARTESIAN_POINT ( 'NONE',  ( 21.37280783159109276, 7.349196219051140844, 11.49999999999998934 ) ) ;
#43978 = EDGE_CURVE ( 'NONE', #38350, #91631, #42784, .T. ) ;
#43980 = ORIENTED_EDGE ( 'NONE', *, *, #72599, .T. ) ;
#43979 = CARTESIAN_POINT ( 'NONE',  ( -115.6235241362618069, -25.00182538069147142, 7.747789668545041586 ) ) ;
#43981 = AXIS2_PLACEMENT_3D ( 'NONE', #90304, #13166, #20774 ) ;
#43982 = ORIENTED_EDGE ( 'NONE', *, *, #62068, .F. ) ;
#43983 = CARTESIAN_POINT ( 'NONE',  ( -31.62287095715005236, -23.48786465467240347, 11.44779295918255180 ) ) ;
#43984 = CYLINDRICAL_SURFACE ( 'NONE', #87833, 130.7884398600581335 ) ;
#43985 = VERTEX_POINT ( 'NONE', #73229 ) ;
#43986 = CARTESIAN_POINT ( 'NONE',  ( -24.90875734969025501, 6.376774720514426953, 26.43402280011862615 ) ) ;
#43987 = CARTESIAN_POINT ( 'NONE',  ( 5.670930919660429836, -21.52877996283707418, -1.500000000000002220 ) ) ;
#43988 = CARTESIAN_POINT ( 'NONE',  ( -50.04527796557857755, -25.13941491172449005, 7.536031268920055481 ) ) ;
#43989 = EDGE_LOOP ( 'NONE', ( #48318, #11968, #82494, #100415 ) ) ;
#43990 = CARTESIAN_POINT ( 'NONE',  ( -78.58953762381672448, -23.47593901973091235, -1.443836447539004642 ) ) ;
#43991 = CARTESIAN_POINT ( 'NONE',  ( -80.68466099729241137, -25.03432220282478937, 7.556350509324876619 ) ) ;
#43992 = CARTESIAN_POINT ( 'NONE',  ( 27.53860345374808105, -5.356774720496559894, 0.000000000000000000 ) ) ;
#43993 = CARTESIAN_POINT ( 'NONE',  ( -0.02075734969026423599, 5.965225279485572685, -29.05397719988136984 ) ) ;
#43994 = DIRECTION ( 'NONE',  ( 0.000000000000000000, -1.000000000000000000, 0.000000000000000000 ) ) ;
#43995 = CARTESIAN_POINT ( 'NONE',  ( 16.96702763494397104, -9.608290155750392358, 11.49999999999998934 ) ) ;
#43996 = CARTESIAN_POINT ( 'NONE',  ( -21.47443924280258187, -0.1944818460393343829, 11.49999999999998934 ) ) ;
#43997 = CARTESIAN_POINT ( 'NONE',  ( -2.457093156980370452, -5.876774720514410077, 19.51167604195716976 ) ) ;
#43998 = PLANE ( 'NONE',  #68175 ) ;
#43999 = CARTESIAN_POINT ( 'NONE',  ( -9.940598223437573822, -5.876774720514426953, 21.78128695274315874 ) ) ;
#44000 = CARTESIAN_POINT ( 'NONE',  ( -12.33899560737860313, 19.21699747222852395, -1.500000000000002220 ) ) ;
#44001 = PERSON ( 'NAUO-PER6', 'UNSPECIFIED', 'UNSPECIFIED', ('UNSPECIFIED'), ('UNSPECIFIED'), ('UNSPECIFIED') ) ;
#44002 = ADVANCED_FACE ( 'NONE', ( #96550 ), #48895, .T. ) ;
#44003 = AXIS2_PLACEMENT_3D ( 'NONE', #8401, #47474, #53601 ) ;
#44004 = DATE_AND_TIME ( #99279, #69977 ) ;
#44005 = CARTESIAN_POINT ( 'NONE',  ( -106.5533739365583585, -24.15620529776629510, 10.23563542870659582 ) ) ;
#44006 = CARTESIAN_POINT ( 'NONE',  ( -125.5562042904833930, -23.48783264082479150, -1.443836473390055941 ) ) ;
#44007 = CARTESIAN_POINT ( 'NONE',  ( 12.75013301566243129, -15.34773647900153115, 11.49999999999999645 ) ) ;
#44008 = CARTESIAN_POINT ( 'NONE',  ( -5.366453405989236813, 0.000000000000000000, 0.000000000000000000 ) ) ;
#44010 = B_SPLINE_CURVE_WITH_KNOTS ( 'NONE', 3,
 ( #27571, #81847, #5219, #58522, #75710, #89463 ),
 .UNSPECIFIED., .F., .F.,
 ( 4, 2, 4 ),
 ( 1.570887131794638196E-05, 0.001396322306279758904, 0.002776935741241571502 ),
 .UNSPECIFIED. ) ;
#44009 = CARTESIAN_POINT ( 'NONE',  ( -74.58799468583525538, -24.35071581493544102, 9.817618358456019934 ) ) ;
#44011 = FACE_OUTER_BOUND ( 'NONE', #96210, .T. ) ;
#44012 = ORIENTED_EDGE ( 'NONE', *, *, #45929, .T. ) ;
#44013 = CARTESIAN_POINT ( 'NONE',  ( -27.33385579971651325, -24.59579688747963289, 1.660712602240671298 ) ) ;
#44014 = CARTESIAN_POINT ( 'NONE',  ( -65.52287095715006160, -25.00182538069144655, 7.747789668545101982 ) ) ;
#44015 = CARTESIAN_POINT ( 'NONE',  ( 15.89274262425319861, 14.76810421718133171, -1.500000000000002220 ) ) ;
#44016 = CARTESIAN_POINT ( 'NONE',  ( -37.52287095715006870, -23.47593901973090524, -1.443836447538997314 ) ) ;
#44017 = CARTESIAN_POINT ( 'NONE',  ( 19.54226456527178257, 0.3027743077981833730, -1.500000000000002220 ) ) ;
#44018 = DIRECTION ( 'NONE',  ( -3.773278334453079618E-23, 0.9999999999976377785, 2.173523156925979975E-06 ) ) ;
#44019 = ORIENTED_EDGE ( 'NONE', *, *, #36833, .T. ) ;
#44020 = DIRECTION ( 'NONE',  ( -3.773278334444167608E-23, 1.000000000000000000, 0.000000000000000000 ) ) ;
#44021 = CARTESIAN_POINT ( 'NONE',  ( -110.6228709571500559, -25.00158670708909625, 2.256160236439165967 ) ) ;
#44022 = CARTESIAN_POINT ( 'NONE',  ( -2.888065500968368227, -20.30684875360264741, 11.49999999999999645 ) ) ;
#44023 = LINE ( 'NONE', #26809, #19688 ) ;
#44024 = VECTOR ( 'NONE', #55761, 999.9999999999998863 ) ;
#44025 = B_SPLINE_CURVE_WITH_KNOTS ( 'NONE', 3,
 ( #53106, #14516, #38359, #45986 ),
 .UNSPECIFIED., .F., .F.,
 ( 4, 4 ),
 ( 0.000000000000000000, 9.999999999998897304E-05 ),
 .UNSPECIFIED. ) ;
#44026 = DIRECTION ( 'NONE',  ( -0.000000000000000000, 2.173523156925979552E-06, -0.9999999999976378895 ) ) ;
#44027 = B_SPLINE_CURVE_WITH_KNOTS ( 'NONE', 3,
 ( #54070, #47444, #48450, #40822, #32708, #260, #78372, #33211, #38819, #93597, #92601, #77868, #78868, #71785, #55564, #24090 ),
 .UNSPECIFIED., .F., .F.,
 ( 4, 2, 2, 2, 2, 2, 2, 4 ),
 ( 1.734723475976807094E-18, 0.0002333606573560949337, 0.0004667213147121881327, 0.0007000819720682813045, 0.0009334426294243745306, 0.001166803286780467757, 0.001400163944136560874, 0.001866885258848787876 ),
 .UNSPECIFIED. ) ;
#44028 = EDGE_CURVE ( 'NONE', #48067, #55188, #40487, .T. ) ;
#44029 = ORIENTED_EDGE ( 'NONE', *, *, #41819, .F. ) ;
#44030 = LINE ( 'NONE', #22172, #39481 ) ;
#44031 = CARTESIAN_POINT ( 'NONE',  ( -106.6228709571500559, -24.64965695001469115, 8.947790433994176951 ) ) ;
#44032 = ADVANCED_FACE ( 'NONE', ( #58014 ), #79821, .F. ) ;
#44033 = DIRECTION ( 'NONE',  ( 0.000000000000000000, 0.000000000000000000, -1.000000000000000000 ) ) ;
#44034 = SHAPE_REPRESENTATION ( 'Plastic Part 1', ( #37391 ), #11455 ) ;
#44035 = CARTESIAN_POINT ( 'NONE',  ( -123.5228709571500900, -23.72773821059536914, 11.05748984161097148 ) ) ;
#44036 = VERTEX_POINT ( 'NONE', #81333 ) ;
#44037 = DIRECTION ( 'NONE',  ( 0.000000000000000000, 2.173523156925980399E-06, -0.9999999999976378895 ) ) ;
#44038 = ADVANCED_FACE ( 'NONE', ( #3721 ), #18431, .T. ) ;
#44039 = EDGE_CURVE ( 'NONE', #16877, #44339, #41790, .T. ) ;
#44040 = AXIS2_PLACEMENT_3D ( 'NONE', #90321, #13682, #67006 ) ;
#44041 = CARTESIAN_POINT ( 'NONE',  ( 20.04565040668967413, 11.27863464804978477, 11.49999999999999645 ) ) ;
#44042 = CARTESIAN_POINT ( 'NONE',  ( -12.29745307268338195, -19.16510367807413218, -1.500000000000002220 ) ) ;
#44043 = CARTESIAN_POINT ( 'NONE',  ( 10.34999999999999432, 12.00000000000002309, 0.000000000000000000 ) ) ;
#44044 = CARTESIAN_POINT ( 'NONE',  ( 8.071512145086501278, -1.028487854913507915, -3.750000000000000444 ) ) ;
#44045 = CARTESIAN_POINT ( 'NONE',  ( -58.87764846858842560, -25.13069340115296058, 2.947789388436138580 ) ) ;
#44047 = ADVANCED_FACE ( 'NONE', ( #65634 ), #11814, .T. ) ;
#44046 = CC_DESIGN_APPROVAL ( #45738, ( #14113 ) ) ;
#44048 = DIRECTION ( 'NONE',  ( 0.000000000000000000, 0.000000000000000000, 1.000000000000000000 ) ) ;
#44049 = CARTESIAN_POINT ( 'NONE',  ( -69.58953762381671027, -24.64898659630528854, 1.056161002820825034 ) ) ;
#44050 = CARTESIAN_POINT ( 'NONE',  ( 21.48171311866277122, -4.276277801222842179, 11.49999999999998934 ) ) ;
#44051 = DIRECTION ( 'NONE',  ( -1.000000000000000000, -0.000000000000000000, 0.000000000000000000 ) ) ;
#44052 = CARTESIAN_POINT ( 'NONE',  ( -34.55620429048339304, -24.66019654487199020, 8.947790411086138818 ) ) ;
#44053 = CARTESIAN_POINT ( 'NONE',  ( -50.37830952628071657, -29.50249428492551829, 5.197779886230994073 ) ) ;
#44054 = CARTESIAN_POINT ( 'NONE',  ( -24.90875734969025501, -0.3587747205144265483, 26.43402280011862615 ) ) ;
#44055 = CARTESIAN_POINT ( 'NONE',  ( -58.58751465073510900, -24.34968618360933945, 0.1864209137778795045 ) ) ;
#44056 = VERTEX_POINT ( 'NONE', #66135 ) ;
#44057 = CARTESIAN_POINT ( 'NONE',  ( 13.31029742451639386, -15.53102932315203510, -1.500000000000002220 ) ) ;
#44058 = VERTEX_POINT ( 'NONE', #12301 ) ;
#44059 = EDGE_LOOP ( 'NONE', ( #2795, #87253, #48599, #76999 ) ) ;
#44060 = ORIENTED_EDGE ( 'NONE', *, *, #38135, .F. ) ;
#44061 = ORIENTED_EDGE ( 'NONE', *, *, #42140, .F. ) ;
#44062 = ADVANCED_FACE ( 'NONE', ( #33150 ), #58508, .F. ) ;
#44063 = CARTESIAN_POINT ( 'NONE',  ( -7.156825135384894843, 21.90021990432103038, 11.49999999999998934 ) ) ;
#44064 = PLANE ( 'NONE',  #32460 ) ;
#44065 = CARTESIAN_POINT ( 'NONE',  ( 3.949161919925879172, -19.86910077469890723, -1.500000000000002220 ) ) ;
#44066 = ORIENTED_EDGE ( 'NONE', *, *, #65048, .F. ) ;
#44067 = CARTESIAN_POINT ( 'NONE',  ( -77.62287095715005592, -29.50250243563736774, 8.947779886222141599 ) ) ;
#44068 = DIRECTION ( 'NONE',  ( -7.960204194457801640E-17, -1.000000000000000000, 0.000000000000000000 ) ) ;
#44069 = B_SPLINE_CURVE_WITH_KNOTS ( 'NONE', 3,
 ( #78241, #56445, #1141, #63055 ),
 .UNSPECIFIED., .F., .F.,
 ( 4, 4 ),
 ( 0.000000000000000000, 9.999999999998900014E-05 ),
 .UNSPECIFIED. ) ;
#44070 = B_SPLINE_CURVE_WITH_KNOTS ( 'NONE', 3,
 ( #24918, #40154, #71110, #1599, #31029, #61994 ),
 .UNSPECIFIED., .F., .F.,
 ( 4, 2, 4 ),
 ( 0.000000000000000000, 0.001380901958385381606, 0.002761803916770763211 ),
 .UNSPECIFIED. ) ;
#44071 = CARTESIAN_POINT ( 'NONE',  ( -95.54721046836138498, -24.63355581998386157, 0.9682620441943944334 ) ) ;
#44072 = CARTESIAN_POINT ( 'NONE',  ( -102.5228709571500758, -23.48786465467241769, 11.44779295918254114 ) ) ;
#44074 = VERTEX_POINT ( 'NONE', #26039 ) ;
#44073 = CARTESIAN_POINT ( 'NONE',  ( -0.4629837013611828866, -21.40787533109759977, 11.49999999999999645 ) ) ;
#44075 = CARTESIAN_POINT ( 'NONE',  ( 0.000000000000000000, 0.3849999999999945688, 1.530000000000001359 ) ) ;
#44076 = ORIENTED_EDGE ( 'NONE', *, *, #33647, .F. ) ;
#44077 = CARTESIAN_POINT ( 'NONE',  ( 21.15429367616652101, -6.912965584596229895, 11.49999999999998934 ) ) ;
#44078 = CARTESIAN_POINT ( 'NONE',  ( 7.508984785159893427, -19.29828013722326929, 11.49999999999998934 ) ) ;
#44079 = EDGE_CURVE ( 'NONE', #93291, #94756, #90080, .T. ) ;
#44080 = ORIENTED_EDGE ( 'NONE', *, *, #30052, .F. ) ;
#44081 = VECTOR ( 'NONE', #5917, 1000.000000000000227 ) ;
#44082 = B_SPLINE_SURFACE_WITH_KNOTS ( 'NONE', 3, 1, ( 
 ( #38220, #45847 ),
 ( #21985, #76766 ),
 ( #90517, #82896 ),
 ( #22481, #29114 ),
 ( #75779, #13381 ),
 ( #13882, #22976 ),
 ( #44361, #91013 ),
 ( #83397, #7266 ),
 ( #69176, #75285 ),
 ( #53471, #60590 ),
 ( #100096, #44856 ),
 ( #6278, #36735 ),
 ( #77271, #99114 ),
 ( #53966, #67703 ),
 ( #37236, #92505 ) ),
 .UNSPECIFIED., .F., .F., .F.,
 ( 4, 1, 1, 1, 1, 1, 1, 1, 1, 1, 1, 1, 4 ),
 ( 2, 2 ),
 ( 0.000000000000000000, 0.09781818961471398788, 0.1997260534018261702, 0.3052763574779416844, 0.4158114905382919169, 0.4744722311435584650, 0.5372738797760969742, 0.6036574205596554332, 0.6742988630901268765, 0.7498344853162316470, 0.8285984767571028531, 0.9123777781577806500, 1.000000000000000000 ),
 ( 0.000000000000000000, 1.000000000000000000 ),
 .UNSPECIFIED. ) ;
#44083 = EDGE_CURVE ( 'NONE', #24828, #76130, #22302, .T. ) ;
#44084 = CARTESIAN_POINT ( 'NONE',  ( -28.67151963337447285, -23.33523189894360073, -1.443835813551990865 ) ) ;
#44085 = ORIENTED_EDGE ( 'NONE', *, *, #39920, .F. ) ;
#44086 = CARTESIAN_POINT ( 'NONE',  ( 0.000000000000000000, -4.056774720514426669, 0.000000000000000000 ) ) ;
#44087 = ORIENTED_EDGE ( 'NONE', *, *, #54912, .T. ) ;
#44088 = CARTESIAN_POINT ( 'NONE',  ( -12.67655569012464944, 16.65582705476778358, -1.500000000000002220 ) ) ;
#44089 = CARTESIAN_POINT ( 'NONE',  ( 21.92589416912191069, -1.073809401359021143, 11.49999999999999645 ) ) ;
#44090 = EDGE_CURVE ( 'NONE', #21186, #57878, #58635, .T. ) ;
#44091 = CARTESIAN_POINT ( 'NONE',  ( -37.57004739008115024, -23.48786465467240347, 11.44779295918255357 ) ) ;
#44092 = CARTESIAN_POINT ( 'NONE',  ( -6.671648801611133273, 21.52854475820963032, 11.49999999999998934 ) ) ;
#44093 = CARTESIAN_POINT ( 'NONE',  ( -20.97355972163249049, 0.1317905507124840780, 11.49999999999998934 ) ) ;
#44094 = ADVANCED_FACE ( 'NONE', ( #37147 ), #5200, .F. ) ;
#44095 = DIRECTION ( 'NONE',  ( 0.000000000000000000, 0.000000000000000000, -1.000000000000000000 ) ) ;
#44096 = CARTESIAN_POINT ( 'NONE',  ( -119.5539580184925796, -24.35071581493544457, 9.817618358456018157 ) ) ;
#44097 = CARTESIAN_POINT ( 'NONE',  ( 8.071512145086503054, -0.8690767389352458405, -3.741933809627420171 ) ) ;
#44098 = ORIENTED_EDGE ( 'NONE', *, *, #2457, .T. ) ;
#44099 = EDGE_CURVE ( 'NONE', #55534, #294, #23557, .T. ) ;
#44100 = ORIENTED_EDGE ( 'NONE', *, *, #50639, .F. ) ;
#44101 = VERTEX_POINT ( 'NONE', #74702 ) ;
#44102 = VECTOR ( 'NONE', #32041, 1000.000000000000000 ) ;
#44103 = CARTESIAN_POINT ( 'NONE',  ( -128.6228709571500417, -23.73934037231758509, 11.05740245334327554 ) ) ;
#44104 = CARTESIAN_POINT ( 'NONE',  ( -13.16228656746626591, 16.97819584282690286, -1.500000000000002220 ) ) ;
#44105 = B_SPLINE_CURVE_WITH_KNOTS ( 'NONE', 3,
 ( #95114, #10374, #34225, #86996, #40331, #18983 ),
 .UNSPECIFIED., .F., .F.,
 ( 4, 2, 4 ),
 ( 0.000000000000000000, 0.001380901958385388545, 0.002761803916770777089 ),
 .UNSPECIFIED. ) ;
#44106 = EDGE_CURVE ( 'NONE', #1512, #95782, #76197, .T. ) ;
#44107 = FACE_OUTER_BOUND ( 'NONE', #76366, .T. ) ;
#44108 = ORIENTED_EDGE ( 'NONE', *, *, #45465, .T. ) ;
#44109 = CARTESIAN_POINT ( 'NONE',  ( -13.65698368949537311, 16.12507722524849996, -1.500000000000002220 ) ) ;
#44110 = CARTESIAN_POINT ( 'NONE',  ( 13.91401389203221406, -6.475225279485573360, 27.24920385068457662 ) ) ;
#44111 = B_SPLINE_CURVE_WITH_KNOTS ( 'NONE', 3,
 ( #25907, #4581, #96919, #65999, #57385, #81194, #65499, #26908, #33520, #57879, #11671, #19283, #19778, #56881, #37015, #44631, #45139, #13163, #6565, #59867, #20274, #58860, #6059 ),
 .UNSPECIFIED., .F., .F.,
 ( 4, 1, 1, 1, 1, 1, 1, 1, 1, 1, 1, 1, 1, 1, 1, 1, 1, 1, 1, 1, 4 ),
 ( 0.000000000000000000, 0.07295106587586808189, 0.1415836941865457888, 0.2059264601708682696, 0.2653013571846069008, 0.3205972327139294809, 0.3718165030988108688, 0.4187897697094533633, 0.4616987286157644976, 0.5021335821035667335, 0.5408043152926478303, 0.5781805253279665990, 0.6142968652075149194, 0.6496782432647882910, 0.6842994600896379342, 0.7183589527723613921, 0.7520808646475963810, 0.8176524386023853452, 0.8797220764054369813, 0.9399655597309874988, 1.000000000000000000 ),
 .UNSPECIFIED. ) ;
#44112 = DIRECTION ( 'NONE',  ( -0.000000000000000000, -1.000000000000000000, 0.000000000000000000 ) ) ;
#44113 = CARTESIAN_POINT ( 'NONE',  ( -83.62359973981459405, -24.66019654487199375, 8.947790411086124607 ) ) ;
#44114 = CARTESIAN_POINT ( 'NONE',  ( 9.016989526679575206, -6.475225279485574248, -27.05137190084761301 ) ) ;
#44115 = CARTESIAN_POINT ( 'NONE',  ( -1.267404104715736279, -5.876774720514411854, 19.66076420632889921 ) ) ;
#44116 = CARTESIAN_POINT ( 'NONE',  ( -18.93877658415168241, -11.43451605920036052, -1.500000000000002220 ) ) ;
#44117 = DIRECTION ( 'NONE',  ( 0.000000000000000000, 0.000000000000000000, 1.000000000000000000 ) ) ;
#44118 = B_SPLINE_CURVE_WITH_KNOTS ( 'NONE', 3,
 ( #48374, #79303, #73700, #4194, #13282, #89427, #6177, #44753, #36137, #19899 ),
 .UNSPECIFIED., .F., .F.,
 ( 4, 2, 2, 2, 4 ),
 ( 0.000000000000000000, 0.0002770619399313387575, 0.0005541238798626775151, 0.0008311858197940162184, 0.001108247759725355030 ),
 .UNSPECIFIED. ) ;
#44119 = CARTESIAN_POINT ( 'NONE',  ( -109.7567281351150541, -25.28788469920083770, 5.668544159025581841 ) ) ;
#44120 = CARTESIAN_POINT ( 'NONE',  ( 11.94353453780502683, 5.048182838635504766, -26.89061828217040784 ) ) ;
#44121 = DIRECTION ( 'NONE',  ( 0.000000000000000000, 0.000000000000000000, -1.000000000000000000 ) ) ;
#44122 = PLANE ( 'NONE',  #9025 ) ;
#44123 = VECTOR ( 'NONE', #21179, 1000.000000000000000 ) ;
#44124 = CARTESIAN_POINT ( 'NONE',  ( -10.03281922573575002, -16.61734169602722488, 11.49999999999998934 ) ) ;
#44125 = APPROVAL_PERSON_ORGANIZATION ( #89442, #82276, #66630 ) ;
#44126 = CARTESIAN_POINT ( 'NONE',  ( 16.79701800048795590, -13.18750964578662455, -1.500000000000002220 ) ) ;
#44127 = LINE ( 'NONE', #13652, #27200 ) ;
#44128 = CARTESIAN_POINT ( 'NONE',  ( -90.70839235003093393, -25.31768024997816013, 4.634761245912265792 ) ) ;
#44129 = PLANE ( 'NONE',  #95700 ) ;
#44131 = B_SPLINE_CURVE_WITH_KNOTS ( 'NONE', 3,
 ( #36361, #28245, #19126, #81039, #65837, #5409 ),
 .UNSPECIFIED., .F., .F.,
 ( 4, 2, 4 ),
 ( 0.000000000000000000, 0.001380764517854763665, 0.002761529035709527329 ),
 .UNSPECIFIED. ) ;
#44130 = CARTESIAN_POINT ( 'NONE',  ( -100.4326965455115186, -25.27359974593377956, 3.293942923980552884 ) ) ;
#44132 = CARTESIAN_POINT ( 'NONE',  ( 10.43192878459595185, 20.09917060401269850, -1.500000000000002220 ) ) ;
#44133 = ORIENTED_EDGE ( 'NONE', *, *, #50464, .F. ) ;
#44134 = DIRECTION ( 'NONE',  ( 0.000000000000000000, 0.000000000000000000, 1.000000000000000000 ) ) ;
#44135 = CARTESIAN_POINT ( 'NONE',  ( -79.54658045552653789, -24.34968618360933945, 0.1864209137778814473 ) ) ;
#44136 = CARTESIAN_POINT ( 'NONE',  ( -19.81728208556213389, 0.3677575464312098363, 11.49999999999999645 ) ) ;
#44137 = CARTESIAN_POINT ( 'NONE',  ( -5.891025641025639636, -6.376774720514420736, 20.75510817307693046 ) ) ;
#44138 = CARTESIAN_POINT ( 'NONE',  ( -119.5228709571501611, -23.96127896941633040, -0.6493128931037963625 ) ) ;
#44139 = ORIENTED_EDGE ( 'NONE', *, *, #55984, .T. ) ;
#44140 = CARTESIAN_POINT ( 'NONE',  ( -77.52287095715006160, -24.64898659630367916, 1.056161002820826145 ) ) ;
#44141 = CARTESIAN_POINT ( 'NONE',  ( -28.67105337545913812, -24.60093948885277015, 1.897772093073314181 ) ) ;
#44142 = CARTESIAN_POINT ( 'NONE',  ( -100.4799102492508780, -25.12268565644366447, 7.101073848355138551 ) ) ;
#44143 = CARTESIAN_POINT ( 'NONE',  ( -21.62496174240652991, 0.2022338437372764308, -1.500000000000002220 ) ) ;
#44144 = CARTESIAN_POINT ( 'NONE',  ( -49.10457154551148307, -25.10935380766095193, 3.999772607897646548 ) ) ;
#44145 = CARTESIAN_POINT ( 'NONE',  ( -18.22047185089115828, 6.579378235550767506, -1.500000000000002220 ) ) ;
#44146 = CARTESIAN_POINT ( 'NONE',  ( 32.53135143123563466, -5.965225279485572685, 6.926385399448451885 ) ) ;
#44147 = LINE ( 'NONE', #52757, #73396 ) ;
#44148 = CARTESIAN_POINT ( 'NONE',  ( -17.91562471463183570, -8.470225615102204841, -1.500000000000002220 ) ) ;
#44149 = ORIENTED_EDGE ( 'NONE', *, *, #290, .T. ) ;
#44150 = CARTESIAN_POINT ( 'NONE',  ( -8.335131950130996614, 18.48905954037022781, 11.49999999999999645 ) ) ;
#44151 = CARTESIAN_POINT ( 'NONE',  ( -54.58953762381672448, -24.66019654487199020, 8.947790411086131712 ) ) ;
#44153 = AXIS2_PLACEMENT_3D ( 'NONE', #2579, #86300, #87299 ) ;
#44152 = FACE_OUTER_BOUND ( 'NONE', #14444, .T. ) ;
#44154 = EDGE_CURVE ( 'NONE', #47480, #53349, #5430, .T. ) ;
#44155 = VERTEX_POINT ( 'NONE', #75205 ) ;
#44156 = FACE_OUTER_BOUND ( 'NONE', #75012, .T. ) ;
#44157 = CARTESIAN_POINT ( 'NONE',  ( 31.63608488009066733, 3.316774720514426456, 27.34773273846990094 ) ) ;
#44158 = FACE_OUTER_BOUND ( 'NONE', #72321, .T. ) ;
#44159 = EDGE_CURVE ( 'NONE', #34973, #27382, #37647, .T. ) ;
#44160 = CARTESIAN_POINT ( 'NONE',  ( -6.660000000000001030, -2.191226316053958875E-18, 2.701633758479787833E-17 ) ) ;
#44161 = CARTESIAN_POINT ( 'NONE',  ( -51.51966037441169277, -25.23394976452496152, 6.321922888134675844 ) ) ;
#44162 = CARTESIAN_POINT ( 'NONE',  ( -13.75281105048956576, 14.62798779934380811, 11.49999999999998934 ) ) ;
#44163 = EDGE_CURVE ( 'NONE', #60109, #44429, #82815, .T. ) ;
#44164 = CARTESIAN_POINT ( 'NONE',  ( -85.52287095715010423, -23.84047902841604127, -0.8780736468305390119 ) ) ;
#44165 = ORIENTED_EDGE ( 'NONE', *, *, #76324, .T. ) ;
#44166 = EDGE_CURVE ( 'NONE', #15254, #51264, #22402, .T. ) ;
#44167 = EDGE_CURVE ( 'NONE', #78612, #56245, #10201, .T. ) ;
#44168 = CARTESIAN_POINT ( 'NONE',  ( 21.82588152991271713, 6.770963248321698380, 11.49999999999999645 ) ) ;
#44169 = CARTESIAN_POINT ( 'NONE',  ( -49.53524246831344868, -25.26258762038820294, 4.168640273188112921 ) ) ;
#44170 = VECTOR ( 'NONE', #39536, 1000.000000000000000 ) ;
#44171 = CARTESIAN_POINT ( 'NONE',  ( -86.62287095715008434, -23.94994826722515668, -0.6494450866351706431 ) ) ;
#44172 = CARTESIAN_POINT ( 'NONE',  ( -5.366453405989236813, 0.000000000000000000, 6.099999999999999645 ) ) ;
#44173 = EDGE_CURVE ( 'NONE', #83609, #11601, #12799, .T. ) ;
#44174 = CARTESIAN_POINT ( 'NONE',  ( 6.403846153846157740, -5.876774720514425177, 21.48076923076922995 ) ) ;
#44175 = PLANE ( 'NONE',  #2500 ) ;
#44176 = CARTESIAN_POINT ( 'NONE',  ( 10.13505985054399083, -19.98934331558005439, 11.49999999999999645 ) ) ;
#44177 = DIRECTION ( 'NONE',  ( -3.773278334453079618E-23, 0.9999999999976377785, 2.173523156925979975E-06 ) ) ;
#44178 = ORIENTED_EDGE ( 'NONE', *, *, #66219, .T. ) ;
#44179 = CARTESIAN_POINT ( 'NONE',  ( -5.548086588741434788, -19.59138962566686004, 11.49999999999998934 ) ) ;
#44180 = ORIENTED_EDGE ( 'NONE', *, *, #49670, .T. ) ;
#44181 = EDGE_CURVE ( 'NONE', #72922, #7606, #76742, .T. ) ;
#44182 = CARTESIAN_POINT ( 'NONE',  ( 17.95915693031428262, 14.28781372813260120, -1.500000000000002220 ) ) ;
#44183 = CARTESIAN_POINT ( 'NONE',  ( -53.52287095715005449, -24.66019654487198665, 8.947790411086121054 ) ) ;
#44184 = ORIENTED_EDGE ( 'NONE', *, *, #75058, .T. ) ;
#44185 = CARTESIAN_POINT ( 'NONE',  ( 9.150000000000000355, -5.876774720514426953, -15.70000000000000284 ) ) ;
#44186 = CARTESIAN_POINT ( 'NONE',  ( -77.53982194047173948, -24.66019654487200441, 8.947790411086108620 ) ) ;
#44187 = VECTOR ( 'NONE', #81201, 1000.000000000000114 ) ;
#44188 = EDGE_CURVE ( 'NONE', #55530, #2529, #93651, .T. ) ;
#44189 = DIRECTION ( 'NONE',  ( -3.773278334453079030E-23, 0.9999999999976377785, 2.173523156925979128E-06 ) ) ;
#44191 = ORIENTED_EDGE ( 'NONE', *, *, #64581, .F. ) ;
#44190 = CARTESIAN_POINT ( 'NONE',  ( -3.247986963444697395, 20.98610878802851332, 11.49999999999999645 ) ) ;
#44192 = SECURITY_CLASSIFICATION ( '', '', #13060 ) ;
#44193 = EDGE_LOOP ( 'NONE', ( #28478, #3939, #61868, #99485 ) ) ;
#44194 = CARTESIAN_POINT ( 'NONE',  ( -22.11311035156252558, 1.696007508605793301, -1.500000000000002220 ) ) ;
#44195 = CARTESIAN_POINT ( 'NONE',  ( -20.25002411749221665, -3.895867502427604379, -1.500000000000002220 ) ) ;
#44196 = EDGE_CURVE ( 'NONE', #420, #16998, #7696, .T. ) ;
#44197 = B_SPLINE_CURVE_WITH_KNOTS ( 'NONE', 3,
 ( #78125, #47206, #16245, #70536, #29460, #38583 ),
 .UNSPECIFIED., .F., .F.,
 ( 4, 2, 4 ),
 ( 0.000000000000000000, 0.001380764517854762147, 0.002761529035709524293 ),
 .UNSPECIFIED. ) ;
#44198 = VERTEX_POINT ( 'NONE', #70101 ) ;
#44200 = VERTEX_POINT ( 'NONE', #23916 ) ;
#44199 = AXIS2_PLACEMENT_3D ( 'NONE', #2475, #65398, #25803 ) ;
#44201 = CARTESIAN_POINT ( 'NONE',  ( 29.68479148105952348, -1.477225279485574028, -9.431263391055122014 ) ) ;
#44202 = CARTESIAN_POINT ( 'NONE',  ( 2.989331223418256744, -5.876774720514424288, 21.46569930292093886 ) ) ;
#44203 = ORIENTED_EDGE ( 'NONE', *, *, #63335, .F. ) ;
#44204 = ORIENTED_EDGE ( 'NONE', *, *, #36146, .T. ) ;
#44205 = EDGE_LOOP ( 'NONE', ( #80637, #90590, #1525, #74436 ) ) ;
#44206 = CARTESIAN_POINT ( 'NONE',  ( -39.52287095715009002, -23.95044443724991368, 10.65354141964649592 ) ) ;
#44207 = DIRECTION ( 'NONE',  ( -0.8760724843741984902, 0.000000000000000000, -0.4821794293853893798 ) ) ;
#44208 = CARTESIAN_POINT ( 'NONE',  ( -119.5228709571500616, -23.48783264082477018, -1.443836473390082142 ) ) ;
#44209 = CARTESIAN_POINT ( 'NONE',  ( 18.38559056850662543, 9.607341378227904016, -1.500000000000002220 ) ) ;
#44210 = CARTESIAN_POINT ( 'NONE',  ( -1.994712787082457472, 21.64621699974126656, 11.49999999999999645 ) ) ;
#44211 = EDGE_LOOP ( 'NONE', ( #86959, #95248, #5803, #92741 ) ) ;
#44212 = CARTESIAN_POINT ( 'NONE',  ( -100.9357141943721530, -25.20148372820526816, 3.413620792782795732 ) ) ;
#44213 = CARTESIAN_POINT ( 'NONE',  ( -100.5228709571500616, -29.50250786944525672, 11.44777988621623166 ) ) ;
#44214 = CARTESIAN_POINT ( 'NONE',  ( -115.6323215094300991, -23.48783264082477018, -1.443836473390087916 ) ) ;
#44215 = CARTESIAN_POINT ( 'NONE',  ( 9.841385673706204429, 20.17164819615926064, -1.500000000000002220 ) ) ;
#44216 = EDGE_CURVE ( 'NONE', #23841, #54069, #30531, .T. ) ;
#44217 = CARTESIAN_POINT ( 'NONE',  ( -40.01839366089613748, -25.30501058306510487, 5.509688048021296858 ) ) ;
#44218 = ORIENTED_EDGE ( 'NONE', *, *, #65617, .T. ) ;
#44219 = DIRECTION ( 'NONE',  ( 0.000000000000000000, 0.000000000000000000, -1.000000000000000000 ) ) ;
#44220 = CARTESIAN_POINT ( 'NONE',  ( -51.69084450196597658, -25.24874092950897264, 3.825624438094035629 ) ) ;
#44221 = B_SPLINE_SURFACE_WITH_KNOTS ( 'NONE', 3, 3, ( 
 ( #60480, #76165, #37118, #5174 ),
 ( #89418, #36129, #50864, #67099 ),
 ( #28508, #99003, #91396, #21873 ),
 ( #30500, #99501, #38111, #60971 ),
 ( #84786, #92896, #22372, #23886 ),
 ( #23373, #78164, #85799, #16279 ),
 ( #91896, #39618, #77665, #54859 ) ),
 .UNSPECIFIED., .F., .F., .F.,
 ( 4, 3, 4 ),
 ( 4, 4 ),
 ( 0.7945040050992243641, 0.8970133687736501216, 0.9995227324480757680 ),
 ( 0.3195752057335992657, 0.3207354674102795289 ),
 .UNSPECIFIED. ) ;
#44222 = ORIENTED_EDGE ( 'NONE', *, *, #75182, .F. ) ;
#44223 = ORIENTED_EDGE ( 'NONE', *, *, #34333, .T. ) ;
#44224 = ADVANCED_FACE ( 'NONE', ( #78688 ), #583, .T. ) ;
#44225 = PLANE ( 'NONE',  #26393 ) ;
#44226 = VERTEX_POINT ( 'NONE', #15299 ) ;
#44227 = CARTESIAN_POINT ( 'NONE',  ( 19.49461108348020133, 8.573440864381753457, -1.500000000000002220 ) ) ;
#44228 = ORIENTED_EDGE ( 'NONE', *, *, #34085, .T. ) ;
#44229 = DIRECTION ( 'NONE',  ( 1.000000000000000000, -0.000000000000000000, 0.000000000000000000 ) ) ;
#44230 = PRODUCT ( 'Locking Button_Varsay\X2\0131\X0\lan', 'Locking Button_Varsay\X2\0131\X0\lan', '', ( #34163 ) ) ;
#44231 = CARTESIAN_POINT ( 'NONE',  ( -20.94189920129180038, 1.864940847883316488, 11.49999999999998934 ) ) ;
#44232 = DIRECTION ( 'NONE',  ( 0.000000000000000000, -0.9999999999976377785, -2.173523156925979975E-06 ) ) ;
#44233 = CARTESIAN_POINT ( 'NONE',  ( 21.16149768242404861, -8.233860041645145955, 11.49999999999998934 ) ) ;
#44234 = PLANE ( 'NONE',  #42127 ) ;
#44235 = DIRECTION ( 'NONE',  ( 1.000000000000000000, 0.000000000000000000, 0.000000000000000000 ) ) ;
#44236 = CARTESIAN_POINT ( 'NONE',  ( 10.99670386783381737, -19.00842362925918749, -1.500000000000002220 ) ) ;
#44237 = DIRECTION ( 'NONE',  ( -3.773278334453079030E-23, 0.9999999999976377785, 2.173523156925979128E-06 ) ) ;
#44238 = ORIENTED_EDGE ( 'NONE', *, *, #57989, .T. ) ;
#44239 = CARTESIAN_POINT ( 'NONE',  ( -0.02075734969026145696, 5.866774720514426278, -22.78097719988138081 ) ) ;
#44240 = ADVANCED_FACE ( 'NONE', ( #85312 ), #61498, .T. ) ;
#44241 = AXIS2_PLACEMENT_3D ( 'NONE', #54834, #24862, #92872 ) ;
#44242 = ORIENTED_EDGE ( 'NONE', *, *, #74914, .F. ) ;
#44243 = CARTESIAN_POINT ( 'NONE',  ( -25.92875734969025814, -3.316774720514426456, 30.51402280011862089 ) ) ;
#44244 = VECTOR ( 'NONE', #5697, 1000.000000000000227 ) ;
#44245 = DIRECTION ( 'NONE',  ( -1.000000000000000000, 0.000000000000000000, -0.000000000000000000 ) ) ;
#44246 = CARTESIAN_POINT ( 'NONE',  ( -30.61247030481453990, -24.47854930503728710, 0.5637492489085954572 ) ) ;
#44247 = CARTESIAN_POINT ( 'NONE',  ( -16.96849063341007380, -12.82450338531451450, -1.500000000000002220 ) ) ;
#44248 = CARTESIAN_POINT ( 'NONE',  ( -112.5918940264897543, -23.96119346886881729, -0.6495511937831842664 ) ) ;
#44249 = DIRECTION ( 'NONE',  ( -0.9890158633619158257, -0.1478094111296165414, -0.000000000000000000 ) ) ;
#44250 = CARTESIAN_POINT ( 'NONE',  ( -114.5228709571500332, -23.73907113217684284, -1.053371485781013916 ) ) ;
#44251 = B_SPLINE_CURVE_WITH_KNOTS ( 'NONE', 3,
 ( #99579, #16356, #55439, #46316 ),
 .UNSPECIFIED., .F., .F.,
 ( 4, 4 ),
 ( 0.6992755142499577081, 0.7002762612907231787 ),
 .UNSPECIFIED. ) ;
#44252 = CARTESIAN_POINT ( 'NONE',  ( -85.62287095715002749, -24.91570333823100114, 8.075032458375551059 ) ) ;
#44253 = DIRECTION ( 'NONE',  ( 0.000000000000000000, 0.000000000000000000, -1.000000000000000000 ) ) ;
#44254 = ORIENTED_EDGE ( 'NONE', *, *, #94892, .F. ) ;
#44255 = CARTESIAN_POINT ( 'NONE',  ( -7.889300446747370188, -17.95381117360125955, 11.49999999999999645 ) ) ;
#44256 = CARTESIAN_POINT ( 'NONE',  ( -78.52287095715007581, -23.96177878511308634, 10.65340807706329862 ) ) ;
#44257 = CARTESIAN_POINT ( 'NONE',  ( -90.70649462243461869, -25.26877915520014639, 5.947789088310639904 ) ) ;
#44258 = B_SPLINE_CURVE_WITH_KNOTS ( 'NONE', 3,
 ( #91954, #25329, #56306, #99548 ),
 .UNSPECIFIED., .F., .F.,
 ( 4, 4 ),
 ( 0.5308790877619156134, 0.5398855190340309251 ),
 .UNSPECIFIED. ) ;
#44259 = EDGE_LOOP ( 'NONE', ( #5415, #41971, #61726, #66218 ) ) ;
#44260 = CARTESIAN_POINT ( 'NONE',  ( -69.00197608513569492, -25.28274124714703319, 5.751830946319327786 ) ) ;
#44261 = CARTESIAN_POINT ( 'NONE',  ( -99.38203303823797796, -25.31439660168539518, 5.782495694000596487 ) ) ;
#44262 = CARTESIAN_POINT ( 'NONE',  ( -42.52287095715004739, -23.48783264083366973, -1.443836473376261642 ) ) ;
#44263 = TOROIDAL_SURFACE ( 'NONE', #39403, 253.2618649670780826, 1.835999999999999854 ) ;
#44264 = CARTESIAN_POINT ( 'NONE',  ( -89.49044893904931541, -25.11033443465437287, 2.832404802291436319 ) ) ;
#44265 = CARTESIAN_POINT ( 'NONE',  ( -2.355416116969162754, -19.56741566493107598, 11.49999999999998934 ) ) ;
#44267 = VERTEX_POINT ( 'NONE', #46261 ) ;
#44266 = LOCAL_TIME ( 0, 54, 15.00000000000000000, #47027 ) ;
#44268 = DIRECTION ( 'NONE',  ( -3.773278334453079618E-23, 0.9999999999976377785, 2.173523156925979975E-06 ) ) ;
#44269 = CARTESIAN_POINT ( 'NONE',  ( 30.61558314414154580, -3.638221654638376990, 27.34201279177319321 ) ) ;
#44270 = AXIS2_PLACEMENT_3D ( 'NONE', #42917, #49536, #34798 ) ;
#44271 = CALENDAR_DATE ( 2026, 9, 10 ) ;
#44272 = EDGE_CURVE ( 'NONE', #72199, #69148, #29491, .T. ) ;
#44273 = VERTEX_POINT ( 'NONE', #8708 ) ;
#44274 = CARTESIAN_POINT ( 'NONE',  ( 8.940588884021771321, 1.075525492964989691E-15, 3.692441190372578674 ) ) ;
#44275 = CARTESIAN_POINT ( 'NONE',  ( -103.6228709571500559, -23.48786465467241769, 11.44779295918254114 ) ) ;
#44276 = CARTESIAN_POINT ( 'NONE',  ( -47.50045621308397159, -24.15543982623907127, -0.2315651400026536022 ) ) ;
#44277 = CARTESIAN_POINT ( 'NONE',  ( -84.58953762381675290, -23.47596703998600631, 11.44779298504227683 ) ) ;
#44278 = PLANE ( 'NONE',  #64764 ) ;
#44279 = EDGE_CURVE ( 'NONE', #55323, #79408, #99271, .T. ) ;
#44280 = CARTESIAN_POINT ( 'NONE',  ( -69.79628282111092119, -25.31201622179200683, 5.458995709863208035 ) ) ;
#44281 = EDGE_CURVE ( 'NONE', #18260, #68279, #46768, .T. ) ;
#44282 = CARTESIAN_POINT ( 'NONE',  ( -120.6228709571500417, -23.47593901973091235, -1.443836447538997536 ) ) ;
#44283 = CARTESIAN_POINT ( 'NONE',  ( -18.23705311251027794, 8.147635122911419003, -1.500000000000002220 ) ) ;
#44284 = ADVANCED_FACE ( 'NONE', ( #9194 ), #47270, .T. ) ;
#44285 = CARTESIAN_POINT ( 'NONE',  ( -100.4381051993576506, -25.27532861597270042, 2.832404458683261961 ) ) ;
#44286 = CARTESIAN_POINT ( 'NONE',  ( -0.05926229584106505049, -22.28280300962049054, 9.277709158646871401 ) ) ;
#44287 = VERTEX_POINT ( 'NONE', #39645 ) ;
#44288 = DIRECTION ( 'NONE',  ( 0.000000000000000000, 1.000000000000000000, 0.000000000000000000 ) ) ;
#44289 = CARTESIAN_POINT ( 'NONE',  ( 12.46200043076872888, -4.205547148226783882, -28.02060279727989922 ) ) ;
#44290 = EDGE_CURVE ( 'NONE', #9907, #40297, #11353, .T. ) ;
#44291 = CARTESIAN_POINT ( 'NONE',  ( -119.5222410164763147, -23.48783264082477373, -1.443836473390087916 ) ) ;
#44292 = CARTESIAN_POINT ( 'NONE',  ( -80.58924316370918461, -24.52399227489127398, 9.353111116836524630 ) ) ;
#44293 = CARTESIAN_POINT ( 'NONE',  ( -127.4335858270658832, -25.30062225142111032, 5.394419286057580365 ) ) ;
#44294 = CARTESIAN_POINT ( 'NONE',  ( -81.54694949955771222, -24.34968618360933945, 0.1864209137778954084 ) ) ;
#44295 = CARTESIAN_POINT ( 'NONE',  ( -28.13975365244298388, -24.60093900632847053, 1.675771093763900099 ) ) ;
#44296 = CARTESIAN_POINT ( 'NONE',  ( -1.394533802543915124, -5.876774720514413630, 20.19722303762275573 ) ) ;
#44297 = ORIENTED_EDGE ( 'NONE', *, *, #80045, .F. ) ;
#44298 = B_SPLINE_SURFACE_WITH_KNOTS ( 'NONE', 3, 1, ( 
 ( #49331, #87879 ),
 ( #95487, #86373 ),
 ( #71657, #16351 ),
 ( #39690, #79250 ),
 ( #64068, #94982 ),
 ( #18363, #17865 ),
 ( #71157, #1647 ),
 ( #25973, #80263 ),
 ( #47317, #10756 ),
 ( #56945, #32079 ),
 ( #34098, #70649 ),
 ( #3157, #24468 ),
 ( #8752, #41210 ),
 ( #41720, #9748 ),
 ( #33089, #48829 ),
 ( #17360, #72660 ),
 ( #16857, #65070 ),
 ( #32582, #40703 ),
 ( #23962, #79755 ) ),
 .UNSPECIFIED., .F., .F., .F.,
 ( 4, 1, 1, 1, 1, 1, 1, 1, 1, 1, 1, 1, 1, 1, 1, 1, 4 ),
 ( 2, 2 ),
 ( 0.000000000000000000, 0.06318289109391794778, 0.1237330903858703257, 0.1836062326498469899, 0.2427039625557292357, 0.3016492823581786720, 0.3610699883815534639, 0.4220736591995472020, 0.4842519596996277542, 0.5473469430655184542, 0.6093464547651399332, 0.6708936127785768422, 0.7332102753497369285, 0.7968038021902664747, 0.8620990789963799417, 0.9294007105664079393, 1.000000000000000000 ),
 ( 0.000000000000000000, 1.000000000000000000 ),
 .UNSPECIFIED. ) ;
#44299 = CARTESIAN_POINT ( 'NONE',  ( -2.606012662418322634, -5.876774720514410077, 19.21974929698718881 ) ) ;
#44300 = B_SPLINE_CURVE_WITH_KNOTS ( 'NONE', 3,
 ( #62983, #2573, #16280, #17792 ),
 .UNSPECIFIED., .F., .F.,
 ( 4, 4 ),
 ( 0.3590215203896768847, 0.3600222674304420223 ),
 .UNSPECIFIED. ) ;
#44301 = CARTESIAN_POINT ( 'NONE',  ( -127.5892768804099404, -24.65952944569305316, 1.056160979905708341 ) ) ;
#44302 = EDGE_LOOP ( 'NONE', ( #20770, #4515, #22220, #7988 ) ) ;
#44303 = B_SPLINE_CURVE_WITH_KNOTS ( 'NONE', 3,
 ( #87350, #47296, #95467, #78223 ),
 .UNSPECIFIED., .F., .F.,
 ( 4, 4 ),
 ( 0.000000000000000000, 9.999999999998897304E-05 ),
 .UNSPECIFIED. ) ;
#44304 = CARTESIAN_POINT ( 'NONE',  ( -19.72078065558051208, -4.686549088087978099, 11.49999999999998934 ) ) ;
#44305 = CARTESIAN_POINT ( 'NONE',  ( -105.5562042904833788, -24.99156044556202971, 7.747789690856173195 ) ) ;
#44306 = CARTESIAN_POINT ( 'NONE',  ( 14.87948092214613460, 4.970807589639875346, -27.40745209048265352 ) ) ;
#44307 = AXIS2_PLACEMENT_3D ( 'NONE', #5784, #98121, #19511 ) ;
#44308 = LINE ( 'NONE', #35690, #5472 ) ;
#44309 = VERTEX_POINT ( 'NONE', #94431 ) ;
#44310 = CARTESIAN_POINT ( 'NONE',  ( -116.5228709571500616, -24.64965694238575011, 8.947790433994191162 ) ) ;
#44311 = FACE_OUTER_BOUND ( 'NONE', #70395, .T. ) ;
#44312 = CARTESIAN_POINT ( 'NONE',  ( 7.746586651691365510, 18.53313339873204058, -1.500000000000002220 ) ) ;
#44313 = VECTOR ( 'NONE', #64149, 1000.000000000000114 ) ;
#44314 = CARTESIAN_POINT ( 'NONE',  ( 20.78037738254806399, 3.014218216234254566, 11.49999999999999645 ) ) ;
#44315 = CARTESIAN_POINT ( 'NONE',  ( -29.24636659181000198, -25.21267509515801564, 4.940287023516041209 ) ) ;
#44316 = CARTESIAN_POINT ( 'NONE',  ( -111.6228709571500559, -24.64965695001468404, 8.947790433994176951 ) ) ;
#44317 = CARTESIAN_POINT ( 'NONE',  ( 2.303347834742990763, 21.97011321758780866, 11.49999999999998934 ) ) ;
#44318 = CARTESIAN_POINT ( 'NONE',  ( 18.14102482237423075, -9.550406459077080967, -1.500000000000002220 ) ) ;
#44319 = CARTESIAN_POINT ( 'NONE',  ( -39.44687923781921057, -25.27805912342874706, 4.188173683520872714 ) ) ;
#44320 = CARTESIAN_POINT ( 'NONE',  ( 30.93860345374796594, -6.475225279485573360, 19.84760796525321780 ) ) ;
#44321 = LINE ( 'NONE', #75249, #80090 ) ;
#44322 = ORIENTED_EDGE ( 'NONE', *, *, #81373, .F. ) ;
#44323 = CARTESIAN_POINT ( 'NONE',  ( -100.2744028882005409, -25.12156721190337905, 2.838270228797207917 ) ) ;
#44324 = CARTESIAN_POINT ( 'NONE',  ( -130.5728709571500588, -23.47596703998600631, 11.44779298504227860 ) ) ;
#44325 = VERTEX_POINT ( 'NONE', #55386 ) ;
#44326 = ORIENTED_EDGE ( 'NONE', *, *, #71496, .T. ) ;
#44327 = CARTESIAN_POINT ( 'NONE',  ( 22.81105451610979173, 1.682774720514426114, -18.46691820600746681 ) ) ;
#44328 = CARTESIAN_POINT ( 'NONE',  ( -81.22287095715006444, -23.47596703998600631, 11.44779298504227860 ) ) ;
#44329 = CARTESIAN_POINT ( 'NONE',  ( -76.58463740794132946, -24.51314013834316441, 0.6176544820404190617 ) ) ;
#44330 = CARTESIAN_POINT ( 'NONE',  ( -19.32567751138619982, -7.045664331180771178, -1.500000000000002220 ) ) ;
#44331 = CARTESIAN_POINT ( 'NONE',  ( -18.53595284743415661, 10.95218985133829825, 11.49999999999999645 ) ) ;
#44332 = ORIENTED_EDGE ( 'NONE', *, *, #94097, .T. ) ;
#44333 = FACE_OUTER_BOUND ( 'NONE', #63811, .T. ) ;
#44334 = CARTESIAN_POINT ( 'NONE',  ( -4.495793269230770939, -6.376774720514410077, 19.27714342948718595 ) ) ;
#44335 = CARTESIAN_POINT ( 'NONE',  ( 14.50327815619135308, -17.01817589256642194, -1.500000000000002220 ) ) ;
#44337 = CARTESIAN_POINT ( 'NONE',  ( -93.52287095715007581, -23.72747288104470798, -1.053458166803226348 ) ) ;
#44336 = AXIS2_PLACEMENT_3D ( 'NONE', #24308, #78576, #9083 ) ;
#44338 = CARTESIAN_POINT ( 'NONE',  ( 3.787259615384621192, -5.876774720514425177, 21.48076923076922640 ) ) ;
#44339 = VERTEX_POINT ( 'NONE', #88 ) ;
#44340 = FACE_OUTER_BOUND ( 'NONE', #10114, .T. ) ;
#44341 = CARTESIAN_POINT ( 'NONE',  ( -49.58207262147149663, -24.51419770103158413, 9.386484678747189392 ) ) ;
#44342 = B_SPLINE_CURVE_WITH_KNOTS ( 'NONE', 3,
 ( #74562, #20760, #52234, #68950 ),
 .UNSPECIFIED., .F., .F.,
 ( 4, 4 ),
 ( 0.000000000000000000, 1.000000000000000000 ),
 .UNSPECIFIED. ) ;
#44343 = CARTESIAN_POINT ( 'NONE',  ( 20.83135763335140922, 1.668377004047274959, -1.500000000000002220 ) ) ;
#44344 = ORIENTED_EDGE ( 'NONE', *, *, #16689, .T. ) ;
#44345 = EDGE_CURVE ( 'NONE', #13092, #51806, #44070, .T. ) ;
#44347 = ORIENTED_EDGE ( 'NONE', *, *, #63416, .F. ) ;
#44346 = LINE ( 'NONE', #152, #29555 ) ;
#44348 = ORIENTED_EDGE ( 'NONE', *, *, #12661, .T. ) ;
#44349 = CIRCLE ( 'NONE', #42762, 27.94799999999999685 ) ;
#44350 = CARTESIAN_POINT ( 'NONE',  ( -100.5221651912381589, -23.48786465467241413, 11.44779295918254469 ) ) ;
#44351 = CARTESIAN_POINT ( 'NONE',  ( -5.075574613727041218, 20.51645923614106337, -1.500000000000002220 ) ) ;
#44352 = EDGE_CURVE ( 'NONE', #94222, #24461, #86821, .T. ) ;
#44353 = EDGE_LOOP ( 'NONE', ( #76364, #27377, #35961, #20607 ) ) ;
#44354 = CARTESIAN_POINT ( 'NONE',  ( -112.5228709571500616, -23.47596703998600631, 11.44779298504228038 ) ) ;
#44355 = CARTESIAN_POINT ( 'NONE',  ( -49.04309943529236904, -25.29535962531968707, 5.511470466757466546 ) ) ;
#44356 = CARTESIAN_POINT ( 'NONE',  ( -110.3346797185884327, -25.18492896333868813, 3.293943116708551777 ) ) ;
#44357 = AXIS2_PLACEMENT_3D ( 'NONE', #45862, #6295, #6786 ) ;
#44358 = CARTESIAN_POINT ( 'NONE',  ( -28.52287095715005094, -23.31182002239687989, -1.443836447538998202 ) ) ;
#44359 = CARTESIAN_POINT ( 'NONE',  ( -33.52287095715006160, -23.47593901973090169, -1.443836447538997314 ) ) ;
#44360 = CARTESIAN_POINT ( 'NONE',  ( -9.430186865587145917, -19.61854929170128869, -1.500000000000002220 ) ) ;
#44361 = CARTESIAN_POINT ( 'NONE',  ( -71.56719770743626441, -25.31639610870687918, 5.535760714805260996 ) ) ;
#44363 = EDGE_LOOP ( 'NONE', ( #14339, #51405, #52865, #68693 ) ) ;
#44362 = CARTESIAN_POINT ( 'NONE',  ( 21.15698459081360383, -7.064864530413820454, 11.49999999999999645 ) ) ;
#44364 = DIRECTION ( 'NONE',  ( -1.000000000000000000, 0.000000000000000000, 0.000000000000000000 ) ) ;
#44365 = CARTESIAN_POINT ( 'NONE',  ( 14.62591090210861999, 3.611920024593927803, -27.34381298535168270 ) ) ;
#44366 = CARTESIAN_POINT ( 'NONE',  ( -100.9228709571500673, -23.47593901973090169, -1.443836447538996870 ) ) ;
#44367 = ORIENTED_EDGE ( 'NONE', *, *, #97536, .T. ) ;
#44368 = ORIENTED_EDGE ( 'NONE', *, *, #85601, .T. ) ;
#44369 = EDGE_LOOP ( 'NONE', ( #56078, #86192, #81311 ) ) ;
#44370 = CARTESIAN_POINT ( 'NONE',  ( 14.52511747680497933, 6.475225279485573360, -27.86035006098926559 ) ) ;
#44371 = PLANE ( 'NONE',  #48208 ) ;
#44372 = PLANE ( 'NONE',  #18712 ) ;
#44373 = LINE ( 'NONE', #75298, #97222 ) ;
#44374 = CARTESIAN_POINT ( 'NONE',  ( -15.38109395195050233, 11.78095549196778258, 11.49999999999998934 ) ) ;
#44375 = DIRECTION ( 'NONE',  ( -1.000000000000000000, -0.000000000000000000, -0.000000000000000000 ) ) ;
#44376 = ORIENTED_EDGE ( 'NONE', *, *, #91231, .F. ) ;
#44377 = CARTESIAN_POINT ( 'NONE',  ( -5.798782886354239885, 18.49141925852020663, 11.49999999999999645 ) ) ;
#44378 = FACE_OUTER_BOUND ( 'NONE', #19348, .T. ) ;
#44379 = ORIENTED_EDGE ( 'NONE', *, *, #21236, .F. ) ;
#44381 = CARTESIAN_POINT ( 'NONE',  ( 3.202571139211427553, -5.876774720514406525, 18.81074098386681470 ) ) ;
#44380 = AXIS2_PLACEMENT_3D ( 'NONE', #95585, #26072, #17965 ) ;
#44382 = CARTESIAN_POINT ( 'NONE',  ( 2.591645189881369493, -6.376774720514411854, 19.84288601127407148 ) ) ;
#44383 = PLANE ( 'NONE',  #30341 ) ;
#44384 = CARTESIAN_POINT ( 'NONE',  ( -87.62287095715002749, -24.50321055353804667, 9.387540953477525818 ) ) ;
#44385 = ADVANCED_FACE ( 'NONE', ( #92922 ), #38138, .T. ) ;
#44386 = CARTESIAN_POINT ( 'NONE',  ( -19.57149217635686966, 1.386223266712492297, 11.49999999999998934 ) ) ;
#44387 = B_SPLINE_CURVE_WITH_KNOTS ( 'NONE', 3,
 ( #84359, #99568, #84860, #30071 ),
 .UNSPECIFIED., .F., .F.,
 ( 4, 4 ),
 ( 0.000000000000000000, 0.0001000000000000028644 ),
 .UNSPECIFIED. ) ;
#44388 = AXIS2_PLACEMENT_3D ( 'NONE', #10990, #12484, #74871 ) ;
#44389 = CARTESIAN_POINT ( 'NONE',  ( -46.53038060754152383, -24.65952944569304606, 1.056160979905696351 ) ) ;
#44390 = ORIENTED_EDGE ( 'NONE', *, *, #30315, .T. ) ;
#44391 = CARTESIAN_POINT ( 'NONE',  ( 19.98928912078053699, -8.061568661392884749, 11.49999999999998934 ) ) ;
#44392 = CARTESIAN_POINT ( 'NONE',  ( -85.62287095715005592, -23.47596703998600631, 11.44779298504227860 ) ) ;
#44393 = CARTESIAN_POINT ( 'NONE',  ( 30.93860345374796594, -0.6647747205144264315, 19.84760796525321780 ) ) ;
#44394 = CARTESIAN_POINT ( 'NONE',  ( 1.305682803664691249, 5.965225279485572685, 29.57950906855421991 ) ) ;
#44395 = DIRECTION ( 'NONE',  ( -3.773278334453079618E-23, 0.9999999999976377785, 2.173523156925979975E-06 ) ) ;
#44396 = CARTESIAN_POINT ( 'NONE',  ( 17.43399715339889511, -14.94103553264482720, -1.500000000000002220 ) ) ;
#44397 = APPROVAL_STATUS ( 'not_yet_approved' ) ;
#44398 = DIRECTION ( 'NONE',  ( 0.2488812114211667315, 0.000000000000000000, 0.9685340172660600322 ) ) ;
#44399 = CARTESIAN_POINT ( 'NONE',  ( -49.62369267386219462, -24.65952944569304606, 1.056160979905696129 ) ) ;
#44400 = CARTESIAN_POINT ( 'NONE',  ( 10.61947033613929214, 17.11087026910869469, 11.49999999999999645 ) ) ;
#44401 = CARTESIAN_POINT ( 'NONE',  ( -109.6441887128288784, -25.28814102335254788, 2.986266316960244804 ) ) ;
#44402 = CARTESIAN_POINT ( 'NONE',  ( 7.749999999999998224, 24.84999999999999787, 0.000000000000000000 ) ) ;
#44403 = EDGE_CURVE ( 'NONE', #21992, #25724, #36880, .T. ) ;
#44404 = CARTESIAN_POINT ( 'NONE',  ( -104.6228709571500559, -24.65952944569304961, 1.056160979905701236 ) ) ;
#44405 = PLANE ( 'NONE',  #94209 ) ;
#44406 = B_SPLINE_CURVE_WITH_KNOTS ( 'NONE', 3,
 ( #53287, #67028, #84218, #97936, #20815, #54794 ),
 .UNSPECIFIED., .F., .F.,
 ( 4, 2, 4 ),
 ( 1.570887131794638196E-05, 0.001396322306279763458, 0.002776935741241580609 ),
 .UNSPECIFIED. ) ;
#44407 = CARTESIAN_POINT ( 'NONE',  ( -111.1213521864704035, -25.29779229951232011, 3.637108192089848480 ) ) ;
#44408 = CARTESIAN_POINT ( 'NONE',  ( -11.18921147948170614, -16.41150865552512883, 11.49999999999998934 ) ) ;
#44409 = EDGE_CURVE ( 'NONE', #2532, #73037, #2936, .T. ) ;
#44410 = LINE ( 'NONE', #75334, #30135 ) ;
#44411 = CARTESIAN_POINT ( 'NONE',  ( 17.16143643543069075, 9.858047367376444825, -1.500000000000002220 ) ) ;
#44412 = CARTESIAN_POINT ( 'NONE',  ( -126.5562100481780448, -23.73791477778912551, 11.05961554403169878 ) ) ;
#44413 = EDGE_CURVE ( 'NONE', #64035, #13507, #12615, .T. ) ;
#44414 = EDGE_CURVE ( 'NONE', #68323, #73714, #62229, .T. ) ;
#44415 = CARTESIAN_POINT ( 'NONE',  ( -0.4362980769230789257, -6.376774720514411854, 19.46153846153846345 ) ) ;
#44416 = CARTESIAN_POINT ( 'NONE',  ( -1.390986686320385468, -6.376774720514413630, 19.62288733224860948 ) ) ;
#44417 = CARTESIAN_POINT ( 'NONE',  ( -17.26476610439243231, 11.37957233835482818, 11.49999999999999645 ) ) ;
#44418 = DIRECTION ( 'NONE',  ( 2.352173255807804438E-16, -2.352173255807796056E-16, -1.000000000000000000 ) ) ;
#44419 = EDGE_CURVE ( 'NONE', #35655, #81742, #87322, .T. ) ;
#44420 = DIRECTION ( 'NONE',  ( 1.000000000000000000, 3.773278334444166432E-23, 8.201307841325785021E-29 ) ) ;
#44421 = PLANE ( 'NONE',  #58730 ) ;
#44422 = CARTESIAN_POINT ( 'NONE',  ( -22.67762270672801250, 1.536325718666671225, 11.49999999999999645 ) ) ;
#44423 = ORIENTED_EDGE ( 'NONE', *, *, #15306, .F. ) ;
#44424 = CARTESIAN_POINT ( 'NONE',  ( -91.62287095715004170, -23.47593901973091235, -1.443836447539002865 ) ) ;
#44425 = DIRECTION ( 'NONE',  ( -0.7071067811865516806, -0.7071067811865434649, 0.000000000000000000 ) ) ;
#44426 = EDGE_CURVE ( 'NONE', #96655, #11694, #13439, .T. ) ;
#44427 = PLANE ( 'NONE',  #97010 ) ;
#44428 = CYLINDRICAL_SURFACE ( 'NONE', #78748, 3.500000000000000000 ) ;
#44429 = VERTEX_POINT ( 'NONE', #49289 ) ;
#44430 = ORIENTED_EDGE ( 'NONE', *, *, #49978, .F. ) ;
#44431 = CARTESIAN_POINT ( 'NONE',  ( -98.62287095715007013, -23.47596703998600631, 11.44779298504227860 ) ) ;
#44432 = CARTESIAN_POINT ( 'NONE',  ( -20.40978113611479827, 10.34812579263477872, 11.49999999999998934 ) ) ;
#44433 = FACE_OUTER_BOUND ( 'NONE', #59412, .T. ) ;
#44434 = CARTESIAN_POINT ( 'NONE',  ( 14.33184905138074683, -16.10332302735202958, -1.500000000000002220 ) ) ;
#44435 = CARTESIAN_POINT ( 'NONE',  ( -123.5538550107125673, -24.65952944569305316, 1.056160979905706343 ) ) ;
#44436 = CARTESIAN_POINT ( 'NONE',  ( -5.366453405989236813, 0.000000000000000000, 24.00000000000000000 ) ) ;
#44437 = CARTESIAN_POINT ( 'NONE',  ( -22.39070119279581306, -2.479732019442284496, 11.49999999999999645 ) ) ;
#44438 = ORIENTED_EDGE ( 'NONE', *, *, #5353, .T. ) ;
#44439 = DIRECTION ( 'NONE',  ( -3.773278334444167608E-23, 1.000000000000000000, 0.000000000000000000 ) ) ;
#44440 = CARTESIAN_POINT ( 'NONE',  ( 3.689792033372774060, 21.67897595795444587, -1.500000000000002220 ) ) ;
#44441 = CARTESIAN_POINT ( 'NONE',  ( -105.5995568635892425, -23.48786465467241769, 11.44779295918254114 ) ) ;
#44442 = CARTESIAN_POINT ( 'NONE',  ( -41.77018777319382536, -25.29087217084345340, 3.672889645907745138 ) ) ;
#44443 = EDGE_LOOP ( 'NONE', ( #24826, #96348, #66232, #16012 ) ) ;
#44444 = DIRECTION ( 'NONE',  ( -1.000000000000000000, -3.773278334444166432E-23, -8.201307841325785021E-29 ) ) ;
#44445 = CARTESIAN_POINT ( 'NONE',  ( -90.54280662865561169, -24.83644354573578994, 8.397322867130100121 ) ) ;
#44446 = ORIENTED_EDGE ( 'NONE', *, *, #74519, .F. ) ;
#44447 = CARTESIAN_POINT ( 'NONE',  ( -29.52287095715006515, -24.26482661340494573, 0.1850815758097280328 ) ) ;
#44448 = EDGE_LOOP ( 'NONE', ( #24120, #45329, #44348, #37747 ) ) ;
#44449 = ORIENTED_EDGE ( 'NONE', *, *, #60102, .F. ) ;
#44450 = CARTESIAN_POINT ( 'NONE',  ( -49.34347621332902634, -25.28835214115807872, 5.818256392113962505 ) ) ;
#44451 = DIRECTION ( 'NONE',  ( 1.000000000000000000, 0.000000000000000000, 0.000000000000000000 ) ) ;
#44452 = CARTESIAN_POINT ( 'NONE',  ( -20.27875734969026311, 7.743225279485574042, 22.60402280011862430 ) ) ;
#44453 = CARTESIAN_POINT ( 'NONE',  ( 13.86372479123709311, 15.02075200336711092, -1.500000000000002220 ) ) ;
#44454 = AXIS2_PLACEMENT_3D ( 'NONE', #18232, #8620, #72528 ) ;
#44455 = ORIENTED_EDGE ( 'NONE', *, *, #76805, .T. ) ;
#44456 = CARTESIAN_POINT ( 'NONE',  ( -2.243088942307695621, -6.376774720514410077, 19.14743589743590846 ) ) ;
#44457 = CARTESIAN_POINT ( 'NONE',  ( -30.59128290392954952, -24.93418366566757882, 8.369064737642425200 ) ) ;
#44458 = B_SPLINE_CURVE_WITH_KNOTS ( 'NONE', 3,
 ( #90827, #37040, #68492, #75584 ),
 .UNSPECIFIED., .F., .F.,
 ( 4, 4 ),
 ( 0.000000000000000000, 0.0001000000000000028644 ),
 .UNSPECIFIED. ) ;
#44459 = EDGE_CURVE ( 'NONE', #87661, #95272, #573, .T. ) ;
#44460 = B_SPLINE_CURVE_WITH_KNOTS ( 'NONE', 3,
 ( #90302, #97416, #20772, #36508 ),
 .UNSPECIFIED., .F., .F.,
 ( 4, 4 ),
 ( 0.000000000000000000, 9.999999999998897304E-05 ),
 .UNSPECIFIED. ) ;
#44461 = CARTESIAN_POINT ( 'NONE',  ( -4.440151687742864617, -6.376774720514411854, 19.67013632031035897 ) ) ;
#44462 = CARTESIAN_POINT ( 'NONE',  ( -47.55620429048338593, -23.48786465467241058, 11.44779295918254292 ) ) ;
#44463 = ORIENTED_EDGE ( 'NONE', *, *, #10468, .T. ) ;
#44464 = PLANE ( 'NONE',  #54909 ) ;
#44465 = CARTESIAN_POINT ( 'NONE',  ( -101.5228709571500900, -23.48783264082477018, -1.443836473390087249 ) ) ;
#44466 = CARTESIAN_POINT ( 'NONE',  ( 2.040502595053849788, 20.68626321094233944, 11.49999999999998934 ) ) ;
#44468 = EDGE_CURVE ( 'NONE', #90388, #32133, #55033, .T. ) ;
#44467 = EDGE_LOOP ( 'NONE', ( #17624, #47036, #97737, #60322 ) ) ;
#44470 = VERTEX_POINT ( 'NONE', #82586 ) ;
#44469 = CARTESIAN_POINT ( 'NONE',  ( 4.281720980632043094, -6.376774720514408301, 18.71132571341777151 ) ) ;
#44471 = CARTESIAN_POINT ( 'NONE',  ( 30.41387671341004761, -4.976059279456417350, 19.84760796525321425 ) ) ;
#44472 = EDGE_LOOP ( 'NONE', ( #28329, #74147, #83510, #27117 ) ) ;
#44473 = ORIENTED_EDGE ( 'NONE', *, *, #70538, .T. ) ;
#44474 = DIRECTION ( 'NONE',  ( -3.773278334444167608E-23, 1.000000000000000000, 0.000000000000000000 ) ) ;
#44475 = CARTESIAN_POINT ( 'NONE',  ( -119.1722388760374258, -25.27126041720326199, 4.079010001960293508 ) ) ;
#44476 = CARTESIAN_POINT ( 'NONE',  ( -4.752075056065355518, -5.876774720514407413, 19.17724329193115551 ) ) ;
#44477 = PLANE ( 'NONE',  #82162 ) ;
#44479 = ORIENTED_EDGE ( 'NONE', *, *, #41584, .T. ) ;
#44478 = CARTESIAN_POINT ( 'NONE',  ( -17.14978611337857473, 13.99085498846200437, 11.49999999999999645 ) ) ;
#44480 = DIRECTION ( 'NONE',  ( -0.000000000000000000, -0.000000000000000000, -1.000000000000000000 ) ) ;
#44481 = CARTESIAN_POINT ( 'NONE',  ( -20.48750165597241590, 9.616757810196778777, 11.49999999999998934 ) ) ;
#44482 = B_SPLINE_CURVE_WITH_KNOTS ( 'NONE', 3,
 ( #10716, #73613, #72622, #86826 ),
 .UNSPECIFIED., .F., .F.,
 ( 4, 4 ),
 ( 2.081668171172168513E-17, 0.0001000000000000097897 ),
 .UNSPECIFIED. ) ;
#44484 = ORIENTED_EDGE ( 'NONE', *, *, #36268, .T. ) ;
#44483 = CARTESIAN_POINT ( 'NONE',  ( -99.29935056655477865, -25.30468847391853870, 5.154975380674369667 ) ) ;
#44485 = VERTEX_POINT ( 'NONE', #95939 ) ;
#44486 = VECTOR ( 'NONE', #75314, 1000.000000000000114 ) ;
#44487 = DIRECTION ( 'NONE',  ( -1.000000000000000000, -0.000000000000000000, -0.000000000000000000 ) ) ;
#44488 = CC_DESIGN_PERSON_AND_ORGANIZATION_ASSIGNMENT ( #14543, #55126, ( #28832 ) ) ;
#44489 = CARTESIAN_POINT ( 'NONE',  ( -20.11654390397962544, -0.4351469013266864860, -1.500000000000002220 ) ) ;
#44490 = B_SPLINE_SURFACE_WITH_KNOTS ( 'NONE', 3, 1, ( 
 ( #12328, #74240 ),
 ( #4735, #35683 ),
 ( #66660, #51408 ),
 ( #74724, #5226 ),
 ( #98057, #36182 ),
 ( #90957, #67149 ),
 ( #28556, #22912 ),
 ( #69629, #16328 ),
 ( #39165, #604 ),
 ( #62516, #46282 ),
 ( #6714, #77210 ),
 ( #7208, #23938 ),
 ( #30044, #46786 ),
 ( #29552, #15318 ),
 ( #83840, #77714 ) ),
 .UNSPECIFIED., .F., .F., .F.,
 ( 4, 1, 1, 1, 1, 1, 1, 1, 1, 1, 1, 1, 4 ),
 ( 2, 2 ),
 ( 0.000000000000000000, 0.08597245417931687061, 0.1699564070247753245, 0.2542168740862559284, 0.3392430307459933791, 0.4239782646133617439, 0.5058277166288100979, 0.5866357120841194650, 0.6677102638611641661, 0.7496008928139508143, 0.8308747881193089269, 0.9140520568558714309, 1.000000000000000000 ),
 ( 0.000000000000000000, 1.000000000000000000 ),
 .UNSPECIFIED. ) ;
#44491 = LINE ( 'NONE', #75415, #44081 ) ;
#44492 = ORIENTED_EDGE ( 'NONE', *, *, #62512, .T. ) ;
#44494 = B_SPLINE_CURVE_WITH_KNOTS ( 'NONE', 3,
 ( #4402, #35353, #58681, #89629, #20110, #51073 ),
 .UNSPECIFIED., .F., .F.,
 ( 4, 2, 4 ),
 ( 0.000000000000000000, 0.001380764517854767134, 0.002761529035709534268 ),
 .UNSPECIFIED. ) ;
#44493 = DIRECTION ( 'NONE',  ( 0.000000000000000000, 0.000000000000000000, -1.000000000000000000 ) ) ;
#44495 = CARTESIAN_POINT ( 'NONE',  ( 21.15429367616652101, -6.912965584596229895, -1.500000000000002220 ) ) ;
#44496 = B_SPLINE_CURVE_WITH_KNOTS ( 'NONE', 3,
 ( #31051, #83846, #31559, #8230, #76223, #38670 ),
 .UNSPECIFIED., .F., .F.,
 ( 4, 2, 4 ),
 ( 0.000000000000000000, 0.001380764517853252937, 0.002761529035706505875 ),
 .UNSPECIFIED. ) ;
#44497 = ORIENTED_EDGE ( 'NONE', *, *, #26099, .F. ) ;
#44498 = DIRECTION ( 'NONE',  ( -0.000000000000000000, -1.000000000000000000, -0.000000000000000000 ) ) ;
#44499 = CARTESIAN_POINT ( 'NONE',  ( -119.5228709571500758, -23.48786465467241769, 11.44779295918253759 ) ) ;
#44500 = CARTESIAN_POINT ( 'NONE',  ( -31.24388727629348494, -29.50250091417111520, 8.247779886223803203 ) ) ;
#44501 = DIRECTION ( 'NONE',  ( -3.773278334444167608E-23, 1.000000000000000000, 0.000000000000000000 ) ) ;
#44502 = CARTESIAN_POINT ( 'NONE',  ( -73.58953762381673869, -24.64965694238407323, 8.947790433994656567 ) ) ;
#44503 = CARTESIAN_POINT ( 'NONE',  ( -18.23695082634099407, 6.967386181637144738, -1.500000000000002220 ) ) ;
#44504 = CARTESIAN_POINT ( 'NONE',  ( -16.68621059303058018, 13.52761613308161870, 11.49999999999998934 ) ) ;
#44505 = CARTESIAN_POINT ( 'NONE',  ( -25.53214279450137170, -24.92775365639140972, 4.846046591611402832 ) ) ;
#44506 = CARTESIAN_POINT ( 'NONE',  ( -56.62287095715005592, -24.64898659630528499, 1.056161002820822592 ) ) ;
#44507 = CARTESIAN_POINT ( 'NONE',  ( -122.6228709571500417, -29.50250243563736774, 8.947779886222134493 ) ) ;
#44509 = VECTOR ( 'NONE', #30545, 1000.000000000000000 ) ;
#44508 = CARTESIAN_POINT ( 'NONE',  ( -21.19308438721250099, -8.479022899233653376, -1.500000000000002220 ) ) ;
#44510 = SHAPE_DEFINITION_REPRESENTATION ( #41743, #96270 ) ;
#44511 = FACE_OUTER_BOUND ( 'NONE', #5992, .T. ) ;
#44512 = CARTESIAN_POINT ( 'NONE',  ( -108.5228709571500758, -23.48783264083353473, -1.443836473376470586 ) ) ;
#44513 = CARTESIAN_POINT ( 'NONE',  ( -15.85412420263326538, -12.13584807887712458, 11.49999999999999645 ) ) ;
#44514 = CARTESIAN_POINT ( 'NONE',  ( -63.52287095715006160, -29.50248528299804818, 1.056150453629034924 ) ) ;
#44515 = CARTESIAN_POINT ( 'NONE',  ( -57.52287095715005449, -24.64898659630528854, 1.056161002820822592 ) ) ;
#44516 = DIRECTION ( 'NONE',  ( 0.000000000000000000, 2.173523156925980399E-06, -0.9999999999976378895 ) ) ;
#44517 = EDGE_CURVE ( 'NONE', #8365, #72161, #49787, .T. ) ;
#44518 = EDGE_LOOP ( 'NONE', ( #72982, #83986, #86856, #57106 ) ) ;
#44519 = CARTESIAN_POINT ( 'NONE',  ( -83.52287095715006160, -23.73934037231757088, 11.05740245334328442 ) ) ;
#44520 = CARTESIAN_POINT ( 'NONE',  ( 10.95759398273795249, -4.132774720514426292, -26.86884997114579932 ) ) ;
#44521 = VECTOR ( 'NONE', #11375, 1000.000000000000000 ) ;
#44522 = CARTESIAN_POINT ( 'NONE',  ( 1.329761939549756855, 21.69843865049760367, 11.49999999999998934 ) ) ;
#44523 = CARTESIAN_POINT ( 'NONE',  ( -37.62287095715005592, -23.47593901973091235, -1.443836447539011525 ) ) ;
#44524 = CARTESIAN_POINT ( 'NONE',  ( -9.542874777335924819, 17.09510996321218101, -1.500000000000002220 ) ) ;
#44525 = CARTESIAN_POINT ( 'NONE',  ( -80.52287095715006160, -23.48786465467241769, 11.44779295918254469 ) ) ;
#44526 = EDGE_LOOP ( 'NONE', ( #80284, #6428, #51702, #13773 ) ) ;
#44527 = DATE_AND_TIME ( #20675, #89537 ) ;
#44528 = EDGE_CURVE ( 'NONE', #68153, #69965, #94939, .T. ) ;
#44529 = CARTESIAN_POINT ( 'NONE',  ( -75.62287095715005592, -29.50250243563736774, 8.947779886222141599 ) ) ;
#44530 = DIRECTION ( 'NONE',  ( 0.000000000000000000, 1.000000000000000000, 0.000000000000000000 ) ) ;
#44531 = CARTESIAN_POINT ( 'NONE',  ( 1.819314030819549233, -20.42850443921780013, 11.49999999999999645 ) ) ;
#44532 = CARTESIAN_POINT ( 'NONE',  ( -47.52287095715005449, -24.51387760970724017, 9.387446482453409402 ) ) ;
#44533 = EDGE_CURVE ( 'NONE', #12105, #69058, #67374, .T. ) ;
#44534 = CARTESIAN_POINT ( 'NONE',  ( -53.92287095715006018, -23.47596703998600276, 11.44779298504227860 ) ) ;
#44535 = ORIENTED_EDGE ( 'NONE', *, *, #48197, .T. ) ;
#44536 = CARTESIAN_POINT ( 'NONE',  ( -30.47959251904011424, -23.47596703649177385, 11.44618536770630968 ) ) ;
#44537 = CARTESIAN_POINT ( 'NONE',  ( -40.16027052433451416, -25.28892429773494044, 3.329282795352901836 ) ) ;
#44538 = CARTESIAN_POINT ( 'NONE',  ( 32.16024265030974050, 0.3587747205144265483, 16.27760796525321751 ) ) ;
#44539 = ADVANCED_FACE ( 'NONE', ( #17310 ), #48275, .F. ) ;
#44540 = CARTESIAN_POINT ( 'NONE',  ( -61.62287095715004881, -24.64898659630528854, 1.056161002820822592 ) ) ;
#44541 = ORIENTED_EDGE ( 'NONE', *, *, #74793, .F. ) ;
#44542 = CARTESIAN_POINT ( 'NONE',  ( -119.6228709571500417, -24.65952944569304961, 1.056160979905704789 ) ) ;
#44543 = CARTESIAN_POINT ( 'NONE',  ( -6.685540227124203483, -22.02754839873749404, 11.49999999999999645 ) ) ;
#44544 = CARTESIAN_POINT ( 'NONE',  ( -2.506051680461856890, -22.62920675306992280, -1.500000000000002220 ) ) ;
#44545 = CARTESIAN_POINT ( 'NONE',  ( -115.6228709571500559, -24.99132157543166954, 2.256160258750667502 ) ) ;
#44546 = CARTESIAN_POINT ( 'NONE',  ( -45.52287095715006160, -23.47596703998600631, 11.44779298504229104 ) ) ;
#44547 = CARTESIAN_POINT ( 'NONE',  ( -120.5228709571500900, -24.14406661686758682, 10.28769366194082657 ) ) ;
#44548 = VECTOR ( 'NONE', #27560, 1000.000000000000000 ) ;
#44549 = CARTESIAN_POINT ( 'NONE',  ( -40.52287095715007581, -24.83620972994592435, 8.398175272781369216 ) ) ;
#44550 = CARTESIAN_POINT ( 'NONE',  ( -110.6272474294926269, -24.52300882791530512, 0.6510814631126382590 ) ) ;
#44551 = CARTESIAN_POINT ( 'NONE',  ( 18.42579859434530931, 11.83097890990371148, 11.49999999999998934 ) ) ;
#44552 = CARTESIAN_POINT ( 'NONE',  ( 7.448826589983275959, -5.876774720514420736, 21.05250386848070221 ) ) ;
#44553 = CARTESIAN_POINT ( 'NONE',  ( -87.58566455517073734, -24.51419770103156281, 9.386484678747175181 ) ) ;
#44554 = CARTESIAN_POINT ( 'NONE',  ( 11.04644962722740864, 4.132774720514426292, -26.87113206189456704 ) ) ;
#44555 = CARTESIAN_POINT ( 'NONE',  ( -28.62287095715007013, -23.79486920467889988, -0.6496301281144789552 ) ) ;
#44556 = CARTESIAN_POINT ( 'NONE',  ( -94.62287095715004170, -24.35013146730204525, 9.818937971375104823 ) ) ;
#44557 = CARTESIAN_POINT ( 'NONE',  ( -86.62287095715009855, -23.95044443724992789, 10.65354141964649592 ) ) ;
#44558 = ORIENTED_EDGE ( 'NONE', *, *, #75789, .T. ) ;
#44559 = CARTESIAN_POINT ( 'NONE',  ( 5.028806042385554953, -19.83023610923392610, 11.49999999999998934 ) ) ;
#44560 = ORIENTED_EDGE ( 'NONE', *, *, #48002, .F. ) ;
#44561 = ORIENTED_EDGE ( 'NONE', *, *, #79437, .T. ) ;
#44562 = VERTEX_POINT ( 'NONE', #56402 ) ;
#44563 = VERTEX_POINT ( 'NONE', #48786 ) ;
#44564 = EDGE_CURVE ( 'NONE', #5126, #79593, #37786, .T. ) ;
#44565 = CARTESIAN_POINT ( 'NONE',  ( -19.45891602060003578, 12.32625358835968576, 11.49999999999998934 ) ) ;
#44566 = CARTESIAN_POINT ( 'NONE',  ( -61.55369709315033333, -23.96119346886880308, -0.6495511937832122440 ) ) ;
#44567 = CARTESIAN_POINT ( 'NONE',  ( 4.066846734877469949, -19.79409818376439389, -1.500000000000002220 ) ) ;
#44568 = ORIENTED_EDGE ( 'NONE', *, *, #9583, .T. ) ;
#44569 = CARTESIAN_POINT ( 'NONE',  ( 29.70220533433690946, 3.451715827188561736, 28.20564067601642222 ) ) ;
#44570 = CARTESIAN_POINT ( 'NONE',  ( 1.305682803664691249, 5.965225279485572685, 29.57950906855421991 ) ) ;
#44571 = EDGE_CURVE ( 'NONE', #10266, #44198, #52350, .T. ) ;
#44572 = CARTESIAN_POINT ( 'NONE',  ( -95.54871114897673579, -24.52300882791530512, 0.6510814631126408125 ) ) ;
#44573 = CARTESIAN_POINT ( 'NONE',  ( -99.55766099210418929, -23.73791477778911840, 11.05961554403170588 ) ) ;
#44575 = EDGE_LOOP ( 'NONE', ( #97855, #9544, #37657, #75408 ) ) ;
#44574 = CARTESIAN_POINT ( 'NONE',  ( -13.24026558610970916, 16.85365899302435722, 11.49999999999999645 ) ) ;
#44576 = CARTESIAN_POINT ( 'NONE',  ( -77.52287095715007581, -23.48783264082476308, -1.443836473390091912 ) ) ;
#44577 = B_SPLINE_CURVE_WITH_KNOTS ( 'NONE', 3,
 ( #15221, #39566, #49569, #34337, #26219, #92837 ),
 .UNSPECIFIED., .F., .F.,
 ( 4, 2, 4 ),
 ( 0.000000000000000000, 0.001380764517854766050, 0.002761529035709532100 ),
 .UNSPECIFIED. ) ;
#44578 = CARTESIAN_POINT ( 'NONE',  ( -41.62371455830013645, -24.65952944569304606, 1.056160979905696351 ) ) ;
#44579 = EDGE_LOOP ( 'NONE', ( #6241, #62204, #26145 ) ) ;
#44580 = CARTESIAN_POINT ( 'NONE',  ( -20.69558417703438025, 1.077208295497980250, -1.500000000000002220 ) ) ;
#44581 = AXIS2_PLACEMENT_3D ( 'NONE', #73626, #72137, #96956 ) ;
#44582 = ORIENTED_EDGE ( 'NONE', *, *, #50600, .F. ) ;
#44583 = EDGE_CURVE ( 'NONE', #33754, #28964, #15562, .T. ) ;
#44584 = LINE ( 'NONE', #59311, #4866 ) ;
#44585 = ORIENTED_EDGE ( 'NONE', *, *, #97162, .T. ) ;
#44586 = CARTESIAN_POINT ( 'NONE',  ( 4.334227700317904386, -5.876774720514401196, 18.30971318885719157 ) ) ;
#44587 = ORIENTED_EDGE ( 'NONE', *, *, #16893, .T. ) ;
#44588 = CARTESIAN_POINT ( 'NONE',  ( -2.639205680565387624, -20.84613592336672028, -1.500000000000002220 ) ) ;
#44589 = CARTESIAN_POINT ( 'NONE',  ( 6.372119535971386917, -21.01724095701019479, 11.49999999999999645 ) ) ;
#44590 = AXIS2_PLACEMENT_3D ( 'NONE', #9890, #87016, #40841 ) ;
#44591 = CARTESIAN_POINT ( 'NONE',  ( -73.60710170687688958, -23.48786465467241058, 11.44779295918254824 ) ) ;
#44592 = CARTESIAN_POINT ( 'NONE',  ( -17.96456891314058879, -13.58578184957126034, 11.49999999999998934 ) ) ;
#44593 = AXIS2_PLACEMENT_3D ( 'NONE', #82860, #36697, #68151 ) ;
#44594 = CARTESIAN_POINT ( 'NONE',  ( -11.48448384864204996, -17.54081393385053644, 11.49999999999998934 ) ) ;
#44595 = CARTESIAN_POINT ( 'NONE',  ( 5.641575934020636396, -5.876774720514419847, 20.76276410292889096 ) ) ;
#44596 = DIRECTION ( 'NONE',  ( 4.015954566446630556E-15, -1.000000000000000000, 1.297050502119899750E-15 ) ) ;
#44597 = DIRECTION ( 'NONE',  ( -0.6599726524652340665, 3.117967031984456719E-15, 0.7512896232465900992 ) ) ;
#44598 = ORIENTED_EDGE ( 'NONE', *, *, #62086, .T. ) ;
#44599 = ORIENTED_EDGE ( 'NONE', *, *, #60450, .T. ) ;
#44600 = EDGE_LOOP ( 'NONE', ( #61992, #9405, #27722, #59381 ) ) ;
#44601 = CARTESIAN_POINT ( 'NONE',  ( -66.63617382715514736, -24.15543982623906771, -0.2315651400026688400 ) ) ;
#44602 = EDGE_CURVE ( 'NONE', #42281, #57513, #65355, .T. ) ;
#44603 = CARTESIAN_POINT ( 'NONE',  ( -10.41973078503355588, 18.78793304046337198, -1.500000000000002220 ) ) ;
#44604 = DIRECTION ( 'NONE',  ( -0.000000000000000000, 2.173523156925979552E-06, -0.9999999999976378895 ) ) ;
#44605 = ORIENTED_EDGE ( 'NONE', *, *, #522, .T. ) ;
#44606 = CARTESIAN_POINT ( 'NONE',  ( -9.620199658202244208, 18.81650055922726494, -1.500000000000002220 ) ) ;
#44607 = CARTESIAN_POINT ( 'NONE',  ( -52.62287095715006302, -23.72773821059535493, 11.05748984161097503 ) ) ;
#44608 = CARTESIAN_POINT ( 'NONE',  ( -64.64155661987921064, -23.96119346886879953, -0.6495511937832134652 ) ) ;
#44609 = EDGE_CURVE ( 'NONE', #74213, #39929, #21663, .T. ) ;
#44610 = CARTESIAN_POINT ( 'NONE',  ( -83.56309760437380874, -23.48786465467241058, 11.44779295918254469 ) ) ;
#44611 = CARTESIAN_POINT ( 'NONE',  ( -29.49875734969025842, 0.3587747205144262708, 23.37402280011862743 ) ) ;
#44612 = CARTESIAN_POINT ( 'NONE',  ( -69.55126625704998844, -25.16221347177320666, 3.076695569926833684 ) ) ;
#44613 = CARTESIAN_POINT ( 'NONE',  ( 1.014068502963303864, -22.09113584270698993, -1.500000000000002220 ) ) ;
#44614 = CARTESIAN_POINT ( 'NONE',  ( -81.49976054116859814, -24.66019654487198665, 8.947790411086131712 ) ) ;
#44615 = VERTEX_POINT ( 'NONE', #75956 ) ;
#44616 = CARTESIAN_POINT ( 'NONE',  ( -56.52287095715006870, -23.47596703998600631, 11.44779298504228926 ) ) ;
#44617 = PLANE ( 'NONE',  #37864 ) ;
#44618 = CARTESIAN_POINT ( 'NONE',  ( -24.90875734969025501, 6.475225279485573360, 29.49402280011861777 ) ) ;
#44619 = EDGE_CURVE ( 'NONE', #54649, #93563, #387, .T. ) ;
#44620 = EDGE_CURVE ( 'NONE', #72780, #21913, #6958, .T. ) ;
#44621 = CARTESIAN_POINT ( 'NONE',  ( -100.6412016622194727, -23.48783264082476663, -1.443836473390090358 ) ) ;
#44622 = CARTESIAN_POINT ( 'NONE',  ( -15.52061920455031618, -11.66286593722069931, 11.49999999999998934 ) ) ;
#44623 = VECTOR ( 'NONE', #25817, 1000.000000000000000 ) ;
#44624 = CARTESIAN_POINT ( 'NONE',  ( -7.638042729800005759, 19.97414216180626667, -1.500000000000002220 ) ) ;
#44625 = CARTESIAN_POINT ( 'NONE',  ( -61.62287095715004881, -29.50250786944525672, 11.44777988621623876 ) ) ;
#44626 = PLANE ( 'NONE',  #96575 ) ;
#44627 = CARTESIAN_POINT ( 'NONE',  ( -6.499999999999992895, 3.299745742347187193E-16, 2.100000000000000977 ) ) ;
#44628 = CARTESIAN_POINT ( 'NONE',  ( -5.366453405989236813, 1.999999999999998224, 18.24068255301867936 ) ) ;
#44629 = CARTESIAN_POINT ( 'NONE',  ( -22.62345309801473547, -0.4825844212548152656, -1.500000000000002220 ) ) ;
#44630 = ORIENTED_EDGE ( 'NONE', *, *, #92459, .F. ) ;
#44631 = CARTESIAN_POINT ( 'NONE',  ( 4.329581153495547063, -5.876774720514422512, 21.24220543808225869 ) ) ;
#44632 = CARTESIAN_POINT ( 'NONE',  ( -102.5228709571500758, -24.64965694238407323, 8.947790433994194714 ) ) ;
#44633 = CARTESIAN_POINT ( 'NONE',  ( 1.028332004353105233, 19.75660188889424518, 11.49999999999999645 ) ) ;
#44634 = LINE ( 'NONE', #98400, #22865 ) ;
#44635 =( BOUNDED_SURFACE ( )  B_SPLINE_SURFACE ( 3, 2, ( 
 ( #21296, #29915, #100403 ),
 ( #37035, #30916, #67995 ),
 ( #76577, #99904, #30416 ),
 ( #60882, #51770, #53268 ),
 ( #77078, #21787, #15190 ),
 ( #46152, #5583, #98923 ),
 ( #22784, #91317, #52765 ),
 ( #14688, #53772, #38529 ),
 ( #84197, #67496, #29414 ),
 ( #60395, #45160, #98418 ) ),
 .UNSPECIFIED., .F., .F., .T. ) 
 B_SPLINE_SURFACE_WITH_KNOTS ( ( 4, 2, 2, 2, 4 ),
 ( 3, 3 ),
 ( -1.454863790203986262E-16, 9.770668801556799598E-05, 0.0001954133760312814648, 0.0002931200640469949336, 0.0003908267520627084295 ),
 ( 0.000000000000000000, 1.000000000000000000 ),
 .UNSPECIFIED. ) 
 GEOMETRIC_REPRESENTATION_ITEM ( )  RATIONAL_B_SPLINE_SURFACE ( (
 ( 1.000000000000000000, 0.8096947957034197341, 1.000000000000000000),
 ( 1.000000000000000000, 0.8369431042627567541, 1.000000000000000000),
 ( 1.000000000000000000, 0.8633772427686626783, 1.000000000000000000),
 ( 1.000000000000000000, 0.9107640641016462313, 1.000000000000000000),
 ( 1.000000000000000000, 0.9319105126974177589, 1.000000000000000000),
 ( 1.000000000000000000, 0.9655776140384774164, 1.000000000000000000),
 ( 1.000000000000000000, 0.9783528158684996479, 1.000000000000000000),
 ( 1.000000000000000000, 0.9955824377509593370, 1.000000000000000000),
 ( 1.000000000000000000, 1.000024029240739631, 1.000000000000000000),
 ( 1.000000000000000000, 1.000000000000000000, 1.000000000000000000) ) ) 
 REPRESENTATION_ITEM ( '' )  SURFACE ( )  );
#44636 = CARTESIAN_POINT ( 'NONE',  ( -35.58953762381673158, -25.00158670708909270, 2.256160236439166411 ) ) ;
#44637 = EDGE_CURVE ( 'NONE', #60030, #39828, #97265, .T. ) ;
#44638 = ORIENTED_EDGE ( 'NONE', *, *, #67775, .F. ) ;
#44639 = CARTESIAN_POINT ( 'NONE',  ( -78.62287095715005592, -29.50247984919015209, -1.443849546365053582 ) ) ;
#44640 = FACE_OUTER_BOUND ( 'NONE', #28872, .T. ) ;
#44641 = CARTESIAN_POINT ( 'NONE',  ( 4.348677445931066643, 21.19853102677161871, -1.500000000000002220 ) ) ;
#44642 = CARTESIAN_POINT ( 'NONE',  ( -49.73634623139758304, -25.10935161048781339, 2.988891661266243283 ) ) ;
#44643 = CARTESIAN_POINT ( 'NONE',  ( -1.608633542659107629, -19.34071428503001755, -1.500000000000002220 ) ) ;
#44644 = DIRECTION ( 'NONE',  ( 0.000000000000000000, -2.173523156925980399E-06, 0.9999999999976378895 ) ) ;
#44645 = DIRECTION ( 'NONE',  ( -3.773278334453079618E-23, 0.9999999999976377785, 2.173523156925979975E-06 ) ) ;
#44646 = CARTESIAN_POINT ( 'NONE',  ( 18.24360591643979035, -7.691401616277519615, -1.500000000000002220 ) ) ;
#44647 = ORIENTED_EDGE ( 'NONE', *, *, #19522, .F. ) ;
#44648 = CARTESIAN_POINT ( 'NONE',  ( -15.70679263237263434, -12.88635299011707502, 11.49999999999999645 ) ) ;
#44649 = LINE ( 'NONE', #75578, #39173 ) ;
#44650 = CIRCLE ( 'NONE', #96499, 2.000000000000000000 ) ;
#44651 = ADVANCED_FACE ( 'NONE', ( #45533 ), #75896, .T. ) ;
#44652 = CIRCLE ( 'NONE', #10683, 0.3000000000000016542 ) ;
#44653 = DIRECTION ( 'NONE',  ( 3.639962309748244178E-15, 1.000000000000000000, -2.135627652102599075E-15 ) ) ;
#44654 = ADVANCED_FACE ( 'NONE', ( #47030 ), #24175, .F. ) ;
#44655 = VERTEX_POINT ( 'NONE', #71370 ) ;
#44656 = CARTESIAN_POINT ( 'NONE',  ( -102.6235477340627256, -24.66019654487200086, 8.947790411086115725 ) ) ;
#44657 = CARTESIAN_POINT ( 'NONE',  ( 14.78484767477524819, -5.152774720514425866, -28.43034250232787485 ) ) ;
#44658 = CARTESIAN_POINT ( 'NONE',  ( -7.160000000000000142, 8.786681894035815787, 6.233837718258663507 ) ) ;
#44659 = CARTESIAN_POINT ( 'NONE',  ( -110.5228709571500758, -23.47593901973090524, -1.443836447538996204 ) ) ;
#44660 = AXIS2_PLACEMENT_3D ( 'NONE', #40744, #64108, #10293 ) ;
#44661 = CARTESIAN_POINT ( 'NONE',  ( -31.52287095715008292, -24.33927499327854349, 9.819080762295818943 ) ) ;
#44662 = CARTESIAN_POINT ( 'NONE',  ( 3.315226082619958881, 19.80964767386612380, -1.500000000000002220 ) ) ;
#44663 = EDGE_CURVE ( 'NONE', #24863, #61929, #78255, .T. ) ;
#44664 = AXIS2_PLACEMENT_3D ( 'NONE', #54575, #2298, #69799 ) ;
#44665 = CARTESIAN_POINT ( 'NONE',  ( 13.91401389203221406, -3.316774720514426456, 158.0376437107427137 ) ) ;
#44666 = VERTEX_POINT ( 'NONE', #49039 ) ;
#44667 = CARTESIAN_POINT ( 'NONE',  ( -117.6228709571500275, -24.33927499327853994, 9.819080762295810061 ) ) ;
#44668 = VECTOR ( 'NONE', #82246, 1000.000000000000114 ) ;
#44669 = EDGE_CURVE ( 'NONE', #4924, #66877, #47531, .T. ) ;
#44670 = B_SPLINE_CURVE_WITH_KNOTS ( 'NONE', 3,
 ( #59485, #90427, #20902, #82805, #33401, #9568, #56270, #64393, #85696, #16177, #63887, #94297, #40534, #1470, #71484, #78561 ),
 .UNSPECIFIED., .F., .F.,
 ( 4, 2, 2, 2, 2, 2, 2, 4 ),
 ( 6.992893892674702526E-18, 0.0002048719647680148778, 0.0004097439295360227624, 0.0008194878590720570174, 0.001024359823840074795, 0.001229231788608092357, 0.001434103753376110351, 0.001638975718144127913 ),
 .UNSPECIFIED. ) ;
#44671 = ADVANCED_FACE ( 'NONE', ( #40909 ), #94183, .T. ) ;
#44672 = CARTESIAN_POINT ( 'NONE',  ( 9.452765381649220089, 20.79790602042944414, 11.49999999999999645 ) ) ;
#44673 = CARTESIAN_POINT ( 'NONE',  ( -102.5228709571500758, -24.33832256527048088, 0.1851278514138648412 ) ) ;
#44674 = CARTESIAN_POINT ( 'NONE',  ( -82.62287095715005592, -24.65952944569304606, 1.056160979905699016 ) ) ;
#44675 = LINE ( 'NONE', #68504, #1465 ) ;
#44676 = DIRECTION ( 'NONE',  ( -3.773278334453079030E-23, 0.9999999999976377785, 2.173523156925979128E-06 ) ) ;
#44677 = CARTESIAN_POINT ( 'NONE',  ( -117.5562042904833930, -23.47596703998600631, 11.44779298504227683 ) ) ;
#44678 = CARTESIAN_POINT ( 'NONE',  ( -73.52287095715007581, -23.47593901973090169, -1.443836447538996870 ) ) ;
#44679 = ORIENTED_EDGE ( 'NONE', *, *, #7319, .F. ) ;
#44680 = CARTESIAN_POINT ( 'NONE',  ( -17.59887021274124663, -10.25344800880639262, -1.500000000000002220 ) ) ;
#44681 = B_SPLINE_CURVE_WITH_KNOTS ( 'NONE', 3,
 ( #24698, #9484, #24205, #86607 ),
 .UNSPECIFIED., .F., .F.,
 ( 4, 4 ),
 ( 1.387778780781445676E-17, 0.0001000000000000028508 ),
 .UNSPECIFIED. ) ;
#44682 = ORIENTED_EDGE ( 'NONE', *, *, #39586, .T. ) ;
#44683 = B_SPLINE_CURVE_WITH_KNOTS ( 'NONE', 3,
 ( #96496, #88899, #97496, #28477 ),
 .UNSPECIFIED., .F., .F.,
 ( 4, 4 ),
 ( 0.4691036948738852019, 0.4701044419146508946 ),
 .UNSPECIFIED. ) ;
#44684 = CARTESIAN_POINT ( 'NONE',  ( 15.56936346670522120, 16.85858822313069894, -1.500000000000002220 ) ) ;
#44685 = CARTESIAN_POINT ( 'NONE',  ( -8.376690734369036662, 12.50000000000004974, 0.000000000000000000 ) ) ;
#44686 = ORIENTED_EDGE ( 'NONE', *, *, #73265, .F. ) ;
#44687 = CARTESIAN_POINT ( 'NONE',  ( -108.5519249696069579, -24.35071581493544457, 9.817618358456016381 ) ) ;
#44688 = CARTESIAN_POINT ( 'NONE',  ( -77.64260741054584969, -23.73791477778911840, 11.05961554403170588 ) ) ;
#44689 = CARTESIAN_POINT ( 'NONE',  ( -40.62287095715007013, -24.62226745350437440, 0.9660975649728171799 ) ) ;
#44691 = EDGE_LOOP ( 'NONE', ( #23497, #15887, #11015, #72193 ) ) ;
#44690 = CARTESIAN_POINT ( 'NONE',  ( 17.81766572339076404, -11.58780717566545526, 11.49999999999999645 ) ) ;
#44692 = AXIS2_PLACEMENT_3D ( 'NONE', #9211, #55915, #71630 ) ;
#44693 = ORIENTED_EDGE ( 'NONE', *, *, #29316, .T. ) ;
#44694 = CARTESIAN_POINT ( 'NONE',  ( -15.96568504569681402, -15.38390974582250692, 11.49999999999998934 ) ) ;
#44695 = CARTESIAN_POINT ( 'NONE',  ( 6.296002175621457475, 19.65409743616946514, 11.49999999999998934 ) ) ;
#44696 = VERTEX_POINT ( 'NONE', #17064 ) ;
#44697 = ORIENTED_EDGE ( 'NONE', *, *, #34197, .F. ) ;
#44698 = CARTESIAN_POINT ( 'NONE',  ( 10.34999999999999254, 2.573529411764703845, 1.544117647058823151 ) ) ;
#44699 = CARTESIAN_POINT ( 'NONE',  ( -121.6228709571500701, -23.73907113216991860, -1.053371485793222595 ) ) ;
#44700 = ORIENTED_EDGE ( 'NONE', *, *, #52589, .T. ) ;
#44701 = EDGE_LOOP ( 'NONE', ( #92248, #35095 ) ) ;
#44702 = CARTESIAN_POINT ( 'NONE',  ( -124.4728709570019873, -25.30556170156495455, 4.804051544042280852 ) ) ;
#44703 = CARTESIAN_POINT ( 'NONE',  ( -111.5203643720066680, -23.73791477778912551, 11.05961554403170055 ) ) ;
#44704 = CARTESIAN_POINT ( 'NONE',  ( 15.99960863614693274, -3.577630190449808012, -27.91116951066528173 ) ) ;
#44705 = CARTESIAN_POINT ( 'NONE',  ( 2.677173591928626806, -20.63698567995287902, -1.500000000000002220 ) ) ;
#44706 = CARTESIAN_POINT ( 'NONE',  ( -0.2038501785326352067, 21.78777694363981254, 11.49999999999999645 ) ) ;
#44707 = CARTESIAN_POINT ( 'NONE',  ( -51.32890343732908889, -25.08217282722072738, 7.322960462340015297 ) ) ;
#44708 = CARTESIAN_POINT ( 'NONE',  ( -77.62287095715007013, -23.48786465467241413, 11.44779295918254469 ) ) ;
#44709 = CARTESIAN_POINT ( 'NONE',  ( -115.5877649471882904, -24.83618233451451118, 1.606449574219534826 ) ) ;
#44710 = CARTESIAN_POINT ( 'NONE',  ( -17.93832129671990572, 13.47109510200611560, 11.49999999999998934 ) ) ;
#44711 = CARTESIAN_POINT ( 'NONE',  ( 33.00535138976592719, -3.570691370340881576, -12.97242311383975988 ) ) ;
#44712 = ORIENTED_EDGE ( 'NONE', *, *, #92415, .F. ) ;
#44713 = PLANE ( 'NONE',  #58260 ) ;
#44714 = CARTESIAN_POINT ( 'NONE',  ( 32.15269211224249091, 4.540774720514427543, 3.401810532325273417 ) ) ;
#44715 = VERTEX_POINT ( 'NONE', #16057 ) ;
#44716 = VERTEX_POINT ( 'NONE', #55650 ) ;
#44717 = CARTESIAN_POINT ( 'NONE',  ( -99.83817514626852585, -25.31070701350142116, 5.349196373867116883 ) ) ;
#44718 = EDGE_LOOP ( 'NONE', ( #63325, #78300, #10344, #20618, #99332, #31416, #78910, #93262, #650, #75764, #82625, #13296, #34340, #16971, #38951, #60794, #76881, #51814, #84262, #69704 ) ) ;
#44719 = AXIS2_PLACEMENT_3D ( 'NONE', #97212, #83978, #37808 ) ;
#44720 = EDGE_CURVE ( 'NONE', #3112, #49156, #18377, .T. ) ;
#44721 = CARTESIAN_POINT ( 'NONE',  ( -15.80959461918071618, 14.24510877297761446, -1.500000000000002220 ) ) ;
#44722 = ORIENTED_EDGE ( 'NONE', *, *, #76328, .T. ) ;
#44723 = DIRECTION ( 'NONE',  ( 0.000000000000000000, 0.000000000000000000, -1.000000000000000000 ) ) ;
#44724 = TOROIDAL_SURFACE ( 'NONE', #15517, 132.8284398600581540, 2.040000000000000036 ) ;
#44725 = CARTESIAN_POINT ( 'NONE',  ( 15.37114825158464271, 14.37155165002682544, 11.49999999999998934 ) ) ;
#44726 = CARTESIAN_POINT ( 'NONE',  ( -55.52287095715006870, -23.47596703998600631, 11.44779298504228926 ) ) ;
#44727 = LINE ( 'NONE', #99979, #67977 ) ;
#44728 = AXIS2_PLACEMENT_3D ( 'NONE', #87180, #32902, #47131 ) ;
#44729 = CARTESIAN_POINT ( 'NONE',  ( -65.52287095715006160, -24.91570333825770334, 8.075032458260364976 ) ) ;
#44730 = CARTESIAN_POINT ( 'NONE',  ( 17.58553779993395594, 13.13030503331179411, -1.500000000000002220 ) ) ;
#44731 = LINE ( 'NONE', #14257, #18785 ) ;
#44732 = ORIENTED_EDGE ( 'NONE', *, *, #75809, .F. ) ;
#44733 = CARTESIAN_POINT ( 'NONE',  ( -40.09699101898657148, -25.29459747820068571, 5.519299892252927719 ) ) ;
#44734 = VECTOR ( 'NONE', #40514, 1000.000000000000000 ) ;
#44735 = EDGE_CURVE ( 'NONE', #27813, #19391, #78453, .T. ) ;
#44736 = EDGE_CURVE ( 'NONE', #63555, #32994, #87079, .T. ) ;
#44737 = CIRCLE ( 'NONE', #51258, 0.3000000000000016542 ) ;
#44738 = EDGE_CURVE ( 'NONE', #7487, #76771, #5232, .T. ) ;
#44739 = CARTESIAN_POINT ( 'NONE',  ( -84.51016183175109120, -24.15620529776628445, 10.23563542870660292 ) ) ;
#44740 = CARTESIAN_POINT ( 'NONE',  ( -27.25988310792305214, 5.965225279485572685, 30.32664379231667695 ) ) ;
#44741 = EDGE_CURVE ( 'NONE', #31278, #33587, #93184, .T. ) ;
#44742 = CARTESIAN_POINT ( 'NONE',  ( 3.252401863874215593, -0.3587747205143964613, -29.35688408629929214 ) ) ;
#44743 = CARTESIAN_POINT ( 'NONE',  ( 1.764508054474889009, 21.21474994468914943, -1.500000000000002220 ) ) ;
#44744 = LINE ( 'NONE', #29003, #95281 ) ;
#44745 = CARTESIAN_POINT ( 'NONE',  ( -107.5924962624403207, -23.96169478059713853, 10.65365249895717348 ) ) ;
#44746 = CARTESIAN_POINT ( 'NONE',  ( -89.52287095715009002, -24.66019654487200441, 8.947790411086119278 ) ) ;
#44747 = CARTESIAN_POINT ( 'NONE',  ( -70.52287095715011844, -24.82558206586151073, 1.605769216559629342 ) ) ;
#44748 = CARTESIAN_POINT ( 'NONE',  ( -20.52357230491503159, 9.176553703681571861, -1.500000000000002220 ) ) ;
#44749 = CYLINDRICAL_SURFACE ( 'NONE', #89565, 0.1000000000000000472 ) ;
#44750 = ORIENTED_EDGE ( 'NONE', *, *, #6591, .T. ) ;
#44751 = CARTESIAN_POINT ( 'NONE',  ( -98.94665561451864733, -25.22304042422490511, 6.503500078851421229 ) ) ;
#44752 = CARTESIAN_POINT ( 'NONE',  ( -18.14765110722914798, -7.448729197826248871, 11.49999999999999645 ) ) ;
#44753 = CARTESIAN_POINT ( 'NONE',  ( -99.13316617824068544, -25.28856576242281662, 4.187040092130447810 ) ) ;
#44754 = CARTESIAN_POINT ( 'NONE',  ( -82.52287095715004739, -23.73907113217677889, -1.053371485781116723 ) ) ;
#44755 = EDGE_CURVE ( 'NONE', #30329, #69394, #95996, .T. ) ;
#44756 = VERTEX_POINT ( 'NONE', #16555 ) ;
#44757 = CARTESIAN_POINT ( 'NONE',  ( -88.62862753172657904, -24.35071581493543746, 9.817618358456025263 ) ) ;
#44758 = DIRECTION ( 'NONE',  ( 0.000000000000000000, 0.000000000000000000, 1.000000000000000000 ) ) ;
#44759 = LINE ( 'NONE', #52367, #72365 ) ;
#44760 = VECTOR ( 'NONE', #82690, 1000.000000000000227 ) ;
#44761 = CARTESIAN_POINT ( 'NONE',  ( -51.52287095715005449, -24.66019654487199375, 8.947790411086119278 ) ) ;
#44763 = EDGE_CURVE ( 'NONE', #90373, #46797, #82695, .T. ) ;
#44762 = CARTESIAN_POINT ( 'NONE',  ( 3.669390655483735220, -19.36157329643844704, 11.49999999999998934 ) ) ;
#44764 = ORIENTED_EDGE ( 'NONE', *, *, #68587, .T. ) ;
#44765 = B_SPLINE_CURVE_WITH_KNOTS ( 'NONE', 3,
 ( #6353, #45921, #30681, #53539 ),
 .UNSPECIFIED., .F., .F.,
 ( 4, 4 ),
 ( 0.000000000000000000, 1.000000000000000000 ),
 .UNSPECIFIED. ) ;
#44766 = CARTESIAN_POINT ( 'NONE',  ( -108.5562042904833930, -23.47596703998600631, 11.44779298504227683 ) ) ;
#44767 = CARTESIAN_POINT ( 'NONE',  ( -41.32836283488544638, 2.682774720514426559, 39.26872235229541985 ) ) ;
#44768 = EDGE_CURVE ( 'NONE', #91326, #12744, #59141, .T. ) ;
#44769 = APPROVAL_DATE_TIME ( #69602, #47590 ) ;
#44770 = ORIENTED_EDGE ( 'NONE', *, *, #44290, .T. ) ;
#44771 = DIRECTION ( 'NONE',  ( -1.000000000000000000, -4.476705744456278313E-16, 0.000000000000000000 ) ) ;
#44772 = CARTESIAN_POINT ( 'NONE',  ( -1.380763273332680896, -6.376774720514418959, 20.28973052848695602 ) ) ;
#44773 = CARTESIAN_POINT ( 'NONE',  ( -107.6228709571500701, -24.66019654487199730, 8.947790411086124607 ) ) ;
#44774 = PLANE ( 'NONE',  #676 ) ;
#44775 = CARTESIAN_POINT ( 'NONE',  ( -119.6228709571500559, -29.50248528299804818, 1.056150453629045360 ) ) ;
#44776 = CARTESIAN_POINT ( 'NONE',  ( -99.62287095715016960, -23.96177878511308634, 10.65340807706329684 ) ) ;
#44777 = CARTESIAN_POINT ( 'NONE',  ( -127.5228709571500616, -24.64898659630368627, 1.056161002820834804 ) ) ;
#44778 = CARTESIAN_POINT ( 'NONE',  ( 4.555139465550277933, 19.45931829295258453, -1.500000000000002220 ) ) ;
#44779 = EDGE_CURVE ( 'NONE', #56245, #31023, #91242, .T. ) ;
#44780 = CARTESIAN_POINT ( 'NONE',  ( -127.6228709571500559, -24.64898659630368627, 1.056161002820834804 ) ) ;
#44781 = CARTESIAN_POINT ( 'NONE',  ( -45.58194095766508980, -24.73531770709095312, 8.716586749053515604 ) ) ;
#44782 = ORIENTED_EDGE ( 'NONE', *, *, #64574, .T. ) ;
#44783 = CARTESIAN_POINT ( 'NONE',  ( 4.647438682898014761, -6.376774720514417183, 20.26932200457894950 ) ) ;
#44784 = CIRCLE ( 'NONE', #17183, 251.4258649670780699 ) ;
#44785 = ADVANCED_FACE ( 'NONE', ( #35307 ), #4844, .T. ) ;
#44786 = CARTESIAN_POINT ( 'NONE',  ( -119.5185327869307059, -24.34968618360934656, 0.1864209137778924941 ) ) ;
#44787 = LINE ( 'NONE', #84325, #15118 ) ;
#44788 = LINE ( 'NONE', #91437, #20228 ) ;
#44789 = CARTESIAN_POINT ( 'NONE',  ( -39.54608221933844447, -24.15543982623906416, -0.2315651400026678131 ) ) ;
#44790 = EDGE_CURVE ( 'NONE', #78621, #31830, #42432, .T. ) ;
#44791 = DIRECTION ( 'NONE',  ( -1.000000000000000000, -0.000000000000000000, -5.238131417152343399E-15 ) ) ;
#44792 = CARTESIAN_POINT ( 'NONE',  ( -1.501937386944296460, -6.376774720514415407, 19.86422795159478483 ) ) ;
#44793 = AXIS2_PLACEMENT_3D ( 'NONE', #86810, #41153, #49276 ) ;
#44794 = FACE_OUTER_BOUND ( 'NONE', #99858, .T. ) ;
#44796 = VECTOR ( 'NONE', #92585, 1000.000000000000114 ) ;
#44795 = DIRECTION ( 'NONE',  ( -3.773278334453079618E-23, 0.9999999999976377785, 2.173523156925979975E-06 ) ) ;
#44797 = ORIENTED_EDGE ( 'NONE', *, *, #96784, .F. ) ;
#44798 = AXIS2_PLACEMENT_3D ( 'NONE', #90990, #89007, #52440 ) ;
#44799 = CARTESIAN_POINT ( 'NONE',  ( -20.21730713243277933, 1.494317884549376974, 11.49999999999998934 ) ) ;
#44800 = DIRECTION ( 'NONE',  ( -3.773278334453079618E-23, 0.9999999999976377785, 2.173523156925979975E-06 ) ) ;
#44801 = CARTESIAN_POINT ( 'NONE',  ( -53.62287095715004881, -23.48783264082478084, -1.443836473390070596 ) ) ;
#44802 = AXIS2_PLACEMENT_3D ( 'NONE', #81597, #12068, #19185 ) ;
#44803 = CARTESIAN_POINT ( 'NONE',  ( -118.6228709571500559, -29.50250243563736774, 8.947779886222134493 ) ) ;
#44804 = VERTEX_POINT ( 'NONE', #35798 ) ;
#44805 = DIRECTION ( 'NONE',  ( 0.000000000000000000, 1.000000000000000000, -0.000000000000000000 ) ) ;
#44806 = DIRECTION ( 'NONE',  ( 3.773278334444166432E-23, -1.000000000000000000, 0.000000000000000000 ) ) ;
#44807 = CARTESIAN_POINT ( 'NONE',  ( -4.889416449700032530, -19.50743224814450016, -1.500000000000002220 ) ) ;
#44808 = CARTESIAN_POINT ( 'NONE',  ( -20.60145385712877797, -4.430719527714695793, 11.49999999999999645 ) ) ;
#44809 = DIRECTION ( 'NONE',  ( 0.000000000000000000, -1.000000000000000000, 0.000000000000000000 ) ) ;
#44810 = CARTESIAN_POINT ( 'NONE',  ( -70.62753707971197059, -24.83644354573578994, 8.397322867130100121 ) ) ;
#44811 = CARTESIAN_POINT ( 'NONE',  ( -16.84257673422482426, -14.26466048179180568, -1.500000000000002220 ) ) ;
#44812 = B_SPLINE_CURVE_WITH_KNOTS ( 'NONE', 3,
 ( #43662, #5589, #51775, #58888, #89830, #27440 ),
 .UNSPECIFIED., .F., .F.,
 ( 4, 2, 4 ),
 ( 6.391158118963033910E-06, 0.001387004593080786580, 0.002767618028042609802 ),
 .UNSPECIFIED. ) ;
#44813 = CARTESIAN_POINT ( 'NONE',  ( 11.66944253441096002, 16.90307425063352298, 11.49999999999998934 ) ) ;
#44814 = CARTESIAN_POINT ( 'NONE',  ( -35.62287095715005592, -24.99132157543083821, 2.256160258750667502 ) ) ;
#44815 = CARTESIAN_POINT ( 'NONE',  ( -35.62287095715005592, -29.50248528299804818, 1.056150453629031594 ) ) ;
#44816 = ORIENTED_EDGE ( 'NONE', *, *, #99542, .T. ) ;
#44817 = DIRECTION ( 'NONE',  ( 0.000000000000000000, 0.000000000000000000, -1.000000000000000000 ) ) ;
#44818 = ORIENTED_EDGE ( 'NONE', *, *, #35629, .F. ) ;
#44819 = CARTESIAN_POINT ( 'NONE',  ( -99.30746832622341458, -25.20873971062084706, 3.386897128527919243 ) ) ;
#44820 = CARTESIAN_POINT ( 'NONE',  ( -129.9395376238167046, -23.47596703998600631, 11.44779298504227860 ) ) ;
#44821 = ORIENTED_EDGE ( 'NONE', *, *, #12466, .T. ) ;
#44822 = EDGE_LOOP ( 'NONE', ( #12691, #70141, #78600, #76993, #48941 ) ) ;
#44823 = CARTESIAN_POINT ( 'NONE',  ( -65.62287095715005592, -23.48783264082478084, -1.443836473390067265 ) ) ;
#44824 = CARTESIAN_POINT ( 'NONE',  ( -31.62287095715005236, -23.47593901973091235, -1.443836447539013301 ) ) ;
#44825 = CARTESIAN_POINT ( 'NONE',  ( -0.3225169060639742624, -6.376774720514411854, 19.46611907402017749 ) ) ;
#44826 = CARTESIAN_POINT ( 'NONE',  ( -7.762539992054180438, 19.06225842855939234, -1.500000000000002220 ) ) ;
#44827 = CARTESIAN_POINT ( 'NONE',  ( 18.49883484089910723, -11.16122333755292750, 11.49999999999999645 ) ) ;
#44828 = VERTEX_POINT ( 'NONE', #81971 ) ;
#44829 = CARTESIAN_POINT ( 'NONE',  ( -99.17846093192173385, -25.28926427284505607, 4.366343918064007568 ) ) ;
#44830 = VECTOR ( 'NONE', #86501, 1000.000000000000114 ) ;
#44831 = CARTESIAN_POINT ( 'NONE',  ( -4.465079497292244959, -6.376774720514410077, 19.29815762497054976 ) ) ;
#44832 = CARTESIAN_POINT ( 'NONE',  ( 10.24050353823403192, -19.87907451059620456, -1.500000000000002220 ) ) ;
#44833 = CARTESIAN_POINT ( 'NONE',  ( -34.52287095715006160, -23.48786465467240347, 11.44779295918255357 ) ) ;
#44834 = CARTESIAN_POINT ( 'NONE',  ( -52.62287095715005592, -29.50250243563736774, 8.947779886222146928 ) ) ;
#44835 = EDGE_LOOP ( 'NONE', ( #24706, #85970, #96851, #50844 ) ) ;
#44836 = CARTESIAN_POINT ( 'NONE',  ( 282.9764569301858046, -5.965225279485572685, 20.79159422840526616 ) ) ;
#44837 = CARTESIAN_POINT ( 'NONE',  ( -49.64567687034262633, -23.96169478059712432, 10.65365249895718414 ) ) ;
#44838 = CIRCLE ( 'NONE', #27018, 91.74549126261076992 ) ;
#44839 = CARTESIAN_POINT ( 'NONE',  ( 20.36350155627077640, -4.707376482769925374, 11.49999999999998934 ) ) ;
#44840 = ORIENTED_EDGE ( 'NONE', *, *, #52750, .F. ) ;
#44842 = ORIENTED_EDGE ( 'NONE', *, *, #35016, .F. ) ;
#44841 = CARTESIAN_POINT ( 'NONE',  ( -67.50569153577386317, -24.15620529776628800, 10.23563542870660115 ) ) ;
#44843 = ORIENTED_EDGE ( 'NONE', *, *, #81320, .F. ) ;
#44844 = CARTESIAN_POINT ( 'NONE',  ( -100.5497400620557187, -24.52399227489127398, 9.353111116836526406 ) ) ;
#44845 = CARTESIAN_POINT ( 'NONE',  ( 20.77832821955112408, -3.674247523096572099, -1.500000000000002220 ) ) ;
#44846 = ORIENTED_EDGE ( 'NONE', *, *, #72565, .T. ) ;
#44847 = CARTESIAN_POINT ( 'NONE',  ( -117.5555609497473597, -23.96119346886881019, -0.6495511937831994764 ) ) ;
#44849 = ADVANCED_FACE ( 'NONE', ( #96689 ), #89086, .F. ) ;
#44848 = DIRECTION ( 'NONE',  ( 0.000000000000000000, 0.9999999999976377785, 2.173523156925979128E-06 ) ) ;
#44850 = CARTESIAN_POINT ( 'NONE',  ( 9.495391690522565042, 19.61495305411445500, 11.49999999999998934 ) ) ;
#44851 = CARTESIAN_POINT ( 'NONE',  ( 9.782958569640028301, -0.6681657214399144840, 19.30000000000000071 ) ) ;
#44852 = ADVANCED_FACE ( 'NONE', ( #73367 ), #11458, .T. ) ;
#44853 = CARTESIAN_POINT ( 'NONE',  ( -81.62287095715005592, -24.64898659630528854, 1.056161002820826145 ) ) ;
#44854 = DIRECTION ( 'NONE',  ( 0.8219392559241307517, -0.5637660281018076480, -0.08114015731558694988 ) ) ;
#44855 = CARTESIAN_POINT ( 'NONE',  ( 11.36066313177254905, -18.55813952095733654, -1.500000000000002220 ) ) ;
#44856 = CARTESIAN_POINT ( 'NONE',  ( -71.39239612577370053, -25.24674124963215505, 5.186401910093661805 ) ) ;
#44858 = VERTEX_POINT ( 'NONE', #26185 ) ;
#44857 = CARTESIAN_POINT ( 'NONE',  ( 3.003370282714790562, 22.13870467353671856, 11.49999999999999645 ) ) ;
#44859 = CARTESIAN_POINT ( 'NONE',  ( -45.62287095715004170, -24.92579138211019085, 1.929029949965659130 ) ) ;
#44860 = CARTESIAN_POINT ( 'NONE',  ( -117.5228709571500758, -23.72747288104470087, -1.053458166803225682 ) ) ;
#44861 = LINE ( 'NONE', #92015, #94264 ) ;
#44862 = ORIENTED_EDGE ( 'NONE', *, *, #37769, .F. ) ;
#44863 = EDGE_CURVE ( 'NONE', #3925, #12606, #40285, .T. ) ;
#44864 = EDGE_CURVE ( 'NONE', #53293, #75504, #26987, .T. ) ;
#44865 = AXIS2_PLACEMENT_3D ( 'NONE', #48512, #79440, #93154 ) ;
#44866 = VERTEX_POINT ( 'NONE', #12449 ) ;
#44867 = VERTEX_POINT ( 'NONE', #64781 ) ;
#44868 = LINE ( 'NONE', #53485, #56231 ) ;
#44869 = CARTESIAN_POINT ( 'NONE',  ( -10.94853654022341516, 18.13385389444049522, -1.500000000000002220 ) ) ;
#44870 = DIRECTION ( 'NONE',  ( 0.000000000000000000, -0.000000000000000000, 1.000000000000000000 ) ) ;
#44871 = CARTESIAN_POINT ( 'NONE',  ( 30.63935204725980554, -3.888906929512149446, 28.25823861891851507 ) ) ;
#44872 = CARTESIAN_POINT ( 'NONE',  ( -64.62287095715005592, -29.50247984919015209, -1.443849546365056913 ) ) ;
#44873 = VECTOR ( 'NONE', #86102, 999.9999999999998863 ) ;
#44874 = CARTESIAN_POINT ( 'NONE',  ( 33.34043384136949584, 4.658726884274782876, -12.67806891602221064 ) ) ;
#44875 = CARTESIAN_POINT ( 'NONE',  ( -9.899997732206244905, -16.63842163800745766, 11.49999999999998934 ) ) ;
#44876 = EDGE_CURVE ( 'NONE', #63805, #60463, #28252, .T. ) ;
#44877 = CARTESIAN_POINT ( 'NONE',  ( -38.52287095715006870, -24.64898659630367206, 1.056161002820819261 ) ) ;
#44878 = VERTEX_POINT ( 'NONE', #13442 ) ;
#44879 = AXIS2_PLACEMENT_3D ( 'NONE', #15859, #70158, #641 ) ;
#44880 = CARTESIAN_POINT ( 'NONE',  ( 6.036767712469883307, 18.47306877840545170, 11.49999999999999645 ) ) ;
#44881 = LINE ( 'NONE', #51987, #47105 ) ;
#44882 = AXIS2_PLACEMENT_3D ( 'NONE', #71939, #96756, #72436 ) ;
#44883 = ORIENTED_EDGE ( 'NONE', *, *, #11460, .T. ) ;
#44884 = CARTESIAN_POINT ( 'NONE',  ( 3.051095722660301934, -5.876774720514410077, 19.07493897947323092 ) ) ;
#44885 = PLANE ( 'NONE',  #91185 ) ;
#44886 = DIRECTION ( 'NONE',  ( 0.000000000000000000, 0.000000000000000000, -1.000000000000000000 ) ) ;
#44887 = VECTOR ( 'NONE', #45133, 1000.000000000000000 ) ;
#44888 = CARTESIAN_POINT ( 'NONE',  ( 26.73860345374794178, -5.334136533370936739, -4.444819549327402086 ) ) ;
#44889 = CARTESIAN_POINT ( 'NONE',  ( -19.37001648656083574, -3.113731218521536004, 11.49999999999998934 ) ) ;
#44890 = CARTESIAN_POINT ( 'NONE',  ( -46.58714575211884323, -24.34968618360932879, 0.1864209137778778391 ) ) ;
#44891 = ORIENTED_EDGE ( 'NONE', *, *, #66071, .F. ) ;
#44892 = CARTESIAN_POINT ( 'NONE',  ( 16.61904782137575154, -13.72857183568914685, -1.500000000000002220 ) ) ;
#44893 = MANIFOLD_SOLID_BREP ( 'Kes-Ekstr\X2\00fc\X0\zyon28', #82466 ) ;
#44894 = DIRECTION ( 'NONE',  ( 0.000000000000000000, 0.000000000000000000, 1.000000000000000000 ) ) ;
#44895 = CARTESIAN_POINT ( 'NONE',  ( -119.6228709571500559, -29.50250786944525672, 11.44777988621622811 ) ) ;
#44896 = DIRECTION ( 'NONE',  ( 3.773278334444166432E-23, -1.000000000000000000, 0.000000000000000000 ) ) ;
#44897 = CARTESIAN_POINT ( 'NONE',  ( -99.92039718326317654, -25.27473246999687007, 3.410800712176911720 ) ) ;
#44898 = CARTESIAN_POINT ( 'NONE',  ( 22.88022663504679599, 2.825535151426334934, -1.500000000000002220 ) ) ;
#44899 = CALENDAR_DATE ( 2026, 9, 10 ) ;
#44900 = CARTESIAN_POINT ( 'NONE',  ( 32.25183987940364005, -6.376774720514426953, 2.026414261721653176 ) ) ;
#44901 = CARTESIAN_POINT ( 'NONE',  ( -129.6228709571500133, -23.48783264082478794, -1.443836473390056607 ) ) ;
#44902 = CARTESIAN_POINT ( 'NONE',  ( -13.64458216870221818, 14.86554040878868044, 11.49999999999999645 ) ) ;
#44903 = CARTESIAN_POINT ( 'NONE',  ( -84.62287095715005592, -23.72773821059536559, 11.05748984161097503 ) ) ;
#44904 = PLANE ( 'NONE',  #27433 ) ;
#44905 = CARTESIAN_POINT ( 'NONE',  ( -89.62287095715004170, -29.50250786944525672, 11.44777988621623344 ) ) ;
#44906 = LINE ( 'NONE', #14429, #47287 ) ;
#44907 = CARTESIAN_POINT ( 'NONE',  ( -30.64751926837171325, -23.47596703998600631, 11.44779298504228038 ) ) ;
#44908 = CARTESIAN_POINT ( 'NONE',  ( 7.211006999188390942, 18.53272205163514030, -1.500000000000002220 ) ) ;
#44909 = CARTESIAN_POINT ( 'NONE',  ( -113.5517726272361045, -24.51314013834315375, 0.6176544820404169522 ) ) ;
#44910 = CARTESIAN_POINT ( 'NONE',  ( -8.281543130087330340, -17.94227898472161797, -1.500000000000002220 ) ) ;
#44911 = AXIS2_PLACEMENT_3D ( 'NONE', #13756, #28494, #99492 ) ;
#44912 = CARTESIAN_POINT ( 'NONE',  ( -29.49875734969025842, -0.3587747205144265483, 17.86602280011862476 ) ) ;
#44913 = EDGE_CURVE ( 'NONE', #86, #29751, #81553, .T. ) ;
#44914 = CARTESIAN_POINT ( 'NONE',  ( -125.6228709571500275, -24.14406661707773338, 10.28769366152062226 ) ) ;
#44915 = DIRECTION ( 'NONE',  ( 1.000000000000000000, -1.734723475976800981E-15, 0.000000000000000000 ) ) ;
#44916 = CARTESIAN_POINT ( 'NONE',  ( -17.42616458466809704, -11.11377323884725321, 11.49999999999999645 ) ) ;
#44917 = CIRCLE ( 'NONE', #17305, 6.594667762285749468 ) ;
#44918 = DIRECTION ( 'NONE',  ( -3.773278334453079030E-23, 0.9999999999976377785, 2.173523156925979128E-06 ) ) ;
#44919 = EDGE_CURVE ( 'NONE', #9882, #57723, #79938, .T. ) ;
#44920 = DIRECTION ( 'NONE',  ( -3.773278334444166432E-23, 1.000000000000000000, 0.000000000000000000 ) ) ;
#44921 = CARTESIAN_POINT ( 'NONE',  ( -35.55620429048339304, -23.47596703998600276, 11.44779298504227505 ) ) ;
#44922 = CARTESIAN_POINT ( 'NONE',  ( 22.16846167567618053, -4.910139430472912458, 11.49999999999999645 ) ) ;
#44923 = ORIENTED_EDGE ( 'NONE', *, *, #17458, .T. ) ;
#44924 = B_SPLINE_SURFACE_WITH_KNOTS ( 'NONE', 3, 3, ( 
 ( #30455, #60424, #7618, #14718 ),
 ( #38568, #68030, #84232, #69525 ),
 ( #91848, #6114, #91349, #84736 ),
 ( #46183, #21824, #45685, #76608 ),
 ( #52800, #15225, #69017, #54309 ),
 ( #7, #30950, #83734, #61916 ),
 ( #99942, #61419, #77613, #92843 ) ),
 .UNSPECIFIED., .F., .F., .F.,
 ( 4, 3, 4 ),
 ( 4, 4 ),
 ( 0.7945040050992243641, 0.8970133687736503436, 0.9995227324480764342 ),
 ( 0.7896946696024070844, 0.7910719696203489804 ),
 .UNSPECIFIED. ) ;
#44925 = FACE_OUTER_BOUND ( 'NONE', #61214, .T. ) ;
#44926 = CARTESIAN_POINT ( 'NONE',  ( 30.59918777245023236, 5.333550415411136392, 26.68477081578061316 ) ) ;
#44927 = CARTESIAN_POINT ( 'NONE',  ( 0.4983251850863967269, 20.17815531296474418, 11.49999999999998934 ) ) ;
#44928 = CARTESIAN_POINT ( 'NONE',  ( -63.62365437609576446, -24.65952944569304250, 1.056160979905695463 ) ) ;
#44929 = DIRECTION ( 'NONE',  ( -3.773278334453079618E-23, 0.9999999999976377785, 2.173523156925979975E-06 ) ) ;
#44930 = ORIENTED_EDGE ( 'NONE', *, *, #91785, .F. ) ;
#44931 = VECTOR ( 'NONE', #79557, 1000.000000000000114 ) ;
#44932 = ORIENTED_EDGE ( 'NONE', *, *, #34236, .T. ) ;
#44933 = CARTESIAN_POINT ( 'NONE',  ( -101.3738023147422780, -29.50249165161862663, 3.986241424695394109 ) ) ;
#44934 = CARTESIAN_POINT ( 'NONE',  ( 21.91704834537361180, 6.644925864936762849, 11.49999999999998934 ) ) ;
#44935 = CARTESIAN_POINT ( 'NONE',  ( -6.660000000000001030, 0.000000000000000000, 0.000000000000000000 ) ) ;
#44936 = CARTESIAN_POINT ( 'NONE',  ( 0.9236959384754221958, 21.56878955078795812, -1.500000000000002220 ) ) ;
#44937 = CARTESIAN_POINT ( 'NONE',  ( -123.5918554517772918, -23.48783264082477373, -1.443836473390086361 ) ) ;
#44938 = CARTESIAN_POINT ( 'NONE',  ( -34.52200860028750640, -23.48783264082478084, -1.443836473390076591 ) ) ;
#44939 = CARTESIAN_POINT ( 'NONE',  ( 20.83135763335140922, 1.668377004047274959, 11.49999999999999645 ) ) ;
#44940 = ORIENTED_EDGE ( 'NONE', *, *, #73942, .T. ) ;
#44941 = DIRECTION ( 'NONE',  ( 1.000000000000000000, -0.000000000000000000, -0.000000000000000000 ) ) ;
#44942 = CARTESIAN_POINT ( 'NONE',  ( 9.413913215453616701, -19.89622248225912315, -1.500000000000002220 ) ) ;
#44943 = VECTOR ( 'NONE', #37456, 1000.000000000000000 ) ;
#44944 = CARTESIAN_POINT ( 'NONE',  ( -105.5855865933814215, -24.92592662359561473, 8.075495903017998245 ) ) ;
#44945 = CARTESIAN_POINT ( 'NONE',  ( -41.68940843163829868, -25.29087182211354090, 3.512445110864212516 ) ) ;
#44946 = ORIENTED_EDGE ( 'NONE', *, *, #49409, .F. ) ;
#44947 = CARTESIAN_POINT ( 'NONE',  ( 3.879812756903532556, -6.376774720514401196, 18.16163344421570969 ) ) ;
#44948 = CARTESIAN_POINT ( 'NONE',  ( -90.58933947920019136, -24.52399227489127398, 9.353111116836531735 ) ) ;
#44949 = VERTEX_POINT ( 'NONE', #83452 ) ;
#44950 = CARTESIAN_POINT ( 'NONE',  ( -93.52287095715006160, -23.47596703998600631, 11.44779298504228393 ) ) ;
#44951 = VERTEX_POINT ( 'NONE', #15436 ) ;
#44952 = AXIS2_PLACEMENT_3D ( 'NONE', #65976, #88795, #51222 ) ;
#44953 = ORIENTED_EDGE ( 'NONE', *, *, #56244, .F. ) ;
#44954 = DIRECTION ( 'NONE',  ( 0.000000000000000000, -0.000000000000000000, -1.000000000000000000 ) ) ;
#44955 = FACE_OUTER_BOUND ( 'NONE', #51145, .T. ) ;
#44956 = CARTESIAN_POINT ( 'NONE',  ( -57.63244684718339528, -24.34968618360933590, 0.1864209137778796155 ) ) ;
#44957 = CARTESIAN_POINT ( 'NONE',  ( -18.16121111207539940, 9.348575961806686152, -1.500000000000002220 ) ) ;
#44958 = VERTEX_POINT ( 'NONE', #76333 ) ;
#44959 = CARTESIAN_POINT ( 'NONE',  ( -3.108425644221024520, -5.876774720514414518, 20.25188360057253334 ) ) ;
#44960 = CARTESIAN_POINT ( 'NONE',  ( -115.6228709571500701, -24.14406661707771207, 10.28769366152061160 ) ) ;
#44961 = B_SPLINE_CURVE_WITH_KNOTS ( 'NONE', 3,
 ( #98105, #18994, #34729, #3303, #35732, #81404, #74771, #73297, #36226, #49973, #66704, #11387, #11883, #82391, #34235, #42365 ),
 .UNSPECIFIED., .F., .F.,
 ( 4, 2, 2, 2, 2, 2, 2, 4 ),
 ( 0.000000000000000000, 0.0002722372812524201055, 0.0005444745625048402109, 0.001088949125009681506, 0.001361186406262094185, 0.001633423687514507297, 0.001905660968766919976, 0.002177898250019332654 ),
 .UNSPECIFIED. ) ;
#44962 = CARTESIAN_POINT ( 'NONE',  ( -4.289200894924355190, -6.376774720514413630, 19.85590024959437017 ) ) ;
#44963 = CARTESIAN_POINT ( 'NONE',  ( -25.63531995026274402, -24.86348392168161681, 6.224458436948604678 ) ) ;
#44964 = ORIENTED_EDGE ( 'NONE', *, *, #39985, .T. ) ;
#44965 = DIRECTION ( 'NONE',  ( -1.000000000000000000, -3.491481338843133355E-15, -2.352173255807796056E-16 ) ) ;
#44966 = CARTESIAN_POINT ( 'NONE',  ( -29.21927636257191807, -25.26247907303463336, 7.471890645913414453 ) ) ;
#44967 = CARTESIAN_POINT ( 'NONE',  ( 2.040502595053849788, 20.68626321094233944, -1.500000000000002220 ) ) ;
#44968 = VERTEX_POINT ( 'NONE', #45908 ) ;
#44970 = ORIENTED_EDGE ( 'NONE', *, *, #22030, .F. ) ;
#44969 = DIRECTION ( 'NONE',  ( 0.000000000000000000, -0.000000000000000000, 1.000000000000000000 ) ) ;
#44971 = CARTESIAN_POINT ( 'NONE',  ( 1.949999999999999734, 0.1924999999999993938, 0.1925000000000007261 ) ) ;
#44972 = ORIENTED_EDGE ( 'NONE', *, *, #59889, .F. ) ;
#44973 = ORIENTED_EDGE ( 'NONE', *, *, #60446, .T. ) ;
#44974 = CARTESIAN_POINT ( 'NONE',  ( 22.81105451610979173, -1.475225279485572916, -19.61691820600746539 ) ) ;
#44976 = EDGE_CURVE ( 'NONE', #41736, #47247, #61141, .T. ) ;
#44975 = DIRECTION ( 'NONE',  ( -0.000000000000000000, 1.000000000000000000, -0.000000000000000000 ) ) ;
#44977 = DIRECTION ( 'NONE',  ( 0.5473052603538087757, -5.646564643389147554E-15, 0.8369330630277725946 ) ) ;
#44978 = CARTESIAN_POINT ( 'NONE',  ( -105.6228709571500559, -23.47593901973091235, -1.443836447538999312 ) ) ;
#44979 = CARTESIAN_POINT ( 'NONE',  ( -92.58855183542770817, -24.35071581493543391, 9.817618358456025263 ) ) ;
#44980 = CARTESIAN_POINT ( 'NONE',  ( -95.55620429048339304, -23.47596703998600631, 11.44779298504227683 ) ) ;
#44982 = ORIENTED_EDGE ( 'NONE', *, *, #86723, .T. ) ;
#44981 = CARTESIAN_POINT ( 'NONE',  ( -21.88945651911318535, 3.243594245096953710, 11.49999999999999645 ) ) ;
#44983 = CARTESIAN_POINT ( 'NONE',  ( -108.5535964976718333, -24.15543982623908192, -0.2315651400026445539 ) ) ;
#44984 = EDGE_CURVE ( 'NONE', #30443, #75862, #38276, .T. ) ;
#44985 = CARTESIAN_POINT ( 'NONE',  ( -21.16596634977960179, 8.012090315382277339, 11.49999999999998934 ) ) ;
#44986 = VECTOR ( 'NONE', #5773, 1000.000000000000000 ) ;
#44987 = ADVANCED_FACE ( 'NONE', ( #60643 ), #75838, .F. ) ;
#44989 = ORIENTED_EDGE ( 'NONE', *, *, #11216, .F. ) ;
#44988 = CARTESIAN_POINT ( 'NONE',  ( -115.6302133932577334, -23.85049219812686871, 10.88485053497526778 ) ) ;
#44990 = EDGE_CURVE ( 'NONE', #77156, #18231, #90573, .T. ) ;
#44991 = EDGE_LOOP ( 'NONE', ( #12099, #59719, #99839, #36940 ) ) ;
#44992 = AXIS2_PLACEMENT_3D ( 'NONE', #28650, #66740, #21023 ) ;
#44993 = ADVANCED_FACE ( 'NONE', ( #99172 ), #92560, .F. ) ;
#44994 = LINE ( 'NONE', #12526, #40183 ) ;
#44995 = CARTESIAN_POINT ( 'NONE',  ( -11.83016301840747175, -16.26703346747452983, -1.500000000000002220 ) ) ;
#44996 = DIRECTION ( 'NONE',  ( 0.000000000000000000, 0.000000000000000000, 1.000000000000000000 ) ) ;
#44997 = ORIENTED_EDGE ( 'NONE', *, *, #98696, .T. ) ;
#44998 = B_SPLINE_CURVE_WITH_KNOTS ( 'NONE', 3,
 ( #30164, #94061, #14437, #45409 ),
 .UNSPECIFIED., .F., .F.,
 ( 4, 4 ),
 ( 0.9294473336260299368, 0.9304480806667954074 ),
 .UNSPECIFIED. ) ;
#44999 = CARTESIAN_POINT ( 'NONE',  ( 2.499999999999988454, 22.00000000000000000, 2.100000000000000089 ) ) ;
#45000 = CARTESIAN_POINT ( 'NONE',  ( -21.40455707349245529, -6.346402434563959361, -1.500000000000002220 ) ) ;
#45001 = ADVANCED_FACE ( 'NONE', ( #6828 ), #22045, .F. ) ;
#45002 = ORIENTED_EDGE ( 'NONE', *, *, #29941, .F. ) ;
#45003 = ORIENTED_EDGE ( 'NONE', *, *, #86156, .F. ) ;
#45004 = DIRECTION ( 'NONE',  ( -1.000000000000000000, -0.000000000000000000, 0.000000000000000000 ) ) ;
#45005 = CARTESIAN_POINT ( 'NONE',  ( 31.82032313667048484, -6.376774720514426953, 9.148483289431936782 ) ) ;
#45006 = CARTESIAN_POINT ( 'NONE',  ( -65.05438548721848235, -5.356774720514425603, 0.7300228001186309656 ) ) ;
#45007 = CARTESIAN_POINT ( 'NONE',  ( -63.52287095715009002, -23.73907113216989728, -1.053371485793251239 ) ) ;
#45008 = CIRCLE ( 'NONE', #12540, 21.89999999999999858 ) ;
#45009 = DIRECTION ( 'NONE',  ( 1.156482317317878549E-14, 0.000000000000000000, 1.000000000000000000 ) ) ;
#45010 = CARTESIAN_POINT ( 'NONE',  ( 8.254404603115069960, -17.72612730319335839, -1.500000000000002220 ) ) ;
#45011 = CARTESIAN_POINT ( 'NONE',  ( -47.52287095715006160, -23.48783264083458988, -1.443836473374825236 ) ) ;
#45012 = CARTESIAN_POINT ( 'NONE',  ( 14.45597713831175035, -15.85640774750547344, 11.49999999999998934 ) ) ;
#45013 = CARTESIAN_POINT ( 'NONE',  ( -25.60037597819128763, -24.92775154704442286, 3.875572922187972225 ) ) ;
#45014 = PLANE ( 'NONE',  #27625 ) ;
#45015 = DIRECTION ( 'NONE',  ( -0.000000000000000000, 1.000000000000000000, -0.000000000000000000 ) ) ;
#45016 = CARTESIAN_POINT ( 'NONE',  ( 13.72848742581335912, -18.28091200367991576, -1.500000000000002220 ) ) ;
#45017 = CIRCLE ( 'NONE', #11039, 1.249999999999996003 ) ;
#45018 = DATE_AND_TIME ( #28780, #82926 ) ;
#45019 = CARTESIAN_POINT ( 'NONE',  ( -106.6344572697143462, -23.48786465467241769, 11.44779295918253581 ) ) ;
#45020 = CARTESIAN_POINT ( 'NONE',  ( -125.5895376238167245, -23.48783264082479505, -1.443836473390057273 ) ) ;
#45021 = CARTESIAN_POINT ( 'NONE',  ( -19.24466553037914807, -5.328869878250761971, 11.49999999999999645 ) ) ;
#45022 = CARTESIAN_POINT ( 'NONE',  ( -111.5562042904833930, -23.47593901973091235, -1.443836447538999312 ) ) ;
#45023 = AXIS2_PLACEMENT_3D ( 'NONE', #17165, #48131, #95295 ) ;
#45024 = CARTESIAN_POINT ( 'NONE',  ( -74.63034837134625832, -24.35071581493544102, 9.817618358456019934 ) ) ;
#45025 = DIRECTION ( 'NONE',  ( 0.000000000000000000, 1.000000000000000000, 0.000000000000000000 ) ) ;
#45026 = ORIENTED_EDGE ( 'NONE', *, *, #99188, .F. ) ;
#45027 = DIRECTION ( 'NONE',  ( 0.000000000000000000, -0.9999999999976377785, -2.173523156925979128E-06 ) ) ;
#45028 = EDGE_CURVE ( 'NONE', #13059, #95824, #59716, .T. ) ;
#45029 = DIRECTION ( 'NONE',  ( -0.000000000000000000, -0.000000000000000000, -1.000000000000000000 ) ) ;
#45030 = CARTESIAN_POINT ( 'NONE',  ( -16.45766974254678061, 14.19212061201335473, -1.500000000000002220 ) ) ;
#45031 = CARTESIAN_POINT ( 'NONE',  ( -77.55620429048339304, -24.66019654487199730, 8.947790411086124607 ) ) ;
#45032 = CARTESIAN_POINT ( 'NONE',  ( -10.75157073690095721, 16.42123490324765811, -1.500000000000002220 ) ) ;
#45033 = LINE ( 'NONE', #6951, #63707 ) ;
#45034 = EDGE_CURVE ( 'NONE', #85354, #1776, #18537, .T. ) ;
#45035 = ORIENTED_EDGE ( 'NONE', *, *, #9060, .F. ) ;
#45036 = ITEM_DEFINED_TRANSFORMATION ( 'NONE', 'NONE', #26155,  #37391 ) ;
#45037 = LINE ( 'NONE', #75955, #62974 ) ;
#45038 = CARTESIAN_POINT ( 'NONE',  ( 3.113719597313231002, -5.876774720514426065, 21.58936759753562029 ) ) ;
#45039 = CARTESIAN_POINT ( 'NONE',  ( -14.05295919346176170, -14.94737400546395456, 11.49999999999999645 ) ) ;
#45040 = DIRECTION ( 'NONE',  ( -1.334402673828313093E-16, 0.000000000000000000, -1.000000000000000000 ) ) ;
#45041 = CARTESIAN_POINT ( 'NONE',  ( -93.52287095715009002, -23.48783264082477018, -1.443836473390088360 ) ) ;
#45042 = VERTEX_POINT ( 'NONE', #67255 ) ;
#45043 = EDGE_CURVE ( 'NONE', #9013, #20503, #36682, .T. ) ;
#45044 = DIRECTION ( 'NONE',  ( 0.000000000000000000, -1.000000000000000000, 0.000000000000000000 ) ) ;
#45045 = DIRECTION ( 'NONE',  ( 0.000000000000000000, 0.000000000000000000, -1.000000000000000000 ) ) ;
#45046 = CARTESIAN_POINT ( 'NONE',  ( -78.62287095715005592, -24.64898659630367916, 1.056161002820826145 ) ) ;
#45047 = EDGE_CURVE ( 'NONE', #43147, #73685, #9324, .T. ) ;
#45048 = PLANE ( 'NONE',  #61392 ) ;
#45049 = CARTESIAN_POINT ( 'NONE',  ( 32.48849721025742099, 4.168223360657076881, -0.9137309853436130780 ) ) ;
#45050 = AXIS2_PLACEMENT_3D ( 'NONE', #100232, #85528, #799 ) ;
#45051 = CARTESIAN_POINT ( 'NONE',  ( -3.594920434497504758, 22.80983129501555950, 11.49999999999999645 ) ) ;
#45052 = CARTESIAN_POINT ( 'NONE',  ( -19.53289989604362376, -11.71160353944097920, -1.500000000000002220 ) ) ;
#45053 = CARTESIAN_POINT ( 'NONE',  ( 3.748501943728875574, -6.376774720514426065, 21.47917144995767558 ) ) ;
#45054 = B_SPLINE_SURFACE_WITH_KNOTS ( 'NONE', 3, 3, ( 
 ( #3181, #26507, #4167, #50344 ),
 ( #87903, #57471, #73184, #17889 ),
 ( #25996, #81784, #18386, #65590 ),
 ( #49355, #19870, #19378, #50845 ),
 ( #34121, #3673, #97006, #12255 ),
 ( #49860, #89397, #74172, #66091 ),
 ( #80791, #35618, #72186, #96012 ) ),
 .UNSPECIFIED., .F., .F., .F.,
 ( 4, 3, 4 ),
 ( 4, 4 ),
 ( 0.0004766839783817761926, 0.1029713700210894839, 0.2054660560637971978 ),
 ( 0.4196007365068247785, 0.4208070640716953803 ),
 .UNSPECIFIED. ) ;
#45055 = CARTESIAN_POINT ( 'NONE',  ( -88.52287095715006160, -24.65952944569304606, 1.056160979905700570 ) ) ;
#45056 = CARTESIAN_POINT ( 'NONE',  ( 17.51792015816173986, -0.3587747205144265483, 29.01255224319336889 ) ) ;
#45057 = CARTESIAN_POINT ( 'NONE',  ( -110.9909297185884327, -25.15277794460069671, 6.986250878905948980 ) ) ;
#45058 = CARTESIAN_POINT ( 'NONE',  ( -69.52287095715006160, -24.64898659630367916, 1.056161002820824368 ) ) ;
#45059 = CARTESIAN_POINT ( 'NONE',  ( -8.322136096487577461, -20.27582920440508829, 11.49999999999998934 ) ) ;
#45060 = CC_DESIGN_PERSON_AND_ORGANIZATION_ASSIGNMENT ( #72490, #65893, ( #96051 ) ) ;
#45061 = DIRECTION ( 'NONE',  ( 0.000000000000000000, -1.000000000000000000, 0.000000000000000000 ) ) ;
#45062 = LINE ( 'NONE', #38931, #18703 ) ;
#45063 = CARTESIAN_POINT ( 'NONE',  ( -31.62287095715005236, -29.50247984919015209, -1.443849546365062242 ) ) ;
#45064 = CARTESIAN_POINT ( 'NONE',  ( -49.16098733389834763, -25.13996252305080503, 7.003495811256752468 ) ) ;
#45065 = CARTESIAN_POINT ( 'NONE',  ( -20.77875734969026311, 3.316774720514426456, 29.49402280011862487 ) ) ;
#45066 = CARTESIAN_POINT ( 'NONE',  ( -73.55620429048340725, -23.48786465467241058, 11.44779295918255002 ) ) ;
#45067 = ORIENTED_EDGE ( 'NONE', *, *, #78635, .T. ) ;
#45068 = CARTESIAN_POINT ( 'NONE',  ( 14.97853827808193294, 13.91023239937271860, 11.49999999999998934 ) ) ;
#45069 = VERTEX_POINT ( 'NONE', #77822 ) ;
#45070 = VERTEX_POINT ( 'NONE', #220 ) ;
#45071 = ORIENTED_EDGE ( 'NONE', *, *, #17957, .F. ) ;
#45072 = ORIENTED_EDGE ( 'NONE', *, *, #30185, .T. ) ;
#45073 = CARTESIAN_POINT ( 'NONE',  ( -17.35246277222573141, 15.15038115719275424, -1.500000000000002220 ) ) ;
#45074 = CARTESIAN_POINT ( 'NONE',  ( -95.62287095715005592, -25.00158670708909625, 2.256160236439165967 ) ) ;
#45075 = CARTESIAN_POINT ( 'NONE',  ( 8.147030896810244727, 18.52525024547675869, -1.500000000000002220 ) ) ;
#45076 = ORIENTED_EDGE ( 'NONE', *, *, #86923, .F. ) ;
#45077 = CARTESIAN_POINT ( 'NONE',  ( -28.20286574835018811, -25.11719900286342266, 4.027978703335532096 ) ) ;
#45078 = VECTOR ( 'NONE', #35290, 1000.000000000000114 ) ;
#45079 = CARTESIAN_POINT ( 'NONE',  ( -41.82896759111799412, -25.30795331362449829, 4.562858401357758886 ) ) ;
#45080 = CARTESIAN_POINT ( 'NONE',  ( -89.81226385320381667, -25.32958633408183857, 5.296208831758598023 ) ) ;
#45081 = FACE_OUTER_BOUND ( 'NONE', #74285, .T. ) ;
#45083 = VERTEX_POINT ( 'NONE', #33168 ) ;
#45082 = CARTESIAN_POINT ( 'NONE',  ( -13.99230614532761052, -16.21612836239924960, 11.49999999999999645 ) ) ;
#45084 = DIRECTION ( 'NONE',  ( 0.000000000000000000, -0.000000000000000000, -1.000000000000000000 ) ) ;
#45085 = CARTESIAN_POINT ( 'NONE',  ( -43.62287095715004881, -23.48783264082477729, -1.443836473390071928 ) ) ;
#45086 = ORIENTED_EDGE ( 'NONE', *, *, #24231, .T. ) ;
#45087 = CARTESIAN_POINT ( 'NONE',  ( 8.970943996638910178, -18.66293075132952950, -1.500000000000002220 ) ) ;
#45088 = AXIS2_PLACEMENT_3D ( 'NONE', #69870, #53659, #84586 ) ;
#45090 = VERTEX_POINT ( 'NONE', #70235 ) ;
#45089 = CARTESIAN_POINT ( 'NONE',  ( -80.58953762381671027, -23.48783264082478439, -1.443836473390065489 ) ) ;
#45091 = CARTESIAN_POINT ( 'NONE',  ( -28.65223502837594793, -23.80851314359095738, -0.6495505116914124244 ) ) ;
#45092 = EDGE_LOOP ( 'NONE', ( #65333, #35313, #90660 ) ) ;
#45093 = CARTESIAN_POINT ( 'NONE',  ( 4.912344403463128728, -6.376774720514408301, 19.26008510998990886 ) ) ;
#45094 = AXIS2_PLACEMENT_3D ( 'NONE', #99775, #8954, #30283 ) ;
#45095 = ORIENTED_EDGE ( 'NONE', *, *, #25712, .T. ) ;
#45096 = B_SPLINE_CURVE_WITH_KNOTS ( 'NONE', 3,
 ( #78589, #3498, #16709, #55796 ),
 .UNSPECIFIED., .F., .F.,
 ( 4, 4 ),
 ( 0.000000000000000000, 9.999999999998897304E-05 ),
 .UNSPECIFIED. ) ;
#45097 = CARTESIAN_POINT ( 'NONE',  ( -20.44905293368100985, -4.654758753755802836, -1.500000000000002220 ) ) ;
#45098 = ADVANCED_FACE ( 'NONE', ( #39771 ), #15933, .F. ) ;
#45099 = CARTESIAN_POINT ( 'NONE',  ( 3.092608977599853315, -21.74436839971096802, 11.49999999999999645 ) ) ;
#45100 = DIRECTION ( 'NONE',  ( -3.773278334453080206E-23, 0.9999999999976377785, 2.173523156925979975E-06 ) ) ;
#45101 = CARTESIAN_POINT ( 'NONE',  ( 19.01167203989450982, 12.12494712425435850, -1.500000000000002220 ) ) ;
#45102 = CARTESIAN_POINT ( 'NONE',  ( -0.6469382494902750080, 20.97623560764392181, -1.500000000000002220 ) ) ;
#45103 = DIRECTION ( 'NONE',  ( -0.5630016722799281448, -5.365801633547210331E-16, 0.8264557562326034779 ) ) ;
#45104 = LINE ( 'NONE', #287, #16155 ) ;
#45105 = CARTESIAN_POINT ( 'NONE',  ( 5.727631217150810805, -6.376774720514422512, 21.11407618546790133 ) ) ;
#45106 = ORIENTED_EDGE ( 'NONE', *, *, #34880, .T. ) ;
#45107 = AXIS2_PLACEMENT_3D ( 'NONE', #14938, #6338, #98680 ) ;
#45108 = EDGE_CURVE ( 'NONE', #94513, #18101, #55018, .T. ) ;
#45109 = ORIENTED_EDGE ( 'NONE', *, *, #18183, .F. ) ;
#45110 = ORIENTED_EDGE ( 'NONE', *, *, #66428, .T. ) ;
#45111 = EDGE_CURVE ( 'NONE', #45090, #97756, #70738, .T. ) ;
#45112 = FACE_OUTER_BOUND ( 'NONE', #99729, .T. ) ;
#45113 = CARTESIAN_POINT ( 'NONE',  ( 21.49998558720804809, 0.1351929536555107336, -1.500000000000002220 ) ) ;
#45114 = CARTESIAN_POINT ( 'NONE',  ( -105.5228709571500758, -24.82576562948885979, 8.398263436605498455 ) ) ;
#45115 = VERTEX_POINT ( 'NONE', #48408 ) ;
#45116 = CARTESIAN_POINT ( 'NONE',  ( -7.596101150008887082, -19.70107428960382734, -1.500000000000002220 ) ) ;
#45117 = CARTESIAN_POINT ( 'NONE',  ( 282.9764569301858046, 5.965225279485572685, 20.79159422840526616 ) ) ;
#45118 = CARTESIAN_POINT ( 'NONE',  ( -42.62287095715004881, -29.50248528299804818, 1.056150453629031594 ) ) ;
#45119 = CARTESIAN_POINT ( 'NONE',  ( -100.5228709571500758, -24.52232992886360918, 0.6492154411906000400 ) ) ;
#45120 = DIRECTION ( 'NONE',  ( -1.348230680810989829E-16, 1.000000000000000000, 0.000000000000000000 ) ) ;
#45121 = CARTESIAN_POINT ( 'NONE',  ( -41.92287095715005307, -23.47593901973090169, -1.443836447538997980 ) ) ;
#45122 = CARTESIAN_POINT ( 'NONE',  ( -15.96568504569681402, -15.38390974582250692, -1.500000000000002220 ) ) ;
#45123 = CARTESIAN_POINT ( 'NONE',  ( -81.60466250293514179, -23.48786465467241413, 11.44779295918254824 ) ) ;
#45124 = EDGE_CURVE ( 'NONE', #26773, #83907, #43879, .T. ) ;
#45125 = VERTEX_POINT ( 'NONE', #9831 ) ;
#45126 = CARTESIAN_POINT ( 'NONE',  ( 11.56983764158150407, 6.376774720514426953, 28.29037853177889517 ) ) ;
#45127 = CARTESIAN_POINT ( 'NONE',  ( -58.62287095715007013, -23.47596703998600276, 11.44779298504227683 ) ) ;
#45128 = CARTESIAN_POINT ( 'NONE',  ( -77.52287095715006160, -24.65952944569304606, 1.056160979905698794 ) ) ;
#45129 = CARTESIAN_POINT ( 'NONE',  ( -100.6334234393085154, -24.15503026093918137, -0.2815557561904373229 ) ) ;
#45130 = CARTESIAN_POINT ( 'NONE',  ( -11.39837868854680814, -15.77482985264681403, 11.49999999999998934 ) ) ;
#45131 = CARTESIAN_POINT ( 'NONE',  ( 20.27498964588844643, 6.839650151297337999, -1.500000000000002220 ) ) ;
#45132 = DIRECTION ( 'NONE',  ( 0.000000000000000000, -0.000000000000000000, -1.000000000000000000 ) ) ;
#45133 = DIRECTION ( 'NONE',  ( -0.000000000000000000, -1.000000000000000000, -0.000000000000000000 ) ) ;
#45134 = DIRECTION ( 'NONE',  ( -0.1254312216594016538, 0.000000000000000000, -0.9921023176230513441 ) ) ;
#45135 = CARTESIAN_POINT ( 'NONE',  ( -69.94583503291330828, -25.24888741496607381, 3.680065526283697874 ) ) ;
#45136 = CARTESIAN_POINT ( 'NONE',  ( -3.801653518169780366, -22.29579330195574016, -1.500000000000002220 ) ) ;
#45137 = B_SPLINE_SURFACE_WITH_KNOTS ( 'NONE', 3, 1, ( 
 ( #25136, #85037 ),
 ( #17535, #56119 ),
 ( #31763, #39374 ),
 ( #24636, #79427 ),
 ( #9921, #1319 ),
 ( #39873, #70328 ),
 ( #24142, #62729 ) ),
 .UNSPECIFIED., .F., .F., .F.,
 ( 4, 1, 1, 1, 4 ),
 ( 2, 2 ),
 ( 0.000000000000000000, 0.2193543708254352964, 0.4566051594240339018, 0.7164051918613050240, 1.000000000000000000 ),
 ( 0.000000000000000000, 1.000000000000000000 ),
 .UNSPECIFIED. ) ;
#45138 = ORIENTED_EDGE ( 'NONE', *, *, #57296, .F. ) ;
#45139 = CARTESIAN_POINT ( 'NONE',  ( 4.281508569253434260, -5.876774720514422512, 21.28700241941785265 ) ) ;
#45140 = CARTESIAN_POINT ( 'NONE',  ( -97.55620429048337883, -24.64898659630528499, 1.056161002820831474 ) ) ;
#45141 = CARTESIAN_POINT ( 'NONE',  ( 16.35176858736616978, 11.14859404531058473, 11.49999999999999645 ) ) ;
#45142 = DIRECTION ( 'NONE',  ( 1.000000000000000000, -0.000000000000000000, -0.000000000000000000 ) ) ;
#45143 = ORIENTED_EDGE ( 'NONE', *, *, #19881, .F. ) ;
#45144 = CARTESIAN_POINT ( 'NONE',  ( -37.52287095715006870, -24.66019654487199375, 8.947790411086122830 ) ) ;
#45145 = CARTESIAN_POINT ( 'NONE',  ( -61.64687923781922763, -25.19045605819419364, 3.255062319851647956 ) ) ;
#45146 = CARTESIAN_POINT ( 'NONE',  ( 16.85579979752674618, 13.57973486276658903, -1.500000000000002220 ) ) ;
#45147 = CARTESIAN_POINT ( 'NONE',  ( -27.09174982187060365, -24.78434339138140885, 7.461775111898752755 ) ) ;
#45148 = AXIS2_PLACEMENT_3D ( 'NONE', #44529, #52140, #44020 ) ;
#45149 = CARTESIAN_POINT ( 'NONE',  ( 11.07193147992585835, -15.93265361536492364, -1.500000000000002220 ) ) ;
#45150 = B_SPLINE_CURVE_WITH_KNOTS ( 'NONE', 3,
 ( #67055, #3651, #19358, #27976 ),
 .UNSPECIFIED., .F., .F.,
 ( 4, 4 ),
 ( 0.000000000000000000, 9.999999999994735322E-05 ),
 .UNSPECIFIED. ) ;
#45151 = DIRECTION ( 'NONE',  ( 0.000000000000000000, 1.000000000000000000, 0.000000000000000000 ) ) ;
#45152 = FACE_OUTER_BOUND ( 'NONE', #52828, .T. ) ;
#45153 = CARTESIAN_POINT ( 'NONE',  ( 16.85830656838225039, -10.38424343889589707, 11.49999999999998934 ) ) ;
#45154 = EDGE_CURVE ( 'NONE', #55933, #5623, #71743, .T. ) ;
#45155 = ORIENTED_EDGE ( 'NONE', *, *, #39782, .F. ) ;
#45156 = B_SPLINE_CURVE_WITH_KNOTS ( 'NONE', 3,
 ( #99130, #99621, #22497, #62094 ),
 .UNSPECIFIED., .F., .F.,
 ( 4, 4 ),
 ( 0.000000000000000000, 9.999999999998897304E-05 ),
 .UNSPECIFIED. ) ;
#45157 = CARTESIAN_POINT ( 'NONE',  ( 9.679018533540549640, -17.85022214266596308, 11.49999999999999645 ) ) ;
#45158 = CARTESIAN_POINT ( 'NONE',  ( -111.5895376238167103, -24.66019654487199375, 8.947790411086121054 ) ) ;
#45159 = ADVANCED_FACE ( 'NONE', ( #94062 ), #47904, .F. ) ;
#45160 = CARTESIAN_POINT ( 'NONE',  ( 33.61456970919608978, -3.316774720514426900, -11.35828564741662028 ) ) ;
#45161 = ORIENTED_EDGE ( 'NONE', *, *, #41585, .T. ) ;
#45162 = CARTESIAN_POINT ( 'NONE',  ( -0.07511669896460689000, -22.07755530215571582, 0.1835287498755953650 ) ) ;
#45163 = CARTESIAN_POINT ( 'NONE',  ( -95.52287095715006160, -24.99156044556203327, 7.747789690856173195 ) ) ;
#45164 = CARTESIAN_POINT ( 'NONE',  ( -49.70686029532972583, -25.31601821332649038, 4.960083871316195214 ) ) ;
#45165 = AXIS2_PLACEMENT_3D ( 'NONE', #31680, #9338, #76833 ) ;
#45166 = CARTESIAN_POINT ( 'NONE',  ( -95.62287095715008434, -24.52232992886363050, 0.6492154411906150280 ) ) ;
#45167 = DIRECTION ( 'NONE',  ( -3.773278334453079030E-23, 0.9999999999976377785, 2.173523156925979128E-06 ) ) ;
#45168 = CARTESIAN_POINT ( 'NONE',  ( -2.827821146493835425, 19.88259668395040691, 11.49999999999998934 ) ) ;
#45169 = CARTESIAN_POINT ( 'NONE',  ( -79.62287095715005592, -23.47593901973091235, -1.443836447539004642 ) ) ;
#45170 = EDGE_LOOP ( 'NONE', ( #7688, #82904, #91415, #18452, #90278, #13512, #96753 ) ) ;
#45171 = CARTESIAN_POINT ( 'NONE',  ( -70.52287095715007581, -25.00158670708909625, 2.256160236439166411 ) ) ;
#45172 = VECTOR ( 'NONE', #63524, 1000.000000000000000 ) ;
#45173 = CARTESIAN_POINT ( 'NONE',  ( 15.01570752033863165, -17.30494853738164096, 11.49999999999999645 ) ) ;
#45174 = CARTESIAN_POINT ( 'NONE',  ( -49.94769165354211538, -25.26258863353852746, 4.634773020030235280 ) ) ;
#45175 = DIRECTION ( 'NONE',  ( -0.000000000000000000, -0.000000000000000000, -1.000000000000000000 ) ) ;
#45176 = DIRECTION ( 'NONE',  ( 0.7071067811865476838, 0.000000000000000000, -0.7071067811865474617 ) ) ;
#45177 = CARTESIAN_POINT ( 'NONE',  ( -24.55517127435777525, 0.3587747205143967943, -15.44180958690143157 ) ) ;
#45178 = ADVANCED_FACE ( 'NONE', ( #62634 ), #16942, .F. ) ;
#45179 = CARTESIAN_POINT ( 'NONE',  ( 0.5964549592197740946, 8.529703308962702124, 1.700000000000008837 ) ) ;
#45180 = CARTESIAN_POINT ( 'NONE',  ( -41.86995616089613748, -25.27977532709532227, 4.210709737483026238 ) ) ;
#45181 = EDGE_LOOP ( 'NONE', ( #31985, #52449, #55184, #22891 ) ) ;
#45182 = CARTESIAN_POINT ( 'NONE',  ( 12.22771034161782566, -16.27230226814707947, -1.500000000000002220 ) ) ;
#45183 = ORIENTED_EDGE ( 'NONE', *, *, #61961, .T. ) ;
#45184 = CARTESIAN_POINT ( 'NONE',  ( 2.177599385301639323, -22.86303409451243596, 11.49999999999998934 ) ) ;
#45185 = CARTESIAN_POINT ( 'NONE',  ( -53.01255352321339842, -4.772774720514425972, 35.59556822165056644 ) ) ;
#45187 = VERTEX_POINT ( 'NONE', #87459 ) ;
#45186 = EDGE_CURVE ( 'NONE', #49833, #75137, #73007, .T. ) ;
#45188 = CARTESIAN_POINT ( 'NONE',  ( -7.160000000000000142, 0.1579206558577706254, 7.788828319098143105 ) ) ;
#45189 = CARTESIAN_POINT ( 'NONE',  ( -2.872281323269014752, -16.94322527948557422, 1.999999999999999556 ) ) ;
#45190 = FACE_OUTER_BOUND ( 'NONE', #69089, .T. ) ;
#45192 = ORIENTED_EDGE ( 'NONE', *, *, #31383, .F. ) ;
#45191 = CARTESIAN_POINT ( 'NONE',  ( 7.950249384483326409, 19.69624408967213469, 11.49999999999999645 ) ) ;
#45193 = VERTEX_POINT ( 'NONE', #78330 ) ;
#45194 = CARTESIAN_POINT ( 'NONE',  ( 18.11909884760711975, -12.84011383348296853, 11.49999999999998934 ) ) ;
#45195 = CARTESIAN_POINT ( 'NONE',  ( -19.88974639711211623, -5.441847772814488948, 11.49999999999998934 ) ) ;
#45196 = ORIENTED_EDGE ( 'NONE', *, *, #10854, .T. ) ;
#45197 = EDGE_LOOP ( 'NONE', ( #27134, #71435, #29080, #88145 ) ) ;
#45198 = PLANE ( 'NONE',  #18723 ) ;
#45199 = CARTESIAN_POINT ( 'NONE',  ( 33.61456970919605425, 3.316774720514426900, -11.35828564741663449 ) ) ;
#45200 = VERTEX_POINT ( 'NONE', #1230 ) ;
#45201 = CIRCLE ( 'NONE', #3131, 0.3000000000000016542 ) ;
#45202 = VECTOR ( 'NONE', #18472, 1000.000000000000114 ) ;
#45203 = EDGE_LOOP ( 'NONE', ( #19232, #74050, #22849, #41647 ) ) ;
#45204 = DIRECTION ( 'NONE',  ( 1.000000000000000000, -1.734723475976800981E-15, 0.000000000000000000 ) ) ;
#45205 = LINE ( 'NONE', #60443, #97365 ) ;
#45206 = CARTESIAN_POINT ( 'NONE',  ( 19.72710162658169608, 6.580912942549038469, -1.500000000000002220 ) ) ;
#45207 = ADVANCED_FACE ( 'NONE', ( #77327 ), #32164, .F. ) ;
#45208 = CARTESIAN_POINT ( 'NONE',  ( 1.801620404824296084, -21.73869551012647605, 11.49999999999999645 ) ) ;
#45209 = CARTESIAN_POINT ( 'NONE',  ( -51.92861183494494526, -25.23934194637364214, 6.270802386038849541 ) ) ;
#45210 = CARTESIAN_POINT ( 'NONE',  ( -98.94588073693361707, -25.21331259941279157, 6.500605466382517683 ) ) ;
#45211 = CARTESIAN_POINT ( 'NONE',  ( 1.786768808452938950, -22.39398889530128756, 11.49999999999998934 ) ) ;
#45212 = AXIS2_PLACEMENT_3D ( 'NONE', #78725, #58802, #19719 ) ;
#45213 = CARTESIAN_POINT ( 'NONE',  ( -51.29599548036032530, -25.26334595364517455, 4.016965689284721641 ) ) ;
#45214 = ORIENTED_EDGE ( 'NONE', *, *, #93238, .T. ) ;
#45215 = CARTESIAN_POINT ( 'NONE',  ( -50.52287095715006160, -24.83620972994591725, 8.398175272781367440 ) ) ;
#45216 = CARTESIAN_POINT ( 'NONE',  ( -69.52287095715006160, -24.64965694238407323, 8.947790433994200043 ) ) ;
#45217 = ORIENTED_EDGE ( 'NONE', *, *, #28845, .F. ) ;
#45218 = AXIS2_PLACEMENT_3D ( 'NONE', #69735, #213, #69228 ) ;
#45219 = ORIENTED_EDGE ( 'NONE', *, *, #83892, .F. ) ;
#45221 = EDGE_CURVE ( 'NONE', #12529, #86771, #86456, .T. ) ;
#45220 = CARTESIAN_POINT ( 'NONE',  ( -57.52287095715005449, -29.50248528299804818, 1.056150453629034924 ) ) ;
#45222 = EDGE_LOOP ( 'NONE', ( #54077, #25609, #51755, #33973 ) ) ;
#45223 = CARTESIAN_POINT ( 'NONE',  ( -17.77299844720193533, 11.79293508692305537, -1.500000000000002220 ) ) ;
#45224 = ADVANCED_FACE ( 'NONE', ( #71241 ), #9664, .T. ) ;
#45225 = EDGE_LOOP ( 'NONE', ( #25447, #24240, #73157, #37110, #2809, #18393, #29585, #49565, #1013, #94922, #29209 ) ) ;
#45226 = CARTESIAN_POINT ( 'NONE',  ( -6.602379858799704238, -5.876774720514410966, 19.46575348430202723 ) ) ;
#45227 = CARTESIAN_POINT ( 'NONE',  ( 18.24537196375281312, 10.48796402029766739, -1.500000000000002220 ) ) ;
#45228 = DIRECTION ( 'NONE',  ( -0.9890158633619158257, -0.1478094111296165414, -0.000000000000000000 ) ) ;
#45229 = CIRCLE ( 'NONE', #41994, 1.399999999999998579 ) ;
#45230 = CARTESIAN_POINT ( 'NONE',  ( -99.66660779535885695, -25.22553094076996061, 3.606680058317695448 ) ) ;
#45231 = CARTESIAN_POINT ( 'NONE',  ( -65.52287095715010423, -24.51254535375846544, 9.355368624242132114 ) ) ;
#45232 = CARTESIAN_POINT ( 'NONE',  ( -21.90371867972833542, 1.011951690471867060, -1.500000000000002220 ) ) ;
#45233 = PLANE ( 'NONE',  #20364 ) ;
#45234 = ORIENTED_EDGE ( 'NONE', *, *, #48921, .T. ) ;
#45235 = CARTESIAN_POINT ( 'NONE',  ( -122.5921615827337661, -23.48786465467241769, 11.44779295918253581 ) ) ;
#45236 = EDGE_CURVE ( 'NONE', #87855, #22734, #41288, .T. ) ;
#45237 = ADVANCED_FACE ( 'NONE', ( #11336 ), #69461, .T. ) ;
#45238 = CARTESIAN_POINT ( 'NONE',  ( -120.5228709571500616, -23.47593901973090524, -1.443836447538996204 ) ) ;
#45239 = CARTESIAN_POINT ( 'NONE',  ( -41.62287095715006302, -23.48783264082477729, -1.443836473390071928 ) ) ;
#45240 = CARTESIAN_POINT ( 'NONE',  ( -20.43735050632677286, -23.59307763070868447, 9.703205396196684873 ) ) ;
#45241 = CARTESIAN_POINT ( 'NONE',  ( 20.09692647535021948, 7.048664716645152595, -1.500000000000002220 ) ) ;
#45242 = CARTESIAN_POINT ( 'NONE',  ( -55.62287095715003460, -23.85229601348995132, 10.88205029486210229 ) ) ;
#45243 = LINE ( 'NONE', #68577, #68988 ) ;
#45244 = CARTESIAN_POINT ( 'NONE',  ( -122.5895376238167387, -24.65952944569304961, 1.056160979905702346 ) ) ;
#45245 = CARTESIAN_POINT ( 'NONE',  ( -33.49677881317446548, -24.15543982623906771, -0.2315651400026580431 ) ) ;
#45246 = CARTESIAN_POINT ( 'NONE',  ( 18.89768980500364037, -12.13386209897132773, -1.500000000000002220 ) ) ;
#45247 = CIRCLE ( 'NONE', #69510, 0.8500000000000017542 ) ;
#45248 = CARTESIAN_POINT ( 'NONE',  ( -111.9711973445961917, -25.30561928443788133, 5.929683345795315752 ) ) ;
#45249 = ORIENTED_EDGE ( 'NONE', *, *, #63033, .F. ) ;
#45250 = CARTESIAN_POINT ( 'NONE',  ( -81.52287095715004739, -24.51387760970724372, 9.387446482453407626 ) ) ;
#45251 = CARTESIAN_POINT ( 'NONE',  ( -11.98250242409135780, 15.54504917500377559, 11.49999999999999645 ) ) ;
#45252 = CARTESIAN_POINT ( 'NONE',  ( -125.5228709571500616, -25.00158670708909980, 2.256160236439166411 ) ) ;
#45253 = CARTESIAN_POINT ( 'NONE',  ( -82.52287095715007581, -24.51283580621453950, 0.6167428607046286926 ) ) ;
#45254 = ORIENTED_EDGE ( 'NONE', *, *, #25149, .F. ) ;
#45255 = CARTESIAN_POINT ( 'NONE',  ( -88.64271420608834262, -23.48786465467241413, 11.44779295918254469 ) ) ;
#45256 = DIRECTION ( 'NONE',  ( -1.000000000000000000, -0.000000000000000000, -0.000000000000000000 ) ) ;
#45257 = CARTESIAN_POINT ( 'NONE',  ( -100.2069791292054504, -25.25095787178537421, 5.245324546832492274 ) ) ;
#45258 = CARTESIAN_POINT ( 'NONE',  ( -26.81181828833286929, -24.64042068939468422, 8.032344318642952175 ) ) ;
#45259 = EDGE_CURVE ( 'NONE', #77096, #45042, #67629, .T. ) ;
#45260 = CARTESIAN_POINT ( 'NONE',  ( -5.084378373094740944, 19.06436389234985285, 11.49999999999998934 ) ) ;
#45261 = B_SPLINE_CURVE_WITH_KNOTS ( 'NONE', 3,
 ( #20638, #51606, #14523, #45498, #67334, #68824 ),
 .UNSPECIFIED., .F., .F.,
 ( 4, 2, 4 ),
 ( 6.384118678619663671E-06, 0.001386860460828383008, 0.002767336802978146663 ),
 .UNSPECIFIED. ) ;
#45262 = ORIENTED_EDGE ( 'NONE', *, *, #92720, .T. ) ;
#45263 = PLANE ( 'NONE',  #79674 ) ;
#45264 = CARTESIAN_POINT ( 'NONE',  ( 7.749999999999998224, 24.84999999999999787, 2.100000000000000089 ) ) ;
#45265 = PERSON ( 'NAUO-PER7', 'UNSPECIFIED', 'UNSPECIFIED', ('UNSPECIFIED'), ('UNSPECIFIED'), ('UNSPECIFIED') ) ;
#45266 = EDGE_CURVE ( 'NONE', #4283, #18679, #29046, .T. ) ;
#45267 = PERSON_AND_ORGANIZATION ( #70597, #27821 ) ;
#45268 = VERTEX_POINT ( 'NONE', #100033 ) ;
#45269 = FACE_OUTER_BOUND ( 'NONE', #12506, .T. ) ;
#45270 = CARTESIAN_POINT ( 'NONE',  ( -87.62287095715004170, -24.64965695001468404, 8.947790433994180503 ) ) ;
#45271 = CARTESIAN_POINT ( 'NONE',  ( -55.57991759551926947, -24.83618233451449697, 1.606449574219536602 ) ) ;
#45272 = CARTESIAN_POINT ( 'NONE',  ( -66.52287095715006160, -24.33832256527049154, 0.1851278514138612330 ) ) ;
#45273 = CARTESIAN_POINT ( 'NONE',  ( -7.234140626586239797, -6.376774720514411854, 19.72789237585158162 ) ) ;
#45274 = CIRCLE ( 'NONE', #66373, 1.835999999999993859 ) ;
#45275 = LINE ( 'NONE', #59502, #27872 ) ;
#45276 = DIRECTION ( 'NONE',  ( -1.000000000000000000, 5.782411586589363555E-16, 0.000000000000000000 ) ) ;
#45277 = CARTESIAN_POINT ( 'NONE',  ( 18.82558416981596139, 6.732768832687442639, 11.49999999999998934 ) ) ;
#45278 = CARTESIAN_POINT ( 'NONE',  ( -127.6228709571500275, -24.33832256526968862, 0.1851278514119955865 ) ) ;
#45279 = CARTESIAN_POINT ( 'NONE',  ( -51.04357394935764347, -25.31543073408252553, 4.940877929217665887 ) ) ;
#45280 = VERTEX_POINT ( 'NONE', #37661 ) ;
#45281 = AXIS2_PLACEMENT_3D ( 'NONE', #69041, #39592, #15249 ) ;
#45282 = CARTESIAN_POINT ( 'NONE',  ( 8.868390920966309210, -6.053523946337313610, -26.43277665853620206 ) ) ;
#45283 = AXIS2_PLACEMENT_3D ( 'NONE', #12713, #53295, #13211 ) ;
#45284 = CARTESIAN_POINT ( 'NONE',  ( -119.5211660777647040, -23.73766607897670866, -1.055555164236450016 ) ) ;
#45285 = CARTESIAN_POINT ( 'NONE',  ( -80.50906975063354309, -24.15602025860895807, 10.28564288303536145 ) ) ;
#45286 = CARTESIAN_POINT ( 'NONE',  ( -119.6228709571500417, -24.66019654487199730, 8.947790411086121054 ) ) ;
#45287 = CARTESIAN_POINT ( 'NONE',  ( -39.50524109486579505, -23.96119346886879597, -0.6495511937832144644 ) ) ;
#45288 = CIRCLE ( 'NONE', #14493, 132.8284398600581824 ) ;
#45289 = CARTESIAN_POINT ( 'NONE',  ( -82.52287095715006160, -24.64965694238407323, 8.947790433994198267 ) ) ;
#45290 = CARTESIAN_POINT ( 'NONE',  ( -1.359786310227693251, -6.376774720514417183, 20.62654306927474579 ) ) ;
#45291 = EDGE_CURVE ( 'NONE', #85381, #27980, #43788, .T. ) ;
#45292 = AXIS2_PLACEMENT_3D ( 'NONE', #92502, #31103, #21483 ) ;
#45293 = CARTESIAN_POINT ( 'NONE',  ( -79.62287095715007013, -23.73934037231756733, 11.05740245334329153 ) ) ;
#45294 = PLANE ( 'NONE',  #98734 ) ;
#45295 = ORIENTED_EDGE ( 'NONE', *, *, #30058, .F. ) ;
#45296 = CARTESIAN_POINT ( 'NONE',  ( -8.208445925564873846, -18.52556626786687488, -1.500000000000002220 ) ) ;
#45297 = CARTESIAN_POINT ( 'NONE',  ( -69.38672083999394147, -25.31448181975444811, 5.177778959383253721 ) ) ;
#45298 = DIRECTION ( 'NONE',  ( -1.000000000000000000, -0.000000000000000000, -0.000000000000000000 ) ) ;
#45299 = EDGE_CURVE ( 'NONE', #54223, #90167, #98550, .T. ) ;
#45300 = EDGE_CURVE ( 'NONE', #18147, #7077, #82830, .T. ) ;
#45301 = CARTESIAN_POINT ( 'NONE',  ( -76.62287095715005592, -23.96127896941631619, -0.6493128931037840390 ) ) ;
#45302 = EDGE_CURVE ( 'NONE', #77832, #4993, #30036, .T. ) ;
#45303 = ORIENTED_EDGE ( 'NONE', *, *, #96787, .T. ) ;
#45304 = LINE ( 'NONE', #76225, #66451 ) ;
#45305 = CARTESIAN_POINT ( 'NONE',  ( -63.62287095715003460, -23.72747288104442021, -1.053458166803663110 ) ) ;
#45306 = CARTESIAN_POINT ( 'NONE',  ( -17.50950832565593984, 9.922426906265528146, -1.500000000000002220 ) ) ;
#45307 = CARTESIAN_POINT ( 'NONE',  ( 19.97611676871187569, -6.800378171449690257, 11.49999999999999645 ) ) ;
#45308 = EDGE_CURVE ( 'NONE', #18260, #18475, #44787, .T. ) ;
#45309 = CARTESIAN_POINT ( 'NONE',  ( 2.872281323269014752, 4.293056017849825601, 1.999999999999999556 ) ) ;
#45310 = CARTESIAN_POINT ( 'NONE',  ( -21.88945651911318535, 3.243594245096953710, -1.500000000000002220 ) ) ;
#45311 = CARTESIAN_POINT ( 'NONE',  ( 8.954683214801249846, 18.48387022957959047, 11.49999999999998934 ) ) ;
#45312 = CARTESIAN_POINT ( 'NONE',  ( 1.949999999999999734, 0.1924999999999993938, 0.1925000000000007261 ) ) ;
#45313 = CARTESIAN_POINT ( 'NONE',  ( -53.62287095715004881, -23.96127896941631619, -0.6493128931037915885 ) ) ;
#45314 = ORIENTED_EDGE ( 'NONE', *, *, #35140, .T. ) ;
#45315 = LINE ( 'NONE', #61039, #2314 ) ;
#45316 = EDGE_LOOP ( 'NONE', ( #32736, #86531, #74415, #15102 ) ) ;
#45317 = CARTESIAN_POINT ( 'NONE',  ( -99.65705935873248222, -25.15797155923122119, 3.047568788030539544 ) ) ;
#45318 = B_SPLINE_SURFACE_WITH_KNOTS ( 'NONE', 3, 3, ( 
 ( #32404, #53752, #70971, #63377 ),
 ( #39515, #46133, #77058, #69960 ),
 ( #445, #62877, #54753, #85688 ),
 ( #50132, #40526, #42030, #95301 ),
 ( #80570, #49640, #25786, #81076 ),
 ( #79572, #65877, #11552, #88695 ),
 ( #65380, #64885, #56761, #96797 ) ),
 .UNSPECIFIED., .F., .F., .F.,
 ( 4, 3, 4 ),
 ( 4, 4 ),
 ( 0.0004766839783820379733, 0.1029713700210895533, 0.2054660560637970590 ),
 ( 0.3195752917425375150, 0.3207354677509840490 ),
 .UNSPECIFIED. ) ;
#45319 = CARTESIAN_POINT ( 'NONE',  ( -65.52287095715006160, -24.99132157543083821, 2.256160258750667502 ) ) ;
#45320 = ORIENTED_EDGE ( 'NONE', *, *, #76788, .F. ) ;
#45321 = ORIENTED_EDGE ( 'NONE', *, *, #68951, .T. ) ;
#45322 = CARTESIAN_POINT ( 'NONE',  ( -19.80875734969026425, -5.965225279485572685, 30.51402280011862089 ) ) ;
#45323 = CARTESIAN_POINT ( 'NONE',  ( -28.62287095715004881, -23.31954350884483773, -1.443835782653508426 ) ) ;
#45324 = CARTESIAN_POINT ( 'NONE',  ( -68.51065382888901922, -23.96169478059712787, 10.65365249895718414 ) ) ;
#45325 = CARTESIAN_POINT ( 'NONE',  ( 17.37421522561336928, 11.14841987994331696, -1.500000000000002220 ) ) ;
#45326 = ADVANCED_FACE ( 'NONE', ( #90948 ), #51399, .T. ) ;
#45327 = EDGE_CURVE ( 'NONE', #497, #77260, #90451, .T. ) ;
#45328 = CARTESIAN_POINT ( 'NONE',  ( -21.57582672592670292, -1.461774377805347802, 11.49999999999999645 ) ) ;
#45329 = ORIENTED_EDGE ( 'NONE', *, *, #27367, .T. ) ;
#45330 = FACE_OUTER_BOUND ( 'NONE', #87230, .T. ) ;
#45331 = CARTESIAN_POINT ( 'NONE',  ( -96.55620429048337883, -24.64965694238574656, 8.947790433994192938 ) ) ;
#45332 = CARTESIAN_POINT ( 'NONE',  ( -14.53400517605410158, 16.95891092046126403, -1.500000000000002220 ) ) ;
#45333 = FACE_OUTER_BOUND ( 'NONE', #754, .T. ) ;
#45334 = CARTESIAN_POINT ( 'NONE',  ( -17.97250661212648026, -5.965225279485594001, -23.43622901028613015 ) ) ;
#45335 = VERTEX_POINT ( 'NONE', #51903 ) ;
#45336 = CARTESIAN_POINT ( 'NONE',  ( 0.1011420733776826480, 1.446399035885977069, -8.999999999999996447 ) ) ;
#45337 = CARTESIAN_POINT ( 'NONE',  ( 6.424528460793287543, -5.876774720514413630, 19.73230822599986212 ) ) ;
#45338 = CARTESIAN_POINT ( 'NONE',  ( 19.90007246472742608, 6.374896562862660154, 11.49999999999998934 ) ) ;
#45339 = ORIENTED_EDGE ( 'NONE', *, *, #8796, .T. ) ;
#45340 = CIRCLE ( 'NONE', #56731, 1.325999999999990298 ) ;
#45343 = ORIENTED_EDGE ( 'NONE', *, *, #11715, .F. ) ;
#45342 = ADVANCED_FACE ( 'NONE', ( #37166 ), #57127, .T. ) ;
#45341 = CARTESIAN_POINT ( 'NONE',  ( -67.58377406375005592, -24.51419770103159124, 9.386484678747168076 ) ) ;
#45344 = ORIENTED_EDGE ( 'NONE', *, *, #48432, .F. ) ;
#45345 = CARTESIAN_POINT ( 'NONE',  ( -50.62287095715005592, -23.84081130438199736, 10.88220057463248658 ) ) ;
#45346 = CARTESIAN_POINT ( 'NONE',  ( 21.03498508994548999, -2.205306954651367946, -1.500000000000002220 ) ) ;
#45347 = ORIENTED_EDGE ( 'NONE', *, *, #96856, .F. ) ;
#45348 = CARTESIAN_POINT ( 'NONE',  ( -112.5228709571500048, -23.95044443724992789, 10.65354141964648882 ) ) ;
#45349 = FACE_OUTER_BOUND ( 'NONE', #6390, .T. ) ;
#45350 = CARTESIAN_POINT ( 'NONE',  ( 21.79142754302170815, -0.6654467836950721527, -1.500000000000002220 ) ) ;
#45351 = CARTESIAN_POINT ( 'NONE',  ( -61.55620429048338593, -23.48786465467241413, 11.44779295918254824 ) ) ;
#45352 = CARTESIAN_POINT ( 'NONE',  ( -19.77875734969026311, 6.143225279485574397, 29.49402280011862487 ) ) ;
#45353 = DIRECTION ( 'NONE',  ( -3.773278334453079030E-23, 0.9999999999976377785, 2.173523156925979128E-06 ) ) ;
#45354 = CARTESIAN_POINT ( 'NONE',  ( -21.62197530259306788, 2.132803791230205359, -1.500000000000002220 ) ) ;
#45355 = CARTESIAN_POINT ( 'NONE',  ( -0.8460708837923186509, -6.376774720514410077, 19.21968329462762526 ) ) ;
#45357 = ORIENTED_EDGE ( 'NONE', *, *, #89436, .T. ) ;
#45356 = CARTESIAN_POINT ( 'NONE',  ( 16.41691039316204481, 15.16158741987741365, 11.49999999999999645 ) ) ;
#45358 = CARTESIAN_POINT ( 'NONE',  ( 26.73860345374794178, 5.356774720496559894, 19.84760796525321780 ) ) ;
#45359 = CARTESIAN_POINT ( 'NONE',  ( -85.62495572383085118, -24.92592662359561473, 8.075495903018000021 ) ) ;
#45360 = CARTESIAN_POINT ( 'NONE',  ( 27.53860345374808105, -3.356774720514427379, 1.647607965253212514 ) ) ;
#45362 = ORIENTED_EDGE ( 'NONE', *, *, #80751, .T. ) ;
#45361 = EDGE_CURVE ( 'NONE', #66086, #56438, #15312, .T. ) ;
#45363 = AXIS2_PLACEMENT_3D ( 'NONE', #91888, #39103, #47231 ) ;
#45364 = EDGE_CURVE ( 'NONE', #40713, #67776, #53603, .T. ) ;
#45365 = ORIENTED_EDGE ( 'NONE', *, *, #71662, .T. ) ;
#45366 = ADVANCED_FACE ( 'NONE', ( #38656 ), #54396, .T. ) ;
#45367 = AXIS2_PLACEMENT_3D ( 'NONE', #32195, #48942, #31705 ) ;
#45368 = VERTEX_POINT ( 'NONE', #32550 ) ;
#45369 = AXIS2_PLACEMENT_3D ( 'NONE', #83351, #81866, #26920 ) ;
#45370 = DIRECTION ( 'NONE',  ( 0.000000000000000000, 0.000000000000000000, 1.000000000000000000 ) ) ;
#45371 = CARTESIAN_POINT ( 'NONE',  ( -13.45780860896912934, -16.40347334334247265, 11.49999999999998934 ) ) ;
#45372 = CYLINDRICAL_SURFACE ( 'NONE', #33645, 0.3000000000000016542 ) ;
#45373 = CARTESIAN_POINT ( 'NONE',  ( -79.14729083585920932, -25.03138132657652193, 6.795304888836573021 ) ) ;
#45374 = CARTESIAN_POINT ( 'NONE',  ( 30.09341516180546350, -1.682774720514426114, -11.39311774897855933 ) ) ;
#45375 = CARTESIAN_POINT ( 'NONE',  ( 32.90449424769446551, 3.618459821963367240, -13.06102137676440300 ) ) ;
#45376 = CIRCLE ( 'NONE', #25946, 2.499999999999972911 ) ;
#45377 = CARTESIAN_POINT ( 'NONE',  ( -17.66094656686658482, 7.961706694365092041, -1.500000000000002220 ) ) ;
#45378 = EDGE_CURVE ( 'NONE', #64588, #32345, #63522, .T. ) ;
#45379 = CARTESIAN_POINT ( 'NONE',  ( -39.98858864963047210, -25.03707806782366418, 7.590868867492675420 ) ) ;
#45380 = ORIENTED_EDGE ( 'NONE', *, *, #63488, .F. ) ;
#45381 = CARTESIAN_POINT ( 'NONE',  ( 19.33761327413411024, 2.027444641817329973, 11.49999999999999645 ) ) ;
#45382 = CARTESIAN_POINT ( 'NONE',  ( -115.5228709571500616, -23.48786465467241769, 11.44779295918253759 ) ) ;
#45383 = ORIENTED_EDGE ( 'NONE', *, *, #28629, .F. ) ;
#45384 = DIRECTION ( 'NONE',  ( -0.9951627101165078093, -0.09824042138329590335, -1.421085471520200214E-14 ) ) ;
#45385 = CARTESIAN_POINT ( 'NONE',  ( -32.62287095715004881, -29.50250243563736774, 8.947779886222150481 ) ) ;
#45386 = CARTESIAN_POINT ( 'NONE',  ( -59.52287095715004739, -24.51387760970726148, 9.387446482453434271 ) ) ;
#45387 = DIRECTION ( 'NONE',  ( 1.000000000000000000, -0.000000000000000000, 0.000000000000000000 ) ) ;
#45388 = CARTESIAN_POINT ( 'NONE',  ( -19.13235715846047214, 4.354950445902704637, -1.500000000000002220 ) ) ;
#45389 = LINE ( 'NONE', #12915, #20196 ) ;
#45390 = VERTEX_POINT ( 'NONE', #77046 ) ;
#45391 = CARTESIAN_POINT ( 'NONE',  ( -13.10987527212420645, -17.12674121770768920, -1.500000000000002220 ) ) ;
#45392 = CARTESIAN_POINT ( 'NONE',  ( -33.52640019870900545, -24.66019654487198665, 8.947790411086133489 ) ) ;
#45393 = CARTESIAN_POINT ( 'NONE',  ( -40.52320638232922079, -24.92564183028978775, 1.928384488918254203 ) ) ;
#45394 = CARTESIAN_POINT ( 'NONE',  ( -100.4008197971955667, -25.27473221760678257, 3.294680443612905574 ) ) ;
#45395 = CARTESIAN_POINT ( 'NONE',  ( -22.84742429131147645, -2.885717679200183738, -1.500000000000002220 ) ) ;
#45396 = APPROVAL_ROLE ( '' ) ;
#45397 = DIRECTION ( 'NONE',  ( -0.000000000000000000, 2.173523156925979552E-06, -0.9999999999976378895 ) ) ;
#45398 = CARTESIAN_POINT ( 'NONE',  ( 17.47419131657910540, 6.376774720514426953, 28.31804950686278843 ) ) ;
#45399 = CARTESIAN_POINT ( 'NONE',  ( -14.30055291515510518, -14.21740073472259525, 11.49999999999999645 ) ) ;
#45400 = CARTESIAN_POINT ( 'NONE',  ( -109.0459178056501486, -25.28814249556381810, 3.663604978347184016 ) ) ;
#45401 = CARTESIAN_POINT ( 'NONE',  ( 30.93860345374796594, -6.475225279485573360, 25.41160796525322141 ) ) ;
#45402 = DIRECTION ( 'NONE',  ( 0.000000000000000000, -1.000000000000000000, 0.000000000000000000 ) ) ;
#45403 = PLANE ( 'NONE',  #6709 ) ;
#45404 = DIRECTION ( 'NONE',  ( -3.773278334453079618E-23, 0.9999999999976377785, 2.173523156925979975E-06 ) ) ;
#45405 = CARTESIAN_POINT ( 'NONE',  ( 15.68239283413728735, 12.23493734220040530, 11.49999999999998934 ) ) ;
#45406 = FACE_OUTER_BOUND ( 'NONE', #42350, .T. ) ;
#45407 = CARTESIAN_POINT ( 'NONE',  ( 19.71268880909926580, -1.816447362451163450, -1.500000000000002220 ) ) ;
#45408 = CARTESIAN_POINT ( 'NONE',  ( -126.5222601503578943, -23.48786465467241769, 11.44779295918253759 ) ) ;
#45409 = CARTESIAN_POINT ( 'NONE',  ( -123.6228709571500559, -23.47596703998600631, 11.44779298504227860 ) ) ;
#45410 = CARTESIAN_POINT ( 'NONE',  ( -66.62287095715005592, -23.47593901973091235, -1.443836447539006196 ) ) ;
#45411 = CARTESIAN_POINT ( 'NONE',  ( 4.478411676025833010, -20.21887007069289766, 11.49999999999999645 ) ) ;
#45412 = CARTESIAN_POINT ( 'NONE',  ( -58.52287095715005449, -23.72747288104470087, -1.053458166803226570 ) ) ;
#45413 = VECTOR ( 'NONE', #81517, 1000.000000000000000 ) ;
#45414 = CARTESIAN_POINT ( 'NONE',  ( -79.62287095715004170, -23.47596703998600631, 11.44779298504227860 ) ) ;
#45415 = CARTESIAN_POINT ( 'NONE',  ( 20.46598465274837864, -9.837531852206524263, 11.49999999999999645 ) ) ;
#45417 = EDGE_CURVE ( 'NONE', #77091, #44866, #6552, .T. ) ;
#45416 = ORIENTED_EDGE ( 'NONE', *, *, #1041, .F. ) ;
#45418 = LINE ( 'NONE', #36306, #59255 ) ;
#45420 = EDGE_CURVE ( 'NONE', #45969, #19596, #69405, .T. ) ;
#45419 = CARTESIAN_POINT ( 'NONE',  ( -33.58953762381673158, -24.66019654487199020, 8.947790411086131712 ) ) ;
#45421 = CIRCLE ( 'NONE', #98857, 7.652410033082763796 ) ;
#45422 = EDGE_CURVE ( 'NONE', #57540, #66877, #42638, .T. ) ;
#45423 = CARTESIAN_POINT ( 'NONE',  ( -18.21026628907936029, 8.684577975296603469, -1.500000000000002220 ) ) ;
#45424 = DIRECTION ( 'NONE',  ( 1.000000000000000000, 3.773278334444167608E-23, 8.201307833595939069E-29 ) ) ;
#45425 = EDGE_CURVE ( 'NONE', #21744, #5489, #78907, .T. ) ;
#45426 = CARTESIAN_POINT ( 'NONE',  ( -52.52287095715009002, -23.72773821059535848, 11.05748984161097503 ) ) ;
#45427 = EDGE_CURVE ( 'NONE', #63059, #9746, #63829, .T. ) ;
#45428 = ORIENTED_EDGE ( 'NONE', *, *, #5110, .T. ) ;
#45429 = B_SPLINE_CURVE_WITH_KNOTS ( 'NONE', 3,
 ( #16479, #87509, #95119, #9877, #7877, #38826, #768, #54559, #16986, #47954, #71791, #62686, #2286, #77874, #48457, #79385, #69788, #25608, #265 ),
 .UNSPECIFIED., .F., .F.,
 ( 4, 1, 1, 1, 1, 1, 1, 1, 1, 1, 1, 1, 1, 1, 1, 1, 4 ),
 ( 0.000000000000000000, 0.06815824415599749941, 0.1347066022023570842, 0.2018649976035983007, 0.2707882662774625526, 0.3400242943604910306, 0.4080827390537214439, 0.4768131952581447508, 0.5473460643070945375, 0.5856397954238962145, 0.6288649531777642521, 0.6771532033637908121, 0.7308028113651056090, 0.7898066155325017546, 0.8543250087420143357, 0.9243651340575425035, 1.000000000000000000 ),
 .UNSPECIFIED. ) ;
#45430 = EDGE_CURVE ( 'NONE', #32236, #11225, #61352, .T. ) ;
#45431 = EDGE_LOOP ( 'NONE', ( #3563, #80932, #71648, #41537 ) ) ;
#45432 = CARTESIAN_POINT ( 'NONE',  ( 0.1739078616027790736, -6.376774720514415407, 19.75705121608222115 ) ) ;
#45433 = CARTESIAN_POINT ( 'NONE',  ( 22.81499323874321661, -2.031749852351878882, -1.500000000000002220 ) ) ;
#45434 = DIRECTION ( 'NONE',  ( 0.000000000000000000, -0.9999999999976377785, -2.173523156925979975E-06 ) ) ;
#45435 = AXIS2_PLACEMENT_3D ( 'NONE', #29758, #74437, #44493 ) ;
#45436 = CARTESIAN_POINT ( 'NONE',  ( 12.90450488963236353, -17.39418326053592168, -1.500000000000002220 ) ) ;
#45437 = PLANE ( 'NONE',  #38258 ) ;
#45438 = CARTESIAN_POINT ( 'NONE',  ( -4.286263797015736595E-16, -2.056774720514426669, -3.500000000000000000 ) ) ;
#45439 = CARTESIAN_POINT ( 'NONE',  ( -18.74228827200876779, -9.293929619069025705, 11.49999999999999645 ) ) ;
#45440 = ORIENTED_EDGE ( 'NONE', *, *, #38191, .T. ) ;
#45441 = VECTOR ( 'NONE', #94709, 1000.000000000000227 ) ;
#45442 = DIRECTION ( 'NONE',  ( 0.000000000000000000, 0.000000000000000000, -1.000000000000000000 ) ) ;
#45443 = CARTESIAN_POINT ( 'NONE',  ( 2.959355296939036872, -21.81356824310248399, -1.500000000000002220 ) ) ;
#45445 = CARTESIAN_POINT ( 'NONE',  ( -105.5608698559539391, -23.48786465467241769, 11.44779295918254114 ) ) ;
#45444 = VECTOR ( 'NONE', #3082, 1000.000000000000114 ) ;
#45446 = CARTESIAN_POINT ( 'NONE',  ( -28.45645220296530908, -24.79700262693759782, 7.353600621000675908 ) ) ;
#45447 = VERTEX_POINT ( 'NONE', #22754 ) ;
#45448 = CARTESIAN_POINT ( 'NONE',  ( 4.334227700317904386, -6.376774720514402972, 18.30971318885719157 ) ) ;
#45449 = CARTESIAN_POINT ( 'NONE',  ( -90.59981717707987059, -23.85049219812686161, 10.88485053497527488 ) ) ;
#45450 = VERTEX_POINT ( 'NONE', #61852 ) ;
#45451 = CARTESIAN_POINT ( 'NONE',  ( -72.59232271956842908, -24.15620529776628089, 10.23563542870660825 ) ) ;
#45452 = ORIENTED_EDGE ( 'NONE', *, *, #22489, .T. ) ;
#45453 = ORIENTED_EDGE ( 'NONE', *, *, #46736, .F. ) ;
#45454 = CARTESIAN_POINT ( 'NONE',  ( -71.62363258555255641, -24.66019654487199730, 8.947790411086113949 ) ) ;
#45455 = LINE ( 'NONE', #37339, #38956 ) ;
#45456 = CARTESIAN_POINT ( 'NONE',  ( -57.50860782142563465, -23.96119346886880663, -0.6495511937832122440 ) ) ;
#45457 = CARTESIAN_POINT ( 'NONE',  ( 1.259202695315177589, 20.44674571593545664, -1.500000000000002220 ) ) ;
#45458 = EDGE_CURVE ( 'NONE', #59957, #80599, #39021, .T. ) ;
#45459 = EDGE_LOOP ( 'NONE', ( #81175, #47829, #40694, #51694 ) ) ;
#45460 = CARTESIAN_POINT ( 'NONE',  ( -0.9078848932494473223, -5.876774720514411854, 19.67454710845354171 ) ) ;
#45461 = CARTESIAN_POINT ( 'NONE',  ( -30.64427850938831099, -23.56000036390796382, 11.50200000000000067 ) ) ;
#45462 = DIRECTION ( 'NONE',  ( -0.6451914333552788428, 0.000000000000000000, -0.7640209514960702997 ) ) ;
#45463 = CARTESIAN_POINT ( 'NONE',  ( -4.533825836049095059, -6.376774720514411854, 19.59623724171353132 ) ) ;
#45464 = CARTESIAN_POINT ( 'NONE',  ( -51.62287095715005592, -24.64965695001468404, 8.947790433994185832 ) ) ;
#45465 = EDGE_CURVE ( 'NONE', #44470, #65117, #84667, .T. ) ;
#45466 = ORIENTED_EDGE ( 'NONE', *, *, #20827, .T. ) ;
#45467 = CARTESIAN_POINT ( 'NONE',  ( -104.5228709571500758, -23.47593901973090524, -1.443836447538996204 ) ) ;
#45468 = CARTESIAN_POINT ( 'NONE',  ( -29.47349813062140100, -25.26247812443174467, 7.035455039352441098 ) ) ;
#45469 = CARTESIAN_POINT ( 'NONE',  ( 20.50115541507891948, 3.495740877612329101, -1.500000000000002220 ) ) ;
#45470 = VERTEX_POINT ( 'NONE', #60853 ) ;
#45472 = EDGE_LOOP ( 'NONE', ( #75016, #47323, #47254, #31615, #41202, #79396 ) ) ;
#45471 = CARTESIAN_POINT ( 'NONE',  ( -54.62287095715003460, -24.33832256526968507, 0.1851278514119833740 ) ) ;
#45473 = B_SPLINE_CURVE_WITH_KNOTS ( 'NONE', 3,
 ( #81384, #58067, #48947, #79875, #72284, #2776 ),
 .UNSPECIFIED., .F., .F.,
 ( 4, 2, 4 ),
 ( 1.570755371633934808E-05, 0.001396183895866087103, 0.002776660238015835145 ),
 .UNSPECIFIED. ) ;
#45474 = LINE ( 'NONE', #23598, #48756 ) ;
#45475 = VERTEX_POINT ( 'NONE', #76539 ) ;
#45476 = ORIENTED_EDGE ( 'NONE', *, *, #94165, .F. ) ;
#45477 = CARTESIAN_POINT ( 'NONE',  ( 30.77956504631911017, -6.277769580494330093, 0.6965969997247714041 ) ) ;
#45478 = LINE ( 'NONE', #92621, #57740 ) ;
#45479 = CARTESIAN_POINT ( 'NONE',  ( -76.52287095715007581, -24.64965694238408034, 8.947790433994198267 ) ) ;
#45480 = CARTESIAN_POINT ( 'NONE',  ( -51.52287095715006870, -24.65952944569304606, 1.056160979905693686 ) ) ;
#45481 = B_SPLINE_CURVE_WITH_KNOTS ( 'NONE', 3,
 ( #51166, #74494, #27826, #97338 ),
 .UNSPECIFIED., .F., .F.,
 ( 4, 4 ),
 ( 0.000000000000000000, 9.999999999998897304E-05 ),
 .UNSPECIFIED. ) ;
#45482 = CARTESIAN_POINT ( 'NONE',  ( -92.51846257638729298, -23.73791477778912196, 11.05961554403170588 ) ) ;
#45483 = CARTESIAN_POINT ( 'NONE',  ( -73.62287095715007013, -24.66019654487199020, 8.947790411086131712 ) ) ;
#45485 = ORIENTED_EDGE ( 'NONE', *, *, #76896, .T. ) ;
#45484 = CARTESIAN_POINT ( 'NONE',  ( -7.320055889550622474, -20.87099576385019972, 11.49999999999999645 ) ) ;
#45486 = FACE_OUTER_BOUND ( 'NONE', #85024, .T. ) ;
#45487 = CARTESIAN_POINT ( 'NONE',  ( -22.13905560727926414, 4.690293145198261904, 11.49999999999998934 ) ) ;
#45488 = EDGE_CURVE ( 'NONE', #27742, #41495, #83757, .T. ) ;
#45490 = ORIENTED_EDGE ( 'NONE', *, *, #63140, .F. ) ;
#45489 = CARTESIAN_POINT ( 'NONE',  ( -87.58953762381671027, -23.47593901973091235, -1.443836447539002865 ) ) ;
#45491 = VERTEX_POINT ( 'NONE', #90790 ) ;
#45492 = CARTESIAN_POINT ( 'NONE',  ( -122.6228709571500417, -23.48786465467242124, 11.44779295918253759 ) ) ;
#45493 = EDGE_CURVE ( 'NONE', #68827, #17038, #13149, .T. ) ;
#45494 = B_SPLINE_CURVE_WITH_KNOTS ( 'NONE', 3,
 ( #76154, #44729, #22357, #84273, #45231, #83278, #38101, #76647 ),
 .UNSPECIFIED., .F., .F.,
 ( 4, 2, 2, 4 ),
 ( -0.001240355328176878311, -0.0002398155169399597986, 0.0007607242942969587134, 0.002761803916770787931 ),
 .UNSPECIFIED. ) ;
#45495 = CARTESIAN_POINT ( 'NONE',  ( 6.436487395234643749, 19.08016507665710648, 11.49999999999998934 ) ) ;
#45496 = CARTESIAN_POINT ( 'NONE',  ( -25.92875734969026524, 5.356774720514425603, 0.7300228001186309656 ) ) ;
#45497 = ORIENTED_EDGE ( 'NONE', *, *, #16879, .F. ) ;
#45498 = CARTESIAN_POINT ( 'NONE',  ( -126.5228709571501184, -24.34917612406837861, 0.1852690917426611239 ) ) ;
#45499 = CARTESIAN_POINT ( 'NONE',  ( -11.77839732991513166, 18.97803183815481987, -1.500000000000002220 ) ) ;
#45500 = ORIENTED_EDGE ( 'NONE', *, *, #21910, .T. ) ;
#45501 = EDGE_LOOP ( 'NONE', ( #11200, #25567, #71331, #48089 ) ) ;
#45502 = DIRECTION ( 'NONE',  ( 3.773278334444167608E-23, -1.000000000000000000, 0.000000000000000000 ) ) ;
#45503 = CARTESIAN_POINT ( 'NONE',  ( -124.5228709571500616, -29.50250243563736774, 8.947779886222134493 ) ) ;
#45504 = DIRECTION ( 'NONE',  ( 3.278764309610055092E-18, 4.688851412615178005E-17, -1.000000000000000000 ) ) ;
#45505 = DIRECTION ( 'NONE',  ( -0.000000000000000000, 1.000000000000000000, -0.000000000000000000 ) ) ;
#45506 = DIRECTION ( 'NONE',  ( -1.000000000000000000, -3.773278334444166432E-23, -8.201307841325785021E-29 ) ) ;
#45507 = AXIS2_PLACEMENT_3D ( 'NONE', #92406, #46244, #69589 ) ;
#45508 = CARTESIAN_POINT ( 'NONE',  ( 3.395600993332231532, 19.23619202488179525, 11.49999999999998934 ) ) ;
#45509 = DIRECTION ( 'NONE',  ( 0.000000000000000000, 0.000000000000000000, -1.000000000000000000 ) ) ;
#45510 = VECTOR ( 'NONE', #96600, 1000.000000000000000 ) ;
#45511 = CARTESIAN_POINT ( 'NONE',  ( -5.860608850286626925, 20.67097946995454905, -1.500000000000002220 ) ) ;
#45512 = CARTESIAN_POINT ( 'NONE',  ( -2.732037236150805626, -6.376774720514411854, 19.78976258633487717 ) ) ;
#45513 = PLANE ( 'NONE',  #53555 ) ;
#45514 = DIRECTION ( 'NONE',  ( 0.000000000000000000, 1.000000000000000000, 0.000000000000000000 ) ) ;
#45515 = CARTESIAN_POINT ( 'NONE',  ( -9.520747347383798243, -20.79447232172871907, -1.500000000000002220 ) ) ;
#45516 = PERSON_AND_ORGANIZATION ( #70597, #27821 ) ;
#45517 = CARTESIAN_POINT ( 'NONE',  ( -96.55228293290541330, -24.15620529776628445, 10.23563542870660115 ) ) ;
#45518 = DIRECTION ( 'NONE',  ( 0.000000000000000000, 0.000000000000000000, 1.000000000000000000 ) ) ;
#45519 = CARTESIAN_POINT ( 'NONE',  ( 12.72590371223024697, 15.41468647733915809, 11.49999999999999645 ) ) ;
#45520 = PLANE ( 'NONE',  #97096 ) ;
#45521 = CARTESIAN_POINT ( 'NONE',  ( -74.51177717695108527, -23.96169478059713498, 10.65365249895717881 ) ) ;
#45522 = CARTESIAN_POINT ( 'NONE',  ( 3.737436867076077363, 13.63388347648318444, 2.100000000000000089 ) ) ;
#45523 = ORIENTED_EDGE ( 'NONE', *, *, #13967, .F. ) ;
#45524 = DIRECTION ( 'NONE',  ( -1.000000000000000000, -3.773278334444166432E-23, -8.201307841325785021E-29 ) ) ;
#45525 = CARTESIAN_POINT ( 'NONE',  ( 10.48383480065558615, -3.481296116130239149, -27.02502823977714286 ) ) ;
#45526 = CARTESIAN_POINT ( 'NONE',  ( -1.994712787082457472, 21.64621699974126656, -1.500000000000002220 ) ) ;
#45527 = FACE_OUTER_BOUND ( 'NONE', #70523, .T. ) ;
#45528 = CARTESIAN_POINT ( 'NONE',  ( -6.824658503225996320, 18.35159230250476270, -1.500000000000002220 ) ) ;
#45529 = CARTESIAN_POINT ( 'NONE',  ( -74.52287095715007581, -29.50248528299804818, 1.056150453629036701 ) ) ;
#45530 = B_SPLINE_CURVE_WITH_KNOTS ( 'NONE', 3,
 ( #10339, #41807, #49422, #18450, #50908, #26573, #57534, #26061, #42805, #3249, #33681, #43299, #4230, #88972 ),
 .UNSPECIFIED., .F., .F.,
 ( 4, 2, 2, 2, 2, 2, 4 ),
 ( 7.059813062317230268E-18, 0.0001563035440846473692, 0.0003126070881692876910, 0.0006252141763385689853, 0.0009378212645078503338, 0.001094124808592491713, 0.001250428352677132766 ),
 .UNSPECIFIED. ) ;
#45531 = APPROVAL_STATUS ( 'not_yet_approved' ) ;
#45532 = LINE ( 'NONE', #20676, #56454 ) ;
#45533 = FACE_OUTER_BOUND ( 'NONE', #12283, .T. ) ;
#45534 = CARTESIAN_POINT ( 'NONE',  ( -16.44861368136865920, 12.28130381464353782, 11.49999999999999645 ) ) ;
#45535 = CARTESIAN_POINT ( 'NONE',  ( -121.5228709571500616, -29.50248528299804818, 1.056150453629045360 ) ) ;
#45536 = PLANE ( 'NONE',  #46472 ) ;
#45537 = ADVANCED_FACE ( 'NONE', ( #68453 ), #44617, .T. ) ;
#45538 = ORIENTED_EDGE ( 'NONE', *, *, #61772, .F. ) ;
#45539 = CARTESIAN_POINT ( 'NONE',  ( -72.52287095715009002, -24.51283580621365488, 0.6167428607019659337 ) ) ;
#45540 = PLANE ( 'NONE',  #5603 ) ;
#45542 = EDGE_CURVE ( 'NONE', #6180, #43572, #28061, .T. ) ;
#45541 = CARTESIAN_POINT ( 'NONE',  ( -90.62287095715004170, -23.48786465467241058, 11.44779295918254469 ) ) ;
#45543 = CARTESIAN_POINT ( 'NONE',  ( -69.62287095715005592, -24.64965695001468404, 8.947790433994184056 ) ) ;
#45544 = CARTESIAN_POINT ( 'NONE',  ( -85.52287095715004739, -24.52232992886361629, 0.6492154411906000400 ) ) ;
#45545 = EDGE_CURVE ( 'NONE', #59154, #5489, #5052, .T. ) ;
#45546 = DIRECTION ( 'NONE',  ( 0.000000000000000000, 0.9999999999976377785, 2.173523156925979975E-06 ) ) ;
#45547 = EDGE_CURVE ( 'NONE', #20858, #42990, #49257, .T. ) ;
#45548 = CARTESIAN_POINT ( 'NONE',  ( 6.910522817300494225, 22.03692736239173300, 11.49999999999999645 ) ) ;
#45549 = CARTESIAN_POINT ( 'NONE',  ( -6.082769120682566921, -21.99330073093985405, -1.500000000000002220 ) ) ;
#45550 = CARTESIAN_POINT ( 'NONE',  ( -110.6352833674019820, -23.48786465467241769, 11.44779295918253759 ) ) ;
#45551 = EDGE_CURVE ( 'NONE', #86024, #53534, #98309, .T. ) ;
#45552 = CARTESIAN_POINT ( 'NONE',  ( -5.706951327759631099, -6.376774720514411854, 19.48569229636961353 ) ) ;
#45553 = CARTESIAN_POINT ( 'NONE',  ( -85.58953762381669605, -24.99156044556120193, 7.747789690856343725 ) ) ;
#45554 = PLANE ( 'NONE',  #49608 ) ;
#45555 = EDGE_CURVE ( 'NONE', #60162, #55041, #46624, .T. ) ;
#45556 = CARTESIAN_POINT ( 'NONE',  ( -99.64934318012689118, -25.31582198417827811, 4.927356293751860683 ) ) ;
#45557 = AXIS2_PLACEMENT_3D ( 'NONE', #20901, #21391, #12291 ) ;
#45558 = CARTESIAN_POINT ( 'NONE',  ( 20.64021973274467570, 7.317367941133321452, -1.500000000000002220 ) ) ;
#45559 = CARTESIAN_POINT ( 'NONE',  ( -58.62287095715004881, -23.48783264082478439, -1.443836473390069264 ) ) ;
#45560 = DIRECTION ( 'NONE',  ( 0.000000000000000000, 0.000000000000000000, -1.000000000000000000 ) ) ;
#45561 = CARTESIAN_POINT ( 'NONE',  ( -77.62287095715011276, -24.51283580621365132, 0.6167428607019761477 ) ) ;
#45562 = CARTESIAN_POINT ( 'NONE',  ( -105.5228709571500758, -29.50250786944525672, 11.44777988621622988 ) ) ;
#45563 = CARTESIAN_POINT ( 'NONE',  ( 22.02124265030973760, 6.143225279485574397, 16.20402280011862217 ) ) ;
#45564 = CARTESIAN_POINT ( 'NONE',  ( -122.6228709571500985, -24.35013146730204525, 9.818937971375095941 ) ) ;
#45565 = ORIENTED_EDGE ( 'NONE', *, *, #34880, .F. ) ;
#45566 = B_SPLINE_CURVE_WITH_KNOTS ( 'NONE', 3,
 ( #43621, #50738, #90289, #68452, #35996, #51732, #28887, #97885, #98889, #97401, #27887, #29382, #44119, #74561 ),
 .UNSPECIFIED., .F., .F.,
 ( 4, 2, 2, 2, 2, 2, 4 ),
 ( 3.469446951953614189E-18, 0.0002365416005296795297, 0.0004730832010593555900, 0.0007096248015890316502, 0.0009461664021187077105, 0.001419249603178059831, 0.001892332804237411951 ),
 .UNSPECIFIED. ) ;
#45567 = CARTESIAN_POINT ( 'NONE',  ( 16.92567061652012228, 11.46397006495115534, -1.500000000000002220 ) ) ;
#45568 = VERTEX_POINT ( 'NONE', #41007 ) ;
#45569 = ORIENTED_EDGE ( 'NONE', *, *, #25017, .F. ) ;
#45570 = EDGE_LOOP ( 'NONE', ( #27763, #21139, #68150, #94535 ) ) ;
#45571 = EDGE_LOOP ( 'NONE', ( #89125, #37335, #11152, #98838 ) ) ;
#45572 = CARTESIAN_POINT ( 'NONE',  ( -21.01138170180016118, -9.542296329091309204, -1.500000000000002220 ) ) ;
#45573 = CARTESIAN_POINT ( 'NONE',  ( -35.52287095715005449, -23.48783264083451883, -1.443836473374936258 ) ) ;
#45574 = CARTESIAN_POINT ( 'NONE',  ( 12.15850541088210868, 16.18036119754114566, -1.500000000000002220 ) ) ;
#45575 = EDGE_LOOP ( 'NONE', ( #93518, #72798, #31987, #77263 ) ) ;
#45576 = CARTESIAN_POINT ( 'NONE',  ( -29.26507481595814752, -25.20890896920636592, 5.848370260082334404 ) ) ;
#45577 = CARTESIAN_POINT ( 'NONE',  ( -127.6228709571500559, -24.64965695001469115, 8.947790433994173398 ) ) ;
#45579 = CARTESIAN_POINT ( 'NONE',  ( -47.55620429048338593, -23.48783264082478084, -1.443836473390070596 ) ) ;
#45578 = VECTOR ( 'NONE', #26161, 1000.000000000000000 ) ;
#45580 = CARTESIAN_POINT ( 'NONE',  ( -99.51410621055458705, -24.15620529776628800, 10.23563542870660115 ) ) ;
#45582 = ORIENTED_EDGE ( 'NONE', *, *, #16502, .T. ) ;
#45581 = CARTESIAN_POINT ( 'NONE',  ( 15.63241172484657682, -14.69700884395465934, 11.49999999999999645 ) ) ;
#45583 = CARTESIAN_POINT ( 'NONE',  ( -113.6228709571500417, -23.72747288104442021, -1.053458166803661777 ) ) ;
#45584 = CARTESIAN_POINT ( 'NONE',  ( 14.43441819135929194, 3.316774720514426456, -28.36222020317710957 ) ) ;
#45585 =( GEOMETRIC_REPRESENTATION_CONTEXT ( 3 ) GLOBAL_UNCERTAINTY_ASSIGNED_CONTEXT ( ( #23533 ) ) GLOBAL_UNIT_ASSIGNED_CONTEXT ( ( #61271, #86084, #53655 ) ) REPRESENTATION_CONTEXT ( 'NONE', 'WORKASPACE' ) );
#45586 = ORIENTED_EDGE ( 'NONE', *, *, #7856, .T. ) ;
#45587 = CARTESIAN_POINT ( 'NONE',  ( 8.970943996638910178, -18.66293075132952950, 11.49999999999998934 ) ) ;
#45589 = ORIENTED_EDGE ( 'NONE', *, *, #98010, .T. ) ;
#45588 = DIRECTION ( 'NONE',  ( 0.000000000000000000, -1.000000000000000000, 0.000000000000000000 ) ) ;
#45590 = CARTESIAN_POINT ( 'NONE',  ( -28.62167455042580499, -23.33138160483529688, -1.443835813551990865 ) ) ;
#45591 = ORIENTED_EDGE ( 'NONE', *, *, #73549, .F. ) ;
#45592 = CARTESIAN_POINT ( 'NONE',  ( 4.642799911345256270, -6.376774720514408301, 18.59646607068888713 ) ) ;
#45593 = CARTESIAN_POINT ( 'NONE',  ( -65.59221808990133695, -24.40034930558990922, 0.3402023900116040167 ) ) ;
#45594 = CARTESIAN_POINT ( 'NONE',  ( -9.458160343781703006, 19.84743614482962926, 11.49999999999999645 ) ) ;
#45595 = CARTESIAN_POINT ( 'NONE',  ( -105.6228709571500417, -29.50249982740957577, 7.747779886224967605 ) ) ;
#45596 = CARTESIAN_POINT ( 'NONE',  ( 6.619388286264371146, -21.57091762011834390, 11.49999999999998934 ) ) ;
#45597 = CARTESIAN_POINT ( 'NONE',  ( -13.85205798638896901, 15.75786377350088507, -1.500000000000002220 ) ) ;
#45598 = CARTESIAN_POINT ( 'NONE',  ( -70.35895856474229504, -25.30161620421289470, 5.313173632321669615 ) ) ;
#45599 = CARTESIAN_POINT ( 'NONE',  ( 5.811591729264017125, -6.376774720514422512, 21.22699980322195046 ) ) ;
#45600 = ORIENTED_EDGE ( 'NONE', *, *, #66405, .F. ) ;
#45601 = ORIENTED_EDGE ( 'NONE', *, *, #5664, .F. ) ;
#45602 = EDGE_LOOP ( 'NONE', ( #16229, #52214, #77997, #46834, #7374, #7107, #17342, #6790, #14130, #86613, #36964, #38840, #80675, #51045, #22212, #27994 ) ) ;
#45603 = CARTESIAN_POINT ( 'NONE',  ( -88.52287095715010423, -23.72773821059536914, 11.05748984161097503 ) ) ;
#45604 = EDGE_CURVE ( 'NONE', #20296, #74207, #96175, .T. ) ;
#45605 = CARTESIAN_POINT ( 'NONE',  ( -15.55086147716002110, 14.89234021980106881, -1.500000000000002220 ) ) ;
#45606 = EDGE_CURVE ( 'NONE', #40077, #54069, #23298, .T. ) ;
#45607 = DIRECTION ( 'NONE',  ( 0.000000000000000000, 0.9999999999976377785, 2.173523156925979128E-06 ) ) ;
#45608 = VERTEX_POINT ( 'NONE', #94278 ) ;
#45609 = CARTESIAN_POINT ( 'NONE',  ( -19.39432879369159224, 8.380699159679657839, -1.500000000000002220 ) ) ;
#45610 = CARTESIAN_POINT ( 'NONE',  ( 5.184553252003285984, -5.965225279485572685, -28.06387035751381731 ) ) ;
#45611 = CARTESIAN_POINT ( 'NONE',  ( -64.55954162791702799, -23.73766607897670156, -1.055555164236459564 ) ) ;
#45612 = CARTESIAN_POINT ( 'NONE',  ( -100.5228709571500616, -25.00158670708909625, 2.256160236439166411 ) ) ;
#45613 = CARTESIAN_POINT ( 'NONE',  ( -46.52287095715006160, -29.50250786944525672, 11.44777988621624054 ) ) ;
#45614 = CARTESIAN_POINT ( 'NONE',  ( -123.6228709571500559, -23.48783264082478794, -1.443836473390058606 ) ) ;
#45615 = CARTESIAN_POINT ( 'NONE',  ( 4.260453091581613450, -21.75001586557718980, -1.500000000000002220 ) ) ;
#45616 = CARTESIAN_POINT ( 'NONE',  ( -71.62363249165781554, -24.65952944569304961, 1.056160979905700570 ) ) ;
#45617 = VERTEX_POINT ( 'NONE', #63363 ) ;
#45618 = CARTESIAN_POINT ( 'NONE',  ( -51.52812418322009336, -25.31633154934941743, 5.264378407383865088 ) ) ;
#45619 = CARTESIAN_POINT ( 'NONE',  ( 13.59451591917074431, 3.316774720514426456, -28.23515841827053308 ) ) ;
#45620 = CARTESIAN_POINT ( 'NONE',  ( 25.61870917940689196, -5.965225279485572685, 29.49402280011862487 ) ) ;
#45621 = B_SPLINE_CURVE_WITH_KNOTS ( 'NONE', 3,
 ( #25342, #87239, #55813, #24839 ),
 .UNSPECIFIED., .F., .F.,
 ( 4, 4 ),
 ( 0.000000000000000000, 0.0001002978970083000140 ),
 .UNSPECIFIED. ) ;
#45622 = CARTESIAN_POINT ( 'NONE',  ( -97.52287095715006160, -23.47596703998600631, 11.44779298504228215 ) ) ;
#45623 = CARTESIAN_POINT ( 'NONE',  ( 17.65527434030279252, -8.155491144718855168, 11.49999999999998934 ) ) ;
#45624 = CARTESIAN_POINT ( 'NONE',  ( -1.242826169824672977, 21.35102975155811222, 11.49999999999998934 ) ) ;
#45625 = CARTESIAN_POINT ( 'NONE',  ( -64.58953762381673869, -24.65952944569304250, 1.056160979905695907 ) ) ;
#45626 = CARTESIAN_POINT ( 'NONE',  ( 3.509873074917118085, 0.3587747205144265483, 29.15869884040363758 ) ) ;
#45627 = AXIS2_PLACEMENT_3D ( 'NONE', #8322, #86446, #40276 ) ;
#45628 = CARTESIAN_POINT ( 'NONE',  ( 33.00535138976610483, 5.965225279485572685, -12.97242311383961066 ) ) ;
#45629 = CARTESIAN_POINT ( 'NONE',  ( -129.5228709571500758, -23.47593901973090524, -1.443836447538996204 ) ) ;
#45630 = EDGE_CURVE ( 'NONE', #58910, #82905, #77544, .T. ) ;
#45631 = CARTESIAN_POINT ( 'NONE',  ( -16.08347380570801377, -15.98036338121420030, -1.500000000000002220 ) ) ;
#45632 = ORIENTED_EDGE ( 'NONE', *, *, #29676, .T. ) ;
#45633 = LINE ( 'NONE', #98901, #83875 ) ;
#45634 = CARTESIAN_POINT ( 'NONE',  ( -102.5562042904834072, -24.64965694238575011, 8.947790433994196491 ) ) ;
#45635 = CARTESIAN_POINT ( 'NONE',  ( -8.418173371947181849, -17.93405594323863284, 11.49999999999999645 ) ) ;
#45636 = CARTESIAN_POINT ( 'NONE',  ( 3.509873074917118085, -0.3587747205144265483, 29.15869884040363758 ) ) ;
#45637 = EDGE_LOOP ( 'NONE', ( #18847, #36828, #6418, #5895 ) ) ;
#45638 = DIRECTION ( 'NONE',  ( 0.000000000000000000, 0.000000000000000000, 1.000000000000000000 ) ) ;
#45639 = CARTESIAN_POINT ( 'NONE',  ( 12.66784028006542151, 2.682774720514427003, -27.12025593822526304 ) ) ;
#45640 = CARTESIAN_POINT ( 'NONE',  ( 20.55956107658784404, -6.795330137259728787, -1.500000000000002220 ) ) ;
#45641 = LINE ( 'NONE', #35541, #39921 ) ;
#45642 = CARTESIAN_POINT ( 'NONE',  ( 13.61561175257155298, 13.87280521877887018, -1.500000000000002220 ) ) ;
#45643 = LINE ( 'NONE', #14174, #41683 ) ;
#45644 = CARTESIAN_POINT ( 'NONE',  ( -129.5228709571500758, -24.50321055353805377, 9.387540953477515160 ) ) ;
#45645 = CARTESIAN_POINT ( 'NONE',  ( 16.01007288495529224, -11.65062672332236104, -1.500000000000002220 ) ) ;
#45646 = AXIS2_PLACEMENT_3D ( 'NONE', #4205, #94543, #57008 ) ;
#45647 = VERTEX_POINT ( 'NONE', #64367 ) ;
#45648 = CC_DESIGN_SECURITY_CLASSIFICATION ( #60221, ( #57026 ) ) ;
#45649 = CARTESIAN_POINT ( 'NONE',  ( 2.303441031721801480, -20.17751241584783628, 11.49999999999999645 ) ) ;
#45650 = CARTESIAN_POINT ( 'NONE',  ( -40.62287095715004170, -29.50249982740957577, 7.747779886224967605 ) ) ;
#45651 = PLANE ( 'NONE',  #14959 ) ;
#45652 = B_SPLINE_CURVE_WITH_KNOTS ( 'NONE', 3,
 ( #78092, #62911, #70503, #55795, #61900, #992 ),
 .UNSPECIFIED., .F., .F.,
 ( 4, 2, 4 ),
 ( 1.570887131794333942E-05, 0.001396322306279758904, 0.002776935741241574537 ),
 .UNSPECIFIED. ) ;
#45653 = VERTEX_POINT ( 'NONE', #31386 ) ;
#45654 = DIRECTION ( 'NONE',  ( -3.773278334444166432E-23, 1.000000000000000000, 0.000000000000000000 ) ) ;
#45655 = DIRECTION ( 'NONE',  ( 0.000000000000000000, 0.000000000000000000, 1.000000000000000000 ) ) ;
#45656 = CARTESIAN_POINT ( 'NONE',  ( -48.95379770480546711, -25.31601981760315923, 5.698183519111846174 ) ) ;
#45657 = DIRECTION ( 'NONE',  ( -3.773278334453079618E-23, 0.9999999999976377785, 2.173523156925979975E-06 ) ) ;
#45658 = CARTESIAN_POINT ( 'NONE',  ( -0.7827064370038755436, -6.376774720514410077, 19.55912026249540148 ) ) ;
#45659 = CARTESIAN_POINT ( 'NONE',  ( -18.95788008782500356, -6.583919088883305015, -1.500000000000002220 ) ) ;
#45660 = DIRECTION ( 'NONE',  ( -0.000000000000000000, 1.000000000000000000, -0.000000000000000000 ) ) ;
#45662 = EDGE_LOOP ( 'NONE', ( #27218, #89373, #89261, #27101, #10490, #34562, #23815, #45002 ) ) ;
#45661 = EDGE_CURVE ( 'NONE', #52812, #66746, #16652, .T. ) ;
#45663 = DIRECTION ( 'NONE',  ( 0.000000000000000000, 0.000000000000000000, 1.000000000000000000 ) ) ;
#45664 = EDGE_CURVE ( 'NONE', #38848, #79772, #79558, .T. ) ;
#45665 = CARTESIAN_POINT ( 'NONE',  ( -4.681240387505234857, -22.43558246840685300, 11.49999999999999645 ) ) ;
#45666 = CARTESIAN_POINT ( 'NONE',  ( 20.46598465274837864, -9.837531852206524263, -1.500000000000002220 ) ) ;
#45667 = DIRECTION ( 'NONE',  ( -0.000000000000000000, -1.000000000000000000, -0.000000000000000000 ) ) ;
#45668 = EDGE_CURVE ( 'NONE', #55838, #53330, #42734, .T. ) ;
#45669 = CARTESIAN_POINT ( 'NONE',  ( -28.52287095715006870, -24.35176667652165250, 0.6166262579151312595 ) ) ;
#45670 = CARTESIAN_POINT ( 'NONE',  ( -38.63477338751106771, -24.35071581493542325, 9.817618358456030592 ) ) ;
#45671 = ADVANCED_FACE ( 'NONE', ( #54240 ), #54085, .T. ) ;
#45672 = DIRECTION ( 'NONE',  ( 0.000000000000000000, 0.000000000000000000, -1.000000000000000000 ) ) ;
#45673 = CARTESIAN_POINT ( 'NONE',  ( -117.6228709571500559, -23.47596703998600631, 11.44779298504227683 ) ) ;
#45674 = AXIS2_PLACEMENT_3D ( 'NONE', #12395, #98123, #58586 ) ;
#45675 = DIRECTION ( 'NONE',  ( -0.000000000000000000, 1.000000000000000000, -0.000000000000000000 ) ) ;
#45676 = VERTEX_POINT ( 'NONE', #80558 ) ;
#45677 = CARTESIAN_POINT ( 'NONE',  ( -19.36681041099238598, 6.328833669845586485, -1.500000000000002220 ) ) ;
#45678 = EDGE_LOOP ( 'NONE', ( #68093, #26482, #90087, #6715 ) ) ;
#45679 = ADVANCED_FACE ( 'NONE', ( #72960 ), #88680, .F. ) ;
#45680 = CARTESIAN_POINT ( 'NONE',  ( 21.75294195941402364, -7.338126679257295670, -1.500000000000002220 ) ) ;
#45681 = CARTESIAN_POINT ( 'NONE',  ( -62.52287095715006160, -29.50250786944525672, 11.44777988621623876 ) ) ;
#45682 = ORIENTED_EDGE ( 'NONE', *, *, #13909, .F. ) ;
#45683 = PLANE ( 'NONE',  #3970 ) ;
#45684 = CARTESIAN_POINT ( 'NONE',  ( -116.5228709571500900, -24.51387760970725793, 9.387446482453407626 ) ) ;
#45685 = CARTESIAN_POINT ( 'NONE',  ( -51.54737341646723792, -24.15620529776627734, 10.23563542870660470 ) ) ;
#45687 = ORIENTED_EDGE ( 'NONE', *, *, #68898, .T. ) ;
#45686 = CARTESIAN_POINT ( 'NONE',  ( 14.73992482348874411, 15.29747818672187165, 11.49999999999999645 ) ) ;
#45688 = VERTEX_POINT ( 'NONE', #27771 ) ;
#45689 = CARTESIAN_POINT ( 'NONE',  ( 5.796264663052079769, -21.44337444023769379, 11.49999999999998934 ) ) ;
#45690 = CIRCLE ( 'NONE', #13292, 18.35000000000000142 ) ;
#45691 = CARTESIAN_POINT ( 'NONE',  ( -20.60669311552257810, 0.8253496925510150906, 11.49999999999998934 ) ) ;
#45692 = B_SPLINE_CURVE_WITH_KNOTS ( 'NONE', 3,
 ( #60190, #98219, #44960, #6386, #35840, #5387, #12498, #4894 ),
 .UNSPECIFIED., .F., .F.,
 ( 4, 2, 2, 4 ),
 ( 0.000000000000000000, 0.002001079623178224094, 0.003001619434767337658, 0.004002159246356451656 ),
 .UNSPECIFIED. ) ;
#45693 = ORIENTED_EDGE ( 'NONE', *, *, #74387, .F. ) ;
#45694 = ORIENTED_EDGE ( 'NONE', *, *, #77944, .F. ) ;
#45695 = CARTESIAN_POINT ( 'NONE',  ( 3.797776442307698286, -6.376774720514427841, 21.83974358974358410 ) ) ;
#45696 = CARTESIAN_POINT ( 'NONE',  ( -40.25280366610014227, -25.12199515523669291, 2.840616586787004128 ) ) ;
#45697 = ORIENTED_EDGE ( 'NONE', *, *, #55908, .F. ) ;
#45698 = CARTESIAN_POINT ( 'NONE',  ( -51.62287095715005592, -24.66019654487199020, 8.947790411086135265 ) ) ;
#45699 = ORIENTED_EDGE ( 'NONE', *, *, #22751, .F. ) ;
#45700 = CARTESIAN_POINT ( 'NONE',  ( -39.52287095715006870, -24.64965694238406613, 8.947790433994205372 ) ) ;
#45701 = CARTESIAN_POINT ( 'NONE',  ( -45.62287095715004881, -24.99132157543083821, 2.256160258750667502 ) ) ;
#45702 = CARTESIAN_POINT ( 'NONE',  ( 20.70993026999094511, 1.908435391604796028, -1.500000000000002220 ) ) ;
#45703 = CARTESIAN_POINT ( 'NONE',  ( 19.81658424304261246, 9.080307684375437560, 11.49999999999999645 ) ) ;
#45704 = CARTESIAN_POINT ( 'NONE',  ( -39.97032894598978459, -25.19873439044615893, 3.393671681319915034 ) ) ;
#45705 = CARTESIAN_POINT ( 'NONE',  ( -99.28744282076259253, -25.12404174411991775, 7.096701639951624507 ) ) ;
#45706 = CARTESIAN_POINT ( 'NONE',  ( -16.74552829020559130, -14.98668287627115170, -1.500000000000002220 ) ) ;
#45707 = CARTESIAN_POINT ( 'NONE',  ( -50.56373716527822637, -25.26334748840130828, 4.723080157104919685 ) ) ;
#45709 = VERTEX_POINT ( 'NONE', #89176 ) ;
#45708 = ADVANCED_FACE ( 'NONE', ( #66852 ), #73951, .F. ) ;
#45710 = B_SPLINE_CURVE_WITH_KNOTS ( 'NONE', 3,
 ( #99266, #76419, #37878, #44499 ),
 .UNSPECIFIED., .F., .F.,
 ( 4, 4 ),
 ( 0.000000000000000000, 9.999999999998897304E-05 ),
 .UNSPECIFIED. ) ;
#45711 = CARTESIAN_POINT ( 'NONE',  ( -80.88924702628075636, -25.30869131066464561, 4.592921213095906730 ) ) ;
#45712 = VECTOR ( 'NONE', #78160, 1000.000000000000000 ) ;
#45713 = CARTESIAN_POINT ( 'NONE',  ( -101.9507253916653440, -25.24282061761981666, 6.236250683194342059 ) ) ;
#45714 = LOCAL_TIME ( 0, 54, 15.00000000000000000, #14917 ) ;
#45715 = ORIENTED_EDGE ( 'NONE', *, *, #88499, .F. ) ;
#45716 = ORIENTED_EDGE ( 'NONE', *, *, #85648, .F. ) ;
#45717 = EDGE_CURVE ( 'NONE', #91001, #83268, #25773, .T. ) ;
#45718 = ORIENTED_EDGE ( 'NONE', *, *, #52873, .F. ) ;
#45719 = CARTESIAN_POINT ( 'NONE',  ( -1.966620079519992181, -21.27258529651320274, -1.500000000000002220 ) ) ;
#45720 = EDGE_LOOP ( 'NONE', ( #92771, #50474, #24759, #95702 ) ) ;
#45721 = CARTESIAN_POINT ( 'NONE',  ( 2.700122536338566359, 20.86363338933649558, -1.500000000000002220 ) ) ;
#45722 = CARTESIAN_POINT ( 'NONE',  ( -30.47816396153159602, -24.83083109926283072, 1.633466014234818076 ) ) ;
#45723 = CARTESIAN_POINT ( 'NONE',  ( 14.62591090210861999, -3.611920024593927803, -27.34381298535168270 ) ) ;
#45724 = CARTESIAN_POINT ( 'NONE',  ( 2.903846153846159517, -6.376774720514415407, 19.99999999999999289 ) ) ;
#45725 = CARTESIAN_POINT ( 'NONE',  ( -21.86317675896206225, -2.224439152981679602, -1.500000000000002220 ) ) ;
#45726 = CARTESIAN_POINT ( 'NONE',  ( -87.63524930070781238, -23.96119346886882084, -0.6495511937831871530 ) ) ;
#45727 = EDGE_LOOP ( 'NONE', ( #6735, #31126, #50960, #3877 ) ) ;
#45728 = CARTESIAN_POINT ( 'NONE',  ( 8.071512145086531476, -9.528487854913507249, 1.500000000000003997 ) ) ;
#45729 = B_SPLINE_CURVE_WITH_KNOTS ( 'NONE', 3,
 ( #92928, #54388, #77695, #92431 ),
 .UNSPECIFIED., .F., .F.,
 ( 4, 4 ),
 ( 0.9663008150836682741, 0.9998940316929132432 ),
 .UNSPECIFIED. ) ;
#45730 = CARTESIAN_POINT ( 'NONE',  ( 27.53860345374808105, 3.356774720514427379, 1.647607965253216067 ) ) ;
#45731 = CARTESIAN_POINT ( 'NONE',  ( -128.5228709571499621, -23.73907113217699560, -1.053371485780730143 ) ) ;
#45732 = CARTESIAN_POINT ( 'NONE',  ( -30.58080474561622353, -25.30588374461880008, 5.002395802403317049 ) ) ;
#45733 = CARTESIAN_POINT ( 'NONE',  ( -3.120219904758775975, 21.05623772282662998, 11.49999999999998934 ) ) ;
#45734 = PLANE ( 'NONE',  #64531 ) ;
#45735 = CARTESIAN_POINT ( 'NONE',  ( -107.5222081683197786, -23.48786465467241769, 11.44779295918253936 ) ) ;
#45736 = CARTESIAN_POINT ( 'NONE',  ( 15.30669617938070459, -3.316774720514427344, -28.51986056384665957 ) ) ;
#45737 = DIRECTION ( 'NONE',  ( -3.773278334453079030E-23, 0.9999999999976377785, 2.173523156925979128E-06 ) ) ;
#45738 = APPROVAL ( #37891, 'UNSPECIFIED' ) ;
#45739 = CARTESIAN_POINT ( 'NONE',  ( 12.90280524143238594, -18.44629484376132922, -1.500000000000002220 ) ) ;
#45740 = B_SPLINE_SURFACE_WITH_KNOTS ( 'NONE', 3, 3, ( 
 ( #11139, #71551, #42109, #26866 ),
 ( #88776, #50210, #11630, #2044 ),
 ( #32986, #64462, #42608, #65955 ),
 ( #48724, #95376, #73544, #4037 ),
 ( #25864, #14122, #6018, #60331 ),
 ( #51705, #6525, #75518, #27861 ),
 ( #12633, #44591, #22227, #36973 ) ),
 .UNSPECIFIED., .F., .F., .F.,
 ( 4, 3, 4 ),
 ( 4, 4 ),
 ( 0.7945040050992242531, 0.8970133687736503436, 0.9995227324480764342 ),
 ( 0.5696387503446669331, 0.5709144579475504688 ),
 .UNSPECIFIED. ) ;
#45741 = PLANE ( 'NONE',  #50671 ) ;
#45742 = VERTEX_POINT ( 'NONE', #96288 ) ;
#45743 = CARTESIAN_POINT ( 'NONE',  ( -99.77167476857428596, -25.07038923500906691, 7.433068779553578587 ) ) ;
#45744 = CARTESIAN_POINT ( 'NONE',  ( -8.122062702759739850, 17.86989387945112995, 11.49999999999999645 ) ) ;
#45745 = LINE ( 'NONE', #69077, #1746 ) ;
#45746 = B_SPLINE_CURVE_WITH_KNOTS ( 'NONE', 3,
 ( #92232, #84122, #93229, #76496 ),
 .UNSPECIFIED., .F., .F.,
 ( 4, 4 ),
 ( 0.3607576081775127896, 0.3697640394496283234 ),
 .UNSPECIFIED. ) ;
#45747 = CARTESIAN_POINT ( 'NONE',  ( 13.91401389203221406, 0.3587747205144265483, 158.0376437107427137 ) ) ;
#45748 = ORIENTED_EDGE ( 'NONE', *, *, #43892, .T. ) ;
#45749 = CARTESIAN_POINT ( 'NONE',  ( -88.54317737591240700, -24.66019654487199730, 8.947790411086115725 ) ) ;
#45750 = CARTESIAN_POINT ( 'NONE',  ( -126.3655805143406354, -25.31862575908220947, 6.461926907689274024 ) ) ;
#45751 = EDGE_CURVE ( 'NONE', #8583, #40108, #41505, .T. ) ;
#45752 = CARTESIAN_POINT ( 'NONE',  ( -124.5544995689860883, -24.51419770103158768, 9.386484678747164523 ) ) ;
#45753 = CARTESIAN_POINT ( 'NONE',  ( -10.60818629614422370, 16.63341085705455669, -1.500000000000002220 ) ) ;
#45754 = VERTEX_POINT ( 'NONE', #58236 ) ;
#45755 = AXIS2_PLACEMENT_3D ( 'NONE', #72358, #33276, #87068 ) ;
#45756 = AXIS2_PLACEMENT_3D ( 'NONE', #61147, #99176, #13446 ) ;
#45757 = CARTESIAN_POINT ( 'NONE',  ( 10.93823315965619791, 6.376774720514427841, -24.99764212866241309 ) ) ;
#45758 = DIRECTION ( 'NONE',  ( 0.000000000000000000, -1.000000000000000000, 0.000000000000000000 ) ) ;
#45759 = SECURITY_CLASSIFICATION_LEVEL ( 'unclassified' ) ;
#45760 = VERTEX_POINT ( 'NONE', #18160 ) ;
#45761 = DIRECTION ( 'NONE',  ( 0.000000000000000000, 0.9967269304714136968, 0.08084198211964954695 ) ) ;
#45762 = CARTESIAN_POINT ( 'NONE',  ( 6.420673076923079314, -6.376774720514427841, 21.83974358974358765 ) ) ;
#45763 = CARTESIAN_POINT ( 'NONE',  ( -55.62855502628812587, -24.83618233451449697, 1.606449574219536602 ) ) ;
#45764 = CARTESIAN_POINT ( 'NONE',  ( -100.2380303841250395, -25.26638540230637631, 7.557070759772178015 ) ) ;
#45765 = CARTESIAN_POINT ( 'NONE',  ( -1.595974963000059477, -5.876774720514409189, 19.39236848396478408 ) ) ;
#45766 = DIRECTION ( 'NONE',  ( 0.000000000000000000, -2.173523156925979552E-06, 0.9999999999976378895 ) ) ;
#45767 = CARTESIAN_POINT ( 'NONE',  ( 20.07151214508649772, 3.809612236891415094E-15, -1.699999999999999956 ) ) ;
#45769 = EDGE_CURVE ( 'NONE', #56886, #12265, #57249, .T. ) ;
#45768 = CARTESIAN_POINT ( 'NONE',  ( 18.82558416981596139, 6.732768832687442639, -1.500000000000002220 ) ) ;
#45770 = CARTESIAN_POINT ( 'NONE',  ( -72.62287095715005592, -29.50247984919015209, -1.443849546365055359 ) ) ;
#45771 = CARTESIAN_POINT ( 'NONE',  ( -45.67376991709483036, -23.48786465467240703, 11.44779295918255002 ) ) ;
#45772 = ORIENTED_EDGE ( 'NONE', *, *, #22832, .T. ) ;
#45773 = VECTOR ( 'NONE', #88319, 1000.000000000000000 ) ;
#45775 = CARTESIAN_POINT ( 'NONE',  ( -119.6256461673538354, -24.15543982623907837, -0.2315651400026546569 ) ) ;
#45774 = LOCAL_TIME ( 0, 54, 15.00000000000000000, #61495 ) ;
#45776 = CARTESIAN_POINT ( 'NONE',  ( -80.64599816240546204, -23.85049219812686161, 10.88485053497527311 ) ) ;
#45777 = EDGE_CURVE ( 'NONE', #79765, #3681, #97066, .T. ) ;
#45778 = CARTESIAN_POINT ( 'NONE',  ( -51.52287095715006870, -29.50247984919015209, -1.443849546365058689 ) ) ;
#45779 = CARTESIAN_POINT ( 'NONE',  ( -61.62287095715004881, -24.66019654487199020, 8.947790411086131712 ) ) ;
#45780 = B_SPLINE_CURVE_WITH_KNOTS ( 'NONE', 3,
 ( #81585, #97304, #59245, #12055, #20664, #12560 ),
 .UNSPECIFIED., .F., .F.,
 ( 4, 2, 4 ),
 ( 0.000000000000000000, 0.001380764517853252287, 0.002761529035706504574 ),
 .UNSPECIFIED. ) ;
#45781 = ADVANCED_FACE ( 'NONE', ( #20149 ), #3948, .T. ) ;
#45782 = DIRECTION ( 'NONE',  ( 0.000000000000000000, 0.000000000000000000, 1.000000000000000000 ) ) ;
#45783 = CARTESIAN_POINT ( 'NONE',  ( -45.58953762381671027, -25.00182538069144655, 7.747789668545102870 ) ) ;
#45784 = CARTESIAN_POINT ( 'NONE',  ( -58.62287095715004881, -24.66019654487199020, 8.947790411086131712 ) ) ;
#45785 = CIRCLE ( 'NONE', #58987, 10.11363636363636154 ) ;
#45786 = CARTESIAN_POINT ( 'NONE',  ( 0.2196812790064107401, -5.876774720514409189, 19.42522865122897002 ) ) ;
#45787 = EDGE_LOOP ( 'NONE', ( #22233, #4371, #35341, #15838 ) ) ;
#45788 = CARTESIAN_POINT ( 'NONE',  ( -14.64122064730360862, 14.02963135428074004, 11.49999999999998934 ) ) ;
#45789 = VECTOR ( 'NONE', #43230, 1000.000000000000000 ) ;
#45790 = CARTESIAN_POINT ( 'NONE',  ( -61.52287095715007581, -23.47593901973090169, -1.443836447538997092 ) ) ;
#45791 = EDGE_CURVE ( 'NONE', #20125, #32109, #88638, .T. ) ;
#45792 = CARTESIAN_POINT ( 'NONE',  ( -29.49875734969025842, 0.3587747205144262708, 15.62202280011862321 ) ) ;
#45793 = CARTESIAN_POINT ( 'NONE',  ( -83.62287095715005592, -23.48783264082478794, -1.443836473390065711 ) ) ;
#45794 = VERTEX_POINT ( 'NONE', #82057 ) ;
#45795 = CARTESIAN_POINT ( 'NONE',  ( -72.52287095715010423, -24.66019654487199375, 8.947790411086128159 ) ) ;
#45796 = CARTESIAN_POINT ( 'NONE',  ( 10.61947033613929214, 17.11087026910869469, -1.500000000000002220 ) ) ;
#45797 = CARTESIAN_POINT ( 'NONE',  ( 0.4554788648648982474, -21.05657754196055009, 11.49999999999999645 ) ) ;
#45798 = CARTESIAN_POINT ( 'NONE',  ( -127.5228709571500616, -23.48786465467242479, 11.44779295918253581 ) ) ;
#45799 = CARTESIAN_POINT ( 'NONE',  ( -18.93877658415168241, -11.43451605920036052, -1.500000000000002220 ) ) ;
#45800 = CARTESIAN_POINT ( 'NONE',  ( -0.1859688948871585645, 20.53422428922035081, -1.500000000000002220 ) ) ;
#45801 = DIRECTION ( 'NONE',  ( 0.000000000000000000, 0.000000000000000000, 1.000000000000000000 ) ) ;
#45802 = AXIS2_PLACEMENT_3D ( 'NONE', #83549, #98769, #96917 ) ;
#45803 = DIRECTION ( 'NONE',  ( 0.000000000000000000, 0.000000000000000000, 1.000000000000000000 ) ) ;
#45804 = EDGE_LOOP ( 'NONE', ( #60928, #79152, #28197, #12857 ) ) ;
#45805 = DIRECTION ( 'NONE',  ( 0.000000000000000000, -2.173523156925980399E-06, 0.9999999999976378895 ) ) ;
#45806 = ORIENTED_EDGE ( 'NONE', *, *, #44763, .F. ) ;
#45807 = CARTESIAN_POINT ( 'NONE',  ( 16.30000000000000071, 2.681976490132703452E-15, -21.89999999999999858 ) ) ;
#45808 = CARTESIAN_POINT ( 'NONE',  ( -29.52287095715006515, -23.38906523657919578, -1.443836447538998424 ) ) ;
#45809 = ORIENTED_EDGE ( 'NONE', *, *, #54572, .F. ) ;
#45810 = ORIENTED_EDGE ( 'NONE', *, *, #64042, .T. ) ;
#45811 = ORIENTED_EDGE ( 'NONE', *, *, #98087, .F. ) ;
#45812 = CARTESIAN_POINT ( 'NONE',  ( -2.169994883066378222, 10.75358048763950869, -3.549999999999999822 ) ) ;
#45813 = CARTESIAN_POINT ( 'NONE',  ( -74.52287095715004739, -24.66019654487200441, 8.947790411086112172 ) ) ;
#45814 = CARTESIAN_POINT ( 'NONE',  ( -68.60862620934042866, -23.48786465467241058, 11.44779295918254824 ) ) ;
#45815 = CARTESIAN_POINT ( 'NONE',  ( 6.115004186001010922, -19.73231167505474559, -1.500000000000002220 ) ) ;
#45816 = CARTESIAN_POINT ( 'NONE',  ( -13.25059585359799108, -17.08168364658555305, 11.49999999999999645 ) ) ;
#45817 = ORIENTED_EDGE ( 'NONE', *, *, #4084, .F. ) ;
#45818 = VECTOR ( 'NONE', #35087, 1000.000000000000114 ) ;
#45819 = B_SPLINE_CURVE_WITH_KNOTS ( 'NONE', 3,
 ( #29822, #47426, #45066, #742 ),
 .UNSPECIFIED., .F., .F.,
 ( 4, 4 ),
 ( 0.000000000000000000, 9.999999999998897304E-05 ),
 .UNSPECIFIED. ) ;
#45820 = CARTESIAN_POINT ( 'NONE',  ( 2.100208336950355914, 0.000000000000000000, 0.000000000000000000 ) ) ;
#45821 = CARTESIAN_POINT ( 'NONE',  ( 5.717391271363888805, 6.376774720514426953, -25.39218285751184467 ) ) ;
#45822 = CARTESIAN_POINT ( 'NONE',  ( -18.94483701893047467, 11.91932228829616669, -1.500000000000002220 ) ) ;
#45823 = FACE_OUTER_BOUND ( 'NONE', #22714, .T. ) ;
#45824 = CARTESIAN_POINT ( 'NONE',  ( -67.62287095715005592, -29.50247984919015209, -1.443849546365055359 ) ) ;
#45825 = VERTEX_POINT ( 'NONE', #34390 ) ;
#45826 = CARTESIAN_POINT ( 'NONE',  ( -99.83329133075007178, -25.30639137160515872, 4.526400298129594546 ) ) ;
#45827 = CARTESIAN_POINT ( 'NONE',  ( -49.51415851261705825, -23.73791477778911840, 11.05961554403170943 ) ) ;
#45828 = B_SPLINE_CURVE_WITH_KNOTS ( 'NONE', 3,
 ( #28214, #59172, #88623, #67289 ),
 .UNSPECIFIED., .F., .F.,
 ( 4, 4 ),
 ( 0.000000000000000000, 1.000000000000000000 ),
 .UNSPECIFIED. ) ;
#45829 = VECTOR ( 'NONE', #39143, 1000.000000000000114 ) ;
#45830 = CARTESIAN_POINT ( 'NONE',  ( -33.52287095715006870, -24.50216790748204332, 0.6166512839542452884 ) ) ;
#45831 = CARTESIAN_POINT ( 'NONE',  ( -20.86263692406621928, 1.606387762444034362, -1.500000000000002220 ) ) ;
#45832 = ORIENTED_EDGE ( 'NONE', *, *, #97660, .F. ) ;
#45834 = ORIENTED_EDGE ( 'NONE', *, *, #48399, .T. ) ;
#45833 = CARTESIAN_POINT ( 'NONE',  ( -67.60893110983315069, -23.48786465467241058, 11.44779295918254824 ) ) ;
#45835 = ORIENTED_EDGE ( 'NONE', *, *, #25362, .T. ) ;
#45836 = EDGE_CURVE ( 'NONE', #30845, #100399, #87677, .T. ) ;
#45837 = CARTESIAN_POINT ( 'NONE',  ( -109.5507735056359451, -24.51419770103157347, 9.386484678747171628 ) ) ;
#45838 = CARTESIAN_POINT ( 'NONE',  ( 20.79131504077403747, 4.132458064796619368, -1.500000000000002220 ) ) ;
#45839 = ORIENTED_EDGE ( 'NONE', *, *, #22030, .T. ) ;
#45840 = CARTESIAN_POINT ( 'NONE',  ( -112.5228709571500900, -23.72773821059536914, 11.05748984161097326 ) ) ;
#45841 = CARTESIAN_POINT ( 'NONE',  ( -99.47310917600722746, -25.12215581454282542, 6.670037910655527646 ) ) ;
#45842 = CARTESIAN_POINT ( 'NONE',  ( 20.57308398666954119, -7.222494929537193187, -1.500000000000002220 ) ) ;
#45843 = CARTESIAN_POINT ( 'NONE',  ( -89.06226385320383088, -25.22391154813773895, 6.409327647370975711 ) ) ;
#45844 = CARTESIAN_POINT ( 'NONE',  ( -76.64821883033769723, -23.48786465467240703, 11.44779295918254647 ) ) ;
#45845 = CARTESIAN_POINT ( 'NONE',  ( -80.33745650938216443, -25.13434931566261099, 7.094763183326051603 ) ) ;
#45846 = CARTESIAN_POINT ( 'NONE',  ( 15.22768361601695020, -15.61070304372801587, -1.500000000000002220 ) ) ;
#45847 = CARTESIAN_POINT ( 'NONE',  ( -71.70841769935768184, -25.24674343745607885, 6.192981443898670335 ) ) ;
#45848 = ORIENTED_EDGE ( 'NONE', *, *, #39227, .F. ) ;
#45849 = CARTESIAN_POINT ( 'NONE',  ( 7.370931459274800090, -5.876774720514417183, 20.26286690110499578 ) ) ;
#45850 = LINE ( 'NONE', #77275, #84844 ) ;
#45851 = CARTESIAN_POINT ( 'NONE',  ( 282.9764569301858046, -5.152774720514427642, 20.79159422840526616 ) ) ;
#45852 = EDGE_LOOP ( 'NONE', ( #69265, #55702, #74888, #93699 ) ) ;
#45853 = ORIENTED_EDGE ( 'NONE', *, *, #86200, .F. ) ;
#45854 = CIRCLE ( 'NONE', #55569, 1.836000000000000743 ) ;
#45855 = ORIENTED_EDGE ( 'NONE', *, *, #90583, .F. ) ;
#45856 = CC_DESIGN_APPROVAL ( #61786, ( #19911 ) ) ;
#45857 = CARTESIAN_POINT ( 'NONE',  ( 30.93860345374796594, 0.6647747205144264315, 19.84760796525321780 ) ) ;
#45858 = CARTESIAN_POINT ( 'NONE',  ( 20.83148622972472808, -3.941400823363257366, -1.500000000000002220 ) ) ;
#45859 = LINE ( 'NONE', #85915, #51465 ) ;
#45860 = CARTESIAN_POINT ( 'NONE',  ( -95.62287095714994223, -24.62285846362214059, 9.038163152653520882 ) ) ;
#45861 = LINE ( 'NONE', #180, #56760 ) ;
#45862 = CARTESIAN_POINT ( 'NONE',  ( 2.230654205607476737, -0.1647943925233645579, -7.922169807384186089E-16 ) ) ;
#45863 = ADVANCED_FACE ( 'NONE', ( #4935 ), #95784, .F. ) ;
#45865 = CARTESIAN_POINT ( 'NONE',  ( -11.15089393765527959, -15.82809448842462885, -1.500000000000002220 ) ) ;
#45864 = VECTOR ( 'NONE', #92182, 1000.000000000000114 ) ;
#45866 = CARTESIAN_POINT ( 'NONE',  ( -39.98583224850788298, -25.11539320593059443, 2.804431443241629740 ) ) ;
#45867 = ORIENTED_EDGE ( 'NONE', *, *, #91640, .T. ) ;
#45868 = CARTESIAN_POINT ( 'NONE',  ( 4.201609111248720829, -18.99613120386805676, 11.49999999999999645 ) ) ;
#45869 = DIRECTION ( 'NONE',  ( 0.000000000000000000, 0.9999999999976377785, 2.173523156925979975E-06 ) ) ;
#45870 = EDGE_CURVE ( 'NONE', #17884, #94189, #58948, .T. ) ;
#45871 = CIRCLE ( 'NONE', #11819, 1.700000000000000178 ) ;
#45872 = B_SPLINE_CURVE_WITH_KNOTS ( 'NONE', 3,
 ( #80702, #10695, #11191, #73101 ),
 .UNSPECIFIED., .F., .F.,
 ( 4, 4 ),
 ( 0.000000000000000000, 9.999999999997510880E-05 ),
 .UNSPECIFIED. ) ;
#45873 = ORIENTED_EDGE ( 'NONE', *, *, #91905, .F. ) ;
#45874 = CARTESIAN_POINT ( 'NONE',  ( 3.052815417670126319, -5.876774720514407413, 18.46676085997033923 ) ) ;
#45875 = EDGE_CURVE ( 'NONE', #87834, #86594, #23180, .T. ) ;
#45876 = DIRECTION ( 'NONE',  ( -0.9994733861282923959, 0.000000000000000000, -0.03244919754393515293 ) ) ;
#45877 = ADVANCED_FACE ( 'NONE', ( #50613 ), #46784, .T. ) ;
#45878 = PLANE ( 'NONE',  #29315 ) ;
#45879 = CARTESIAN_POINT ( 'NONE',  ( -93.60100369702254852, -23.48786465467241058, 11.44779295918254469 ) ) ;
#45880 = CARTESIAN_POINT ( 'NONE',  ( 18.70796670040472165, 5.986831462552164140, 11.49999999999998934 ) ) ;
#45881 = B_SPLINE_SURFACE_WITH_KNOTS ( 'NONE', 3, 1, ( 
 ( #82001, #27221 ),
 ( #41445, #72402 ),
 ( #33826, #51060 ),
 ( #65312, #81508 ),
 ( #88124, #64813 ),
 ( #26217, #2897 ),
 ( #49567, #65802 ) ),
 .UNSPECIFIED., .F., .F., .F.,
 ( 4, 1, 1, 1, 4 ),
 ( 2, 2 ),
 ( 0.000000000000000000, 0.2499864026691206442, 0.4969648798681433055, 0.7462659243093390238, 1.000000000000000000 ),
 ( 0.000000000000000000, 1.000000000000000000 ),
 .UNSPECIFIED. ) ;
#45882 = CARTESIAN_POINT ( 'NONE',  ( -41.42418673051398770, -25.27806002644363303, 4.451104005806604036 ) ) ;
#45884 = EDGE_CURVE ( 'NONE', #73093, #52694, #31320, .T. ) ;
#45883 = ORIENTED_EDGE ( 'NONE', *, *, #19962, .T. ) ;
#45885 = CARTESIAN_POINT ( 'NONE',  ( 8.794441374123232791, -19.68457759291379716, -1.500000000000002220 ) ) ;
#45886 = CARTESIAN_POINT ( 'NONE',  ( -33.65850923073764989, -23.73791477778911130, 11.05961554403171299 ) ) ;
#45887 = CARTESIAN_POINT ( 'NONE',  ( -73.92287095715006728, -23.47593901973090169, -1.443836447538997536 ) ) ;
#45888 = CARTESIAN_POINT ( 'NONE',  ( -121.5562042904833788, -24.64898659630529210, 1.056161002820831030 ) ) ;
#45889 = CARTESIAN_POINT ( 'NONE',  ( 6.753845092018655016, 22.03294598498517232, -1.500000000000002220 ) ) ;
#45890 = PERSON_AND_ORGANIZATION ( #70597, #27821 ) ;
#45891 = CARTESIAN_POINT ( 'NONE',  ( -93.59418303358040703, -23.96119346886880663, -0.6495511937832079141 ) ) ;
#45892 = CARTESIAN_POINT ( 'NONE',  ( -51.31007370257843547, -25.18370859199909972, 3.285367768258824483 ) ) ;
#45893 = CARTESIAN_POINT ( 'NONE',  ( 12.15850541088210868, 16.18036119754114566, 11.49999999999999645 ) ) ;
#45894 = CARTESIAN_POINT ( 'NONE',  ( -121.5213653170695096, -23.73791477778912551, 11.05961554403170055 ) ) ;
#45895 = DIRECTION ( 'NONE',  ( 0.000000000000000000, 1.000000000000000000, -0.000000000000000000 ) ) ;
#45896 = CARTESIAN_POINT ( 'NONE',  ( -111.7814946224345789, -25.10921699980403687, 4.332404819734247958 ) ) ;
#45897 = PLANE ( 'NONE',  #76386 ) ;
#45898 = DIRECTION ( 'NONE',  ( 0.000000000000000000, 1.000000000000000000, -0.000000000000000000 ) ) ;
#45900 = EDGE_CURVE ( 'NONE', #96177, #7232, #84608, .T. ) ;
#45899 = CARTESIAN_POINT ( 'NONE',  ( 18.24224480919323810, -7.949361806615760528, 11.49999999999998934 ) ) ;
#45901 = VECTOR ( 'NONE', #79390, 1000.000000000000000 ) ;
#45902 = LINE ( 'NONE', #710, #57764 ) ;
#45903 = CARTESIAN_POINT ( 'NONE',  ( -19.76903914530799966, 0.2396048511829373395, -1.500000000000002220 ) ) ;
#45904 = CARTESIAN_POINT ( 'NONE',  ( 0.3849403830293018358, -5.876774720514418959, 20.45311193189268906 ) ) ;
#45905 = VECTOR ( 'NONE', #98050, 1000.000000000000000 ) ;
#45906 = DESIGN_CONTEXT ( 'detailed design', #40771, 'design' ) ;
#45907 = CARTESIAN_POINT ( 'NONE',  ( 33.00535138976610483, -5.965225279485572685, -12.97242311383961066 ) ) ;
#45908 = CARTESIAN_POINT ( 'NONE',  ( -105.5228709571500616, -24.99132157543084887, 2.256160258750667502 ) ) ;
#45909 = CARTESIAN_POINT ( 'NONE',  ( -4.528870947376731237, 20.18191347215651987, 11.49999999999999645 ) ) ;
#45910 = CARTESIAN_POINT ( 'NONE',  ( 13.57151214508650305, -0.8999999999999998002, 1.500000000000000666 ) ) ;
#45911 = EDGE_CURVE ( 'NONE', #16912, #1680, #87469, .T. ) ;
#45912 = CARTESIAN_POINT ( 'NONE',  ( -39.52287095715006870, -24.66019654487198665, 8.947790411086131712 ) ) ;
#45913 = CARTESIAN_POINT ( 'NONE',  ( -0.6305239314742796530, -22.70799625201654592, 11.49999999999999645 ) ) ;
#45914 = VERTEX_POINT ( 'NONE', #91710 ) ;
#45915 = CARTESIAN_POINT ( 'NONE',  ( -67.52287095715003318, -23.47593901973090169, -1.443836447538996870 ) ) ;
#45916 = EDGE_CURVE ( 'NONE', #82569, #91875, #69888, .T. ) ;
#45917 = CARTESIAN_POINT ( 'NONE',  ( -74.62287095715005592, -23.96177878511307924, 10.65340807706329862 ) ) ;
#45918 = CARTESIAN_POINT ( 'NONE',  ( 12.02422309597069017, 16.21794576832014556, 11.49999999999998934 ) ) ;
#45919 = CARTESIAN_POINT ( 'NONE',  ( 8.974114877419671288, -0.9738252115640718687, -3.736985260579223311 ) ) ;
#45920 = EDGE_CURVE ( 'NONE', #23547, #64340, #47063, .T. ) ;
#45921 = CARTESIAN_POINT ( 'NONE',  ( -52.55620429048339304, -23.47593901973091235, -1.443836447539009749 ) ) ;
#45922 = ORIENTED_EDGE ( 'NONE', *, *, #11089, .F. ) ;
#45923 = EDGE_CURVE ( 'NONE', #12467, #52403, #74182, .T. ) ;
#45924 = VERTEX_POINT ( 'NONE', #75982 ) ;
#45925 = VECTOR ( 'NONE', #85203, 1000.000000000000227 ) ;
#45926 = PLANE ( 'NONE',  #95459 ) ;
#45927 = CARTESIAN_POINT ( 'NONE',  ( 19.54225192528841859, -11.95493969655435151, 11.49999999999998934 ) ) ;
#45929 = EDGE_CURVE ( 'NONE', #88329, #44867, #76981, .T. ) ;
#45928 = CARTESIAN_POINT ( 'NONE',  ( -50.43601667505130592, -25.18439649994563823, 3.294780684294133177 ) ) ;
#45930 = CARTESIAN_POINT ( 'NONE',  ( -3.891998276399621481, 21.28400606017829233, -1.500000000000002220 ) ) ;
#45931 = CARTESIAN_POINT ( 'NONE',  ( -123.6266572008115787, -23.48783264082477373, -1.443836473390086361 ) ) ;
#45932 = CARTESIAN_POINT ( 'NONE',  ( -34.64253015005402858, -24.15543982623907127, -0.2315651400026574880 ) ) ;
#45933 = CARTESIAN_POINT ( 'NONE',  ( 8.468106961216914641, 19.09613275528424836, 11.49999999999999645 ) ) ;
#45934 = EDGE_LOOP ( 'NONE', ( #95859, #49082, #36221, #48581 ) ) ;
#45935 = CARTESIAN_POINT ( 'NONE',  ( -124.5222546880168437, -23.48783264082477373, -1.443836473390086139 ) ) ;
#45936 = CARTESIAN_POINT ( 'NONE',  ( -21.12052157030387889, 6.262089831203976331, 11.49999999999998934 ) ) ;
#45937 = CARTESIAN_POINT ( 'NONE',  ( -105.5864560779018433, -24.83644354573579349, 8.397322867130096569 ) ) ;
#45938 = CARTESIAN_POINT ( 'NONE',  ( -41.86334916006617135, -25.29087293436575479, 4.024172904988462918 ) ) ;
#45939 = VECTOR ( 'NONE', #91067, 1000.000000000000000 ) ;
#45940 = VERTEX_POINT ( 'NONE', #16093 ) ;
#45941 = CARTESIAN_POINT ( 'NONE',  ( 1.000208336950358934, 0.000000000000000000, 0.000000000000000000 ) ) ;
#45942 = DIRECTION ( 'NONE',  ( -5.204170427930421283E-15, 1.000000000000000000, 0.000000000000000000 ) ) ;
#45943 = VERTEX_POINT ( 'NONE', #7477 ) ;
#45944 = DIRECTION ( 'NONE',  ( -3.773278334453079618E-23, 0.9999999999976377785, 2.173523156925978705E-06 ) ) ;
#45945 = ORIENTED_EDGE ( 'NONE', *, *, #65753, .F. ) ;
#45946 = VECTOR ( 'NONE', #8037, 1000.000000000000114 ) ;
#45947 = ORIENTED_EDGE ( 'NONE', *, *, #14342, .F. ) ;
#45948 = CARTESIAN_POINT ( 'NONE',  ( -71.53799170295864940, -24.66019654487199730, 8.947790411086113949 ) ) ;
#45949 = CARTESIAN_POINT ( 'NONE',  ( -95.62287095715002749, -24.15516710230295416, 10.28746687063724785 ) ) ;
#45950 = CARTESIAN_POINT ( 'NONE',  ( -4.243469080022288509, -5.876774720514411854, 19.94806476610987644 ) ) ;
#45951 = CARTESIAN_POINT ( 'NONE',  ( -16.48689143942861079, 12.14541645011370541, -1.500000000000002220 ) ) ;
#45952 = ORIENTED_EDGE ( 'NONE', *, *, #39411, .T. ) ;
#45953 = CARTESIAN_POINT ( 'NONE',  ( 10.54059822343757880, -5.876774720514426953, 22.82308057603841078 ) ) ;
#45954 = DIRECTION ( 'NONE',  ( -0.02119372647573786531, -9.594337693711052596E-15, -0.9997753877537052247 ) ) ;
#45955 = DIRECTION ( 'NONE',  ( -3.469446951953614189E-15, 1.000000000000000000, 0.000000000000000000 ) ) ;
#45956 = CARTESIAN_POINT ( 'NONE',  ( 9.404896790668452411, 20.21284700076377305, 11.49999999999998934 ) ) ;
#45957 = DIRECTION ( 'NONE',  ( 0.000000000000000000, -1.000000000000000000, 0.000000000000000000 ) ) ;
#45958 = CARTESIAN_POINT ( 'NONE',  ( -88.62287095715002749, -24.66019654487199730, 8.947790411086128159 ) ) ;
#45959 = ORIENTED_EDGE ( 'NONE', *, *, #22983, .F. ) ;
#45960 = CARTESIAN_POINT ( 'NONE',  ( 0.02224039135773590858, 0.3828044741864812250, -0.3828044741864797817 ) ) ;
#45961 = CARTESIAN_POINT ( 'NONE',  ( -86.62287095715004170, -24.64898659630528854, 1.056161002820827921 ) ) ;
#45962 = CARTESIAN_POINT ( 'NONE',  ( 8.324980675869593227, 19.10421180063631752, 11.49999999999998934 ) ) ;
#45963 = ORIENTED_EDGE ( 'NONE', *, *, #24913, .F. ) ;
#45965 = VERTEX_POINT ( 'NONE', #92708 ) ;
#45964 = CARTESIAN_POINT ( 'NONE',  ( 4.627238781264984446, -6.376774720514408301, 19.49219360614394247 ) ) ;
#45966 = B_SPLINE_SURFACE_WITH_KNOTS ( 'NONE', 3, 3, ( 
 ( #8688, #95919, #17292, #24899 ),
 ( #95420, #26413, #79689, #40643 ),
 ( #48257, #2584, #55370, #85808 ),
 ( #47755, #79188, #16288, #1075 ),
 ( #33026, #62990, #64002, #33521 ),
 ( #94916, #9177, #1583, #40138 ),
 ( #25407, #56382, #17801, #10186 ) ),
 .UNSPECIFIED., .F., .F., .F.,
 ( 4, 3, 4 ),
 ( 4, 4 ),
 ( 0.7945040050992253633, 0.8970133687736512318, 0.9995227324480769893 ),
 ( 0.9897455052912615958, 0.9912151620501660210 ),
 .UNSPECIFIED. ) ;
#45967 = CARTESIAN_POINT ( 'NONE',  ( -51.52589570729855950, -25.25854379533914695, 6.227983929447254319 ) ) ;
#45968 = ORIENTED_EDGE ( 'NONE', *, *, #78779, .T. ) ;
#45969 = VERTEX_POINT ( 'NONE', #54182 ) ;
#45970 = DIRECTION ( 'NONE',  ( -1.000000000000000000, -0.000000000000000000, -0.000000000000000000 ) ) ;
#45971 = CARTESIAN_POINT ( 'NONE',  ( -121.5562042904833788, -23.48786465467241769, 11.44779295918253759 ) ) ;
#45972 = CARTESIAN_POINT ( 'NONE',  ( 9.405830370894557646, -5.356774720514425603, -24.99732136569351226 ) ) ;
#45973 = DIRECTION ( 'NONE',  ( -3.773278334453079030E-23, 0.9999999999976377785, 2.173523156925979128E-06 ) ) ;
#45974 = DIRECTION ( 'NONE',  ( -3.773278334444166432E-23, 1.000000000000000000, 0.000000000000000000 ) ) ;
#45975 = DIRECTION ( 'NONE',  ( 3.773278334444166432E-23, -1.000000000000000000, 0.000000000000000000 ) ) ;
#45977 = ORIENTED_EDGE ( 'NONE', *, *, #86529, .T. ) ;
#45976 = CARTESIAN_POINT ( 'NONE',  ( 17.03105324785762420, 14.15717209551829647, 11.49999999999999645 ) ) ;
#45978 = CARTESIAN_POINT ( 'NONE',  ( -28.98875734969026396, -5.965225279485572685, 10.11402280011862587 ) ) ;
#45979 = AXIS2_PLACEMENT_3D ( 'NONE', #4796, #59092, #19011 ) ;
#45980 = CARTESIAN_POINT ( 'NONE',  ( 0.4201012023153268271, 22.63755686032812164, 11.49999999999998934 ) ) ;
#45982 = ORIENTED_EDGE ( 'NONE', *, *, #55190, .T. ) ;
#45981 = CARTESIAN_POINT ( 'NONE',  ( -92.52287095715003318, -24.51283580621460345, 0.6167428607048187628 ) ) ;
#45983 = B_SPLINE_CURVE_WITH_KNOTS ( 'NONE', 3,
 ( #61508, #29038, #38145, #45278, #77197, #44780 ),
 .UNSPECIFIED., .F., .F.,
 ( 4, 2, 4 ),
 ( 0.000000000000000000, 0.001380764517853255323, 0.002761529035706510645 ),
 .UNSPECIFIED. ) ;
#45984 = CIRCLE ( 'NONE', #21621, 1.150000000000003464 ) ;
#45985 = EDGE_LOOP ( 'NONE', ( #41682, #86276, #27109, #25714 ) ) ;
#45986 = CARTESIAN_POINT ( 'NONE',  ( -99.62287095715005592, -24.65952944569304961, 1.056160979905702124 ) ) ;
#45987 = EDGE_CURVE ( 'NONE', #89509, #35626, #85106, .T. ) ;
#45988 = CARTESIAN_POINT ( 'NONE',  ( -20.11654390397962544, -0.4351469013266864860, 11.49999999999998934 ) ) ;
#45989 = CARTESIAN_POINT ( 'NONE',  ( 33.00535138976610483, 5.965225279485572685, -12.97242311383961066 ) ) ;
#45990 = ORIENTED_EDGE ( 'NONE', *, *, #57691, .F. ) ;
#45991 = CARTESIAN_POINT ( 'NONE',  ( 15.77421270221671179, -3.602820947333605250, -28.08718493694522422 ) ) ;
#45992 = CARTESIAN_POINT ( 'NONE',  ( -4.763361739610138201, -21.85411462188651299, -1.500000000000002220 ) ) ;
#45993 = ORIENTED_EDGE ( 'NONE', *, *, #66868, .F. ) ;
#45994 = ORIENTED_EDGE ( 'NONE', *, *, #6609, .T. ) ;
#45995 = CARTESIAN_POINT ( 'NONE',  ( -101.4413695709857990, -25.16257366102977144, 6.524206556767607523 ) ) ;
#45996 = CARTESIAN_POINT ( 'NONE',  ( -81.87214700851818350, -25.22769362155178641, 6.379145389457276494 ) ) ;
#45997 = FACE_BOUND ( 'NONE', #48863, .T. ) ;
#45998 = EDGE_CURVE ( 'NONE', #63531, #149, #25708, .T. ) ;
#45999 = ADVANCED_FACE ( 'NONE', ( #10483 ), #48574, .F. ) ;
#46000 = CARTESIAN_POINT ( 'NONE',  ( -68.52287095715004739, -24.51387760970724372, 9.387446482453414731 ) ) ;
#46001 = EDGE_CURVE ( 'NONE', #38118, #2589, #93715, .T. ) ;
#46002 = CARTESIAN_POINT ( 'NONE',  ( -8.499999999999987566, 18.74999999999999645, 2.100000000000000089 ) ) ;
#46003 = CARTESIAN_POINT ( 'NONE',  ( 15.26536572251939461, -12.21375333317339695, -1.500000000000002220 ) ) ;
#46004 = DIRECTION ( 'NONE',  ( 0.000000000000000000, -0.9999999999976377785, -2.173523156925979975E-06 ) ) ;
#46005 = EDGE_CURVE ( 'NONE', #3440, #79116, #9487, .T. ) ;
#46006 = CARTESIAN_POINT ( 'NONE',  ( -20.95461191387366284, 4.708766595171775649, -1.500000000000002220 ) ) ;
#46007 = FACE_OUTER_BOUND ( 'NONE', #29011, .T. ) ;
#46008 = DIRECTION ( 'NONE',  ( -1.000000000000000000, 0.000000000000000000, 0.000000000000000000 ) ) ;
#46009 = CARTESIAN_POINT ( 'NONE',  ( -129.5228709571501042, -23.96177878511308990, 10.65340807706329329 ) ) ;
#46010 = CARTESIAN_POINT ( 'NONE',  ( 1.119804705421552748, 22.86502198858056545, -1.500000000000002220 ) ) ;
#46011 = VECTOR ( 'NONE', #87692, 1000.000000000000114 ) ;
#46012 = MECHANICAL_CONTEXT ( 'NONE', #34267, 'mechanical' ) ;
#46013 = CARTESIAN_POINT ( 'NONE',  ( -8.499999999999987566, 18.99999999999977973, 2.100000000000000089 ) ) ;
#46014 = CARTESIAN_POINT ( 'NONE',  ( -2.794871794871795156, -5.876774720514418071, 20.36318108974359475 ) ) ;
#46015 = CARTESIAN_POINT ( 'NONE',  ( 19.28819943863484454, -5.468471092112969778, 11.49999999999999645 ) ) ;
#46016 = CARTESIAN_POINT ( 'NONE',  ( -79.58953762381672448, -23.48783264082478794, -1.443836473390065489 ) ) ;
#46017 = DIRECTION ( 'NONE',  ( -3.773278334453079030E-23, 0.9999999999976377785, 2.173523156925979128E-06 ) ) ;
#46018 = VECTOR ( 'NONE', #21151, 1000.000000000000000 ) ;
#46019 = CARTESIAN_POINT ( 'NONE',  ( -29.49875734969026198, 5.965225279485572685, 0.1180228001186258285 ) ) ;
#46020 = FACE_OUTER_BOUND ( 'NONE', #94750, .T. ) ;
#46021 = VERTEX_POINT ( 'NONE', #48059 ) ;
#46022 = DIRECTION ( 'NONE',  ( -3.389844910009033029E-15, 1.000000000000000000, 0.000000000000000000 ) ) ;
#46023 = ADVANCED_FACE ( 'NONE', ( #87619 ), #39937, .F. ) ;
#46024 = CARTESIAN_POINT ( 'NONE',  ( -115.6228709571500559, -23.48786465467242479, 11.44779295918253759 ) ) ;
#46025 = CARTESIAN_POINT ( 'NONE',  ( 20.88924836996103451, 6.054424527964996194, 11.49999999999998934 ) ) ;
#46026 = CARTESIAN_POINT ( 'NONE',  ( -45.52287095715007581, -24.83620972994591725, 8.398175272781367440 ) ) ;
#46027 = CARTESIAN_POINT ( 'NONE',  ( 19.39309126630920588, -2.812899550206792831, -1.500000000000002220 ) ) ;
#46028 = CARTESIAN_POINT ( 'NONE',  ( -59.56094173781918499, -29.50249039766296022, 3.409318347773680369 ) ) ;
#46029 = EDGE_CURVE ( 'NONE', #60699, #17009, #45984, .T. ) ;
#46030 = CARTESIAN_POINT ( 'NONE',  ( -110.0852742341990904, -25.31698216522971379, 5.455857398936061031 ) ) ;
#46031 = CALENDAR_DATE ( 2026, 9, 10 ) ;
#46032 = CARTESIAN_POINT ( 'NONE',  ( 29.73860345376319003, -4.772774720514425972, -4.021180035027960287 ) ) ;
#46033 = CARTESIAN_POINT ( 'NONE',  ( 2.787364042957740651, -6.376774720514424288, 21.14548745790758488 ) ) ;
#46034 = CARTESIAN_POINT ( 'NONE',  ( 17.04084431845542369, 11.38269047019995206, 11.49999999999999645 ) ) ;
#46035 = CARTESIAN_POINT ( 'NONE',  ( -39.29848179823069643, -25.31692503256359572, 5.130235141806659627 ) ) ;
#46036 = EDGE_CURVE ( 'NONE', #84750, #29911, #65648, .T. ) ;
#46037 = FACE_OUTER_BOUND ( 'NONE', #42370, .T. ) ;
#46038 = ORIENTED_EDGE ( 'NONE', *, *, #60918, .F. ) ;
#46039 =( NAMED_UNIT ( * ) PLANE_ANGLE_UNIT ( ) SI_UNIT ( $, .RADIAN. ) );
#46040 = CARTESIAN_POINT ( 'NONE',  ( -62.52287095715009002, -23.95044443724992078, 10.65354141964649592 ) ) ;
#46041 = CARTESIAN_POINT ( 'NONE',  ( -9.940598223437577374, -6.376774720514426953, 17.91871304725684766 ) ) ;
#46042 = CARTESIAN_POINT ( 'NONE',  ( -125.5194281211166896, -24.92592662359561828, 8.075495903018000021 ) ) ;
#46043 = DIRECTION ( 'NONE',  ( 0.000000000000000000, 0.000000000000000000, -1.000000000000000000 ) ) ;
#46044 = CARTESIAN_POINT ( 'NONE',  ( -51.93149462243456327, -29.50249640685361641, 6.174041905459458413 ) ) ;
#46045 = VECTOR ( 'NONE', #113, 1000.000000000000114 ) ;
#46046 = CARTESIAN_POINT ( 'NONE',  ( 30.32108885906865936, 6.376774720514427841, 3.274824222184972822 ) ) ;
#46047 = EDGE_CURVE ( 'NONE', #74508, #89020, #29750, .T. ) ;
#46048 = CARTESIAN_POINT ( 'NONE',  ( -21.01138170180016118, -9.542296329091309204, 11.49999999999999645 ) ) ;
#46049 = CARTESIAN_POINT ( 'NONE',  ( 22.20067557195093855, 5.203973054738295190, 11.49999999999998934 ) ) ;
#46050 = CARTESIAN_POINT ( 'NONE',  ( 4.547289707988324103, -5.876774720514410966, 19.12266226838056582 ) ) ;
#46051 = VECTOR ( 'NONE', #29075, 1000.000000000000000 ) ;
#46052 = CARTESIAN_POINT ( 'NONE',  ( 15.63605935613269438, 5.965225279485572685, -27.55169773172585934 ) ) ;
#46053 = CARTESIAN_POINT ( 'NONE',  ( -0.02075734969026423599, -5.965225279485572685, -0.08597719988137648983 ) ) ;
#46054 = CARTESIAN_POINT ( 'NONE',  ( 22.37589550080693712, 1.095942408959037273, 11.49999999999999645 ) ) ;
#46055 = CARTESIAN_POINT ( 'NONE',  ( -74.52287095715004739, -24.66019654487200441, 8.947790411086112172 ) ) ;
#46056 = CARTESIAN_POINT ( 'NONE',  ( -47.52287095715006160, -23.48786465467240347, 11.44779295918255002 ) ) ;
#46057 = EDGE_CURVE ( 'NONE', #87641, #19622, #60893, .T. ) ;
#46058 = CARTESIAN_POINT ( 'NONE',  ( 0.1985894851802381678, 21.93841921393417849, 11.49999999999998934 ) ) ;
#46059 = CARTESIAN_POINT ( 'NONE',  ( -5.115065434581078208, -5.876774720514408301, 19.15054976246387497 ) ) ;
#46060 = CARTESIAN_POINT ( 'NONE',  ( -87.62875044884228259, -24.35071581493543391, 9.817618358456025263 ) ) ;
#46061 = DIRECTION ( 'NONE',  ( 1.000000000000000000, 3.773278334444167608E-23, 8.201307833595939069E-29 ) ) ;
#46062 = CARTESIAN_POINT ( 'NONE',  ( -48.90931483959620607, -25.21642463136752710, 6.474588610440971337 ) ) ;
#46063 = CARTESIAN_POINT ( 'NONE',  ( 22.02124265030973760, 7.743225279485574042, 16.20402280011862217 ) ) ;
#46064 = ORIENTED_EDGE ( 'NONE', *, *, #54936, .F. ) ;
#46065 = CARTESIAN_POINT ( 'NONE',  ( -17.80769721941407369, -10.09151516499986734, 11.49999999999998934 ) ) ;
#46066 = VERTEX_POINT ( 'NONE', #18102 ) ;
#46067 = ORIENTED_EDGE ( 'NONE', *, *, #13678, .T. ) ;
#46068 = ORIENTED_EDGE ( 'NONE', *, *, #31121, .T. ) ;
#46069 = ORIENTED_EDGE ( 'NONE', *, *, #11312, .F. ) ;
#46070 = CARTESIAN_POINT ( 'NONE',  ( 14.79121776280621425, -17.69394282334246427, 11.49999999999998934 ) ) ;
#46071 = FACE_OUTER_BOUND ( 'NONE', #48738, .T. ) ;
#46072 = B_SPLINE_CURVE_WITH_KNOTS ( 'NONE', 3,
 ( #86819, #72114, #3110, #10203, #73114, #2605, #65022, #48271, #95936, #64524, #57403, #88331, #3601, #9700, #80718, #95436, #18807, #34546, #79202 ),
 .UNSPECIFIED., .F., .F.,
 ( 4, 1, 1, 1, 1, 1, 1, 1, 1, 1, 1, 1, 1, 1, 1, 1, 4 ),
 ( 0.000000000000000000, 0.07560433049574560860, 0.1479650154827357456, 0.2187969985237000203, 0.2894704453213765016, 0.3597242180874995476, 0.4297077387530455206, 0.5004965198485865630, 0.5744290198679483650, 0.6139472962286703916, 0.6571552698261112768, 0.7039727697209375856, 0.7549389848168005512, 0.8097066112894875101, 0.8688329536985499590, 0.9323854739325975194, 1.000000000000000000 ),
 .UNSPECIFIED. ) ;
#46073 = CARTESIAN_POINT ( 'NONE',  ( -18.19507518397214341, 8.946258903265221107, -1.500000000000002220 ) ) ;
#46074 = ORIENTED_EDGE ( 'NONE', *, *, #56955, .T. ) ;
#46075 = CARTESIAN_POINT ( 'NONE',  ( -30.30596983276391754, -23.44958398067863925, 11.44779298504228038 ) ) ;
#46076 = LINE ( 'NONE', #76995, #20654 ) ;
#46077 = CARTESIAN_POINT ( 'NONE',  ( -101.1944152955115186, -25.17323144036708626, 6.858246026757193192 ) ) ;
#46078 = PLANE ( 'NONE',  #36673 ) ;
#46080 = ORIENTED_EDGE ( 'NONE', *, *, #9119, .F. ) ;
#46079 = CARTESIAN_POINT ( 'NONE',  ( -5.333777546869826303, -20.73983961313815172, 11.49999999999999645 ) ) ;
#46081 = DIRECTION ( 'NONE',  ( 0.8219392559241306406, -0.08114015731558522904, -0.5637660281018079811 ) ) ;
#46082 = DIRECTION ( 'NONE',  ( 0.000000000000000000, 0.000000000000000000, -1.000000000000000000 ) ) ;
#46083 = ORIENTED_EDGE ( 'NONE', *, *, #16259, .F. ) ;
#46084 = CARTESIAN_POINT ( 'NONE',  ( -17.53982812869053731, -11.02811673548155902, -1.500000000000002220 ) ) ;
#46085 = VERTEX_POINT ( 'NONE', #71398 ) ;
#46087 = ORIENTED_EDGE ( 'NONE', *, *, #3031, .F. ) ;
#46086 = DIRECTION ( 'NONE',  ( 0.000000000000000000, -1.000000000000000000, 0.000000000000000000 ) ) ;
#46088 = DIRECTION ( 'NONE',  ( 0.000000000000000000, 0.000000000000000000, -1.000000000000000000 ) ) ;
#46089 = ORIENTED_EDGE ( 'NONE', *, *, #20566, .T. ) ;
#46090 = VERTEX_POINT ( 'NONE', #63806 ) ;
#46091 = CARTESIAN_POINT ( 'NONE',  ( 4.931982383686722926, -5.876774720514410077, 19.38944687450761961 ) ) ;
#46092 = CARTESIAN_POINT ( 'NONE',  ( -76.52287095715007581, -24.51387760970724372, 9.387446482453411178 ) ) ;
#46093 = CARTESIAN_POINT ( 'NONE',  ( -15.43752342082821905, -15.63289427301443801, 11.49999999999999645 ) ) ;
#46094 = CARTESIAN_POINT ( 'NONE',  ( -89.52215892217839155, -23.48786465467241413, 11.44779295918254292 ) ) ;
#46095 = CARTESIAN_POINT ( 'NONE',  ( -0.2110286175373513040, -22.56517410205234597, 11.49999999999998934 ) ) ;
#46096 = CARTESIAN_POINT ( 'NONE',  ( -18.84683179826791743, -9.195131953753229226, 11.49999999999998934 ) ) ;
#46097 = CARTESIAN_POINT ( 'NONE',  ( -111.5895376238167245, -24.64898659630368627, 1.056161002820391825 ) ) ;
#46098 = PLANE ( 'NONE',  #13509 ) ;
#46099 = ORIENTED_EDGE ( 'NONE', *, *, #65268, .T. ) ;
#46100 = EDGE_LOOP ( 'NONE', ( #33858, #37054, #17748, #92361 ) ) ;
#46101 = ORIENTED_EDGE ( 'NONE', *, *, #50633, .T. ) ;
#46102 = CARTESIAN_POINT ( 'NONE',  ( -88.52287095715000476, -23.95044443724992078, 10.65354141964648704 ) ) ;
#46103 = AXIS2_PLACEMENT_3D ( 'NONE', #95325, #33418, #70492 ) ;
#46104 = CARTESIAN_POINT ( 'NONE',  ( 20.96596170256846747, -4.772324250704091497, -1.500000000000002220 ) ) ;
#46105 = CARTESIAN_POINT ( 'NONE',  ( 1.305682803664691249, 0.3587747205144265483, 29.57950906855421991 ) ) ;
#46106 = ORIENTED_EDGE ( 'NONE', *, *, #38567, .T. ) ;
#46107 = CARTESIAN_POINT ( 'NONE',  ( 9.660767377612277329, -18.76748907076374095, -1.500000000000002220 ) ) ;
#46108 = PLANE ( 'NONE',  #83823 ) ;
#46109 = ADVANCED_FACE ( 'NONE', ( #49067 ), #7059, .T. ) ;
#46110 = FACE_OUTER_BOUND ( 'NONE', #35711, .T. ) ;
#46111 = CARTESIAN_POINT ( 'NONE',  ( -50.12585357699241939, -25.30188792181875357, 4.702141515391761395 ) ) ;
#46112 = DIRECTION ( 'NONE',  ( -1.000000000000000000, -0.000000000000000000, -0.000000000000000000 ) ) ;
#46113 = CARTESIAN_POINT ( 'NONE',  ( -15.87499999999997868, 0.000000000000000000, 2.349999999999999645 ) ) ;
#46114 = CARTESIAN_POINT ( 'NONE',  ( 17.13038851031509680, -14.05419017248541813, -1.500000000000002220 ) ) ;
#46115 = EDGE_CURVE ( 'NONE', #89719, #74381, #83266, .T. ) ;
#46116 = CARTESIAN_POINT ( 'NONE',  ( -111.5228709571500190, -23.48783264082477018, -1.443836473390084585 ) ) ;
#46117 = VECTOR ( 'NONE', #37061, 1000.000000000000114 ) ;
#46118 = ADVANCED_FACE ( 'NONE', ( #4880 ), #26715, .F. ) ;
#46119 = ORIENTED_EDGE ( 'NONE', *, *, #79834, .F. ) ;
#46120 = CARTESIAN_POINT ( 'NONE',  ( -51.44679290749079570, -25.31633139922050191, 5.195306718205446650 ) ) ;
#46121 = CARTESIAN_POINT ( 'NONE',  ( -64.55620429048339304, -23.47593901973091235, -1.443836447539007972 ) ) ;
#46122 = DIRECTION ( 'NONE',  ( 0.000000000000000000, 0.000000000000000000, -1.000000000000000000 ) ) ;
#46123 = ADVANCED_FACE ( 'NONE', ( #4387 ), #51560, .F. ) ;
#46124 = CARTESIAN_POINT ( 'NONE',  ( -100.5450588623535282, -24.92564183028979130, 1.928384488918251760 ) ) ;
#46125 = CARTESIAN_POINT ( 'NONE',  ( 18.22972481837485859, -6.773019484731225504, -1.500000000000002220 ) ) ;
#46126 = CARTESIAN_POINT ( 'NONE',  ( 12.64048258313813733, 17.25876517447949610, 11.49999999999998934 ) ) ;
#46127 = CARTESIAN_POINT ( 'NONE',  ( -62.54858697878290741, -24.15543982623907482, -0.2315651400026649265 ) ) ;
#46128 = CARTESIAN_POINT ( 'NONE',  ( -17.66201745896767505, 6.376774720514425177, -23.06272557202527906 ) ) ;
#46129 = CARTESIAN_POINT ( 'NONE',  ( 28.87399897812680649, -4.772774720514425972, -12.57761096169975623 ) ) ;
#46130 = CARTESIAN_POINT ( 'NONE',  ( -37.22287095715007155, -23.47593901973090524, -1.443836447538998424 ) ) ;
#46131 = CARTESIAN_POINT ( 'NONE',  ( -11.11902432501355342, 19.77583997595719367, -1.500000000000002220 ) ) ;
#46132 = EDGE_CURVE ( 'NONE', #100315, #1307, #51059, .T. ) ;
#46133 = CARTESIAN_POINT ( 'NONE',  ( -98.59636335847339694, -23.73766607897669445, -1.055555164236453569 ) ) ;
#46134 = CARTESIAN_POINT ( 'NONE',  ( 1.876957540558651605, -5.558144974487054135, 0.000000000000000000 ) ) ;
#46135 = CARTESIAN_POINT ( 'NONE',  ( 10.99584971316270732, 16.45119811332560289, 11.49999999999999645 ) ) ;
#46136 = CARTESIAN_POINT ( 'NONE',  ( -101.6228709571500559, -24.66019654487199730, 8.947790411086121054 ) ) ;
#46137 = B_SPLINE_CURVE_WITH_KNOTS ( 'NONE', 3,
 ( #65332, #41979, #49586, #39959, #72424, #2917 ),
 .UNSPECIFIED., .F., .F.,
 ( 4, 2, 4 ),
 ( 0.000000000000000000, 0.001380901958385396351, 0.002761803916770792702 ),
 .UNSPECIFIED. ) ;
#46138 = ORIENTED_EDGE ( 'NONE', *, *, #96965, .T. ) ;
#46139 = DIRECTION ( 'NONE',  ( 1.000000000000000000, 0.000000000000000000, 4.335561085774420994E-16 ) ) ;
#46140 = CARTESIAN_POINT ( 'NONE',  ( -53.62287095715007013, -24.33927499327854704, 9.819080762295818943 ) ) ;
#46141 = CARTESIAN_POINT ( 'NONE',  ( -75.52287095715004739, -25.00182538069145366, 7.747789668545101094 ) ) ;
#46142 = CARTESIAN_POINT ( 'NONE',  ( 16.85579979752674618, 13.57973486276658903, 11.49999999999998934 ) ) ;
#46143 = DIRECTION ( 'NONE',  ( -0.000000000000000000, 1.000000000000000000, -0.000000000000000000 ) ) ;
#46144 = CARTESIAN_POINT ( 'NONE',  ( 12.26431755764203047, -15.03328313062362298, -1.500000000000002220 ) ) ;
#46145 = CARTESIAN_POINT ( 'NONE',  ( -129.6228709571500417, -24.66019654487200086, 8.947790411086117501 ) ) ;
#46146 = DIRECTION ( 'NONE',  ( -3.773278334444166432E-23, 1.000000000000000000, 0.000000000000000000 ) ) ;
#46147 = CARTESIAN_POINT ( 'NONE',  ( -15.05033210666397103, 12.90603908704162173, 11.49999999999998934 ) ) ;
#46148 = ORIENTED_EDGE ( 'NONE', *, *, #69702, .T. ) ;
#46149 = VECTOR ( 'NONE', #85425, 1000.000000000000000 ) ;
#46150 = CARTESIAN_POINT ( 'NONE',  ( 0.8761431260907562857, 20.31601184897261092, 11.49999999999999645 ) ) ;
#46151 = CARTESIAN_POINT ( 'NONE',  ( -80.49978053820711921, -24.63355581998386157, 0.9682620441943954326 ) ) ;
#46152 = CARTESIAN_POINT ( 'NONE',  ( 33.57588617459661151, -3.431642488465076912, -12.05779067269562255 ) ) ;
#46153 = ORIENTED_EDGE ( 'NONE', *, *, #69511, .F. ) ;
#46154 = B_SPLINE_SURFACE_WITH_KNOTS ( 'NONE', 3, 3, ( 
 ( #97729, #14479, #82991, #67801 ),
 ( #68284, #4890, #29218, #35835 ),
 ( #60186, #13980, #91111, #45456 ),
 ( #68780, #83996, #52063, #21587 ),
 ( #44956, #90616, #76370, #53068 ),
 ( #51568, #28724, #6873, #12494 ),
 ( #27726, #67294, #58674, #82009 ) ),
 .UNSPECIFIED., .F., .F., .F.,
 ( 4, 3, 4 ),
 ( 4, 4 ),
 ( 0.0004766839783816705913, 0.1029713700210893035, 0.2054660560637969480 ),
 ( 0.7296796152761164667, 0.7310290126659014787 ),
 .UNSPECIFIED. ) ;
#46155 = CARTESIAN_POINT ( 'NONE',  ( -102.5194635214501062, -23.73791477778911840, 11.05961554403170410 ) ) ;
#46156 = DIRECTION ( 'NONE',  ( 1.000000000000000000, 3.773278334444167608E-23, 8.201307833595939069E-29 ) ) ;
#46157 = CARTESIAN_POINT ( 'NONE',  ( 3.787259615384621636, -6.376774720514404748, 18.51923076923076650 ) ) ;
#46158 = CARTESIAN_POINT ( 'NONE',  ( -69.62287095715005592, -29.50247984919015209, -1.443849546365055359 ) ) ;
#46159 = CARTESIAN_POINT ( 'NONE',  ( -0.7067007548136460260, -6.376774720514410077, 19.51517878119693350 ) ) ;
#46160 = CARTESIAN_POINT ( 'NONE',  ( -19.96166555454951208, -2.086822695551191043, -1.500000000000002220 ) ) ;
#46161 = CARTESIAN_POINT ( 'NONE',  ( -91.62287095715004170, -29.50250243563736774, 8.947779886222139822 ) ) ;
#46162 = ORIENTED_EDGE ( 'NONE', *, *, #16822, .T. ) ;
#46163 = CARTESIAN_POINT ( 'NONE',  ( -91.62287095715005592, -24.51387760970725083, 9.387446482453411178 ) ) ;
#46164 = CARTESIAN_POINT ( 'NONE',  ( -20.40978113611479827, 10.34812579263477872, 11.49999999999999645 ) ) ;
#46165 = CARTESIAN_POINT ( 'NONE',  ( -20.99730734726578874, -8.693733401623333634, 11.49999999999998934 ) ) ;
#46166 = ORIENTED_EDGE ( 'NONE', *, *, #88846, .F. ) ;
#46167 = CARTESIAN_POINT ( 'NONE',  ( -31.58953762381672092, -23.47596703998600276, 11.44779298504227505 ) ) ;
#46168 = CARTESIAN_POINT ( 'NONE',  ( -89.40841769935767047, -25.26877885127129986, 5.947789088311301597 ) ) ;
#46169 = CARTESIAN_POINT ( 'NONE',  ( -38.65670220571585247, -23.73791477778911485, 11.05961554403170766 ) ) ;
#46170 = LINE ( 'NONE', #92329, #18919 ) ;
#46171 = ADVANCED_FACE ( 'NONE', ( #89613 ), #43938, .T. ) ;
#46172 = CARTESIAN_POINT ( 'NONE',  ( -128.6238584146351798, -24.15620529776629510, 10.23563542870659404 ) ) ;
#46173 = CARTESIAN_POINT ( 'NONE',  ( -96.62287095715005592, -29.50250243563736774, 8.947779886222138046 ) ) ;
#46174 = VERTEX_POINT ( 'NONE', #65311 ) ;
#46175 = CARTESIAN_POINT ( 'NONE',  ( 18.17922461840205983, -9.147185827878928421, 11.49999999999998934 ) ) ;
#46176 = ORIENTED_EDGE ( 'NONE', *, *, #63480, .F. ) ;
#46177 = CARTESIAN_POINT ( 'NONE',  ( -16.88208375265294237, -15.58181570610299715, -1.500000000000002220 ) ) ;
#46178 = CARTESIAN_POINT ( 'NONE',  ( -54.48736948649989387, -24.66019654487199375, 8.947790411086119278 ) ) ;
#46179 = VECTOR ( 'NONE', #95258, 1000.000000000000114 ) ;
#46180 = VERTEX_POINT ( 'NONE', #43451 ) ;
#46181 = CARTESIAN_POINT ( 'NONE',  ( -108.5890470795098821, -24.35071581493544102, 9.817618358456016381 ) ) ;
#46182 = CARTESIAN_POINT ( 'NONE',  ( -116.5228709571500474, -24.35013146730204525, 9.818937971375097717 ) ) ;
#46183 = CARTESIAN_POINT ( 'NONE',  ( -51.63915185263472551, -24.15620529776628089, 10.23563542870660470 ) ) ;
#46185 = EDGE_LOOP ( 'NONE', ( #98203, #44178, #87651, #65839 ) ) ;
#46184 = CARTESIAN_POINT ( 'NONE',  ( 12.23393567461250697, 17.36540613969008007, 11.49999999999999645 ) ) ;
#46186 = ORIENTED_EDGE ( 'NONE', *, *, #14652, .F. ) ;
#46187 = CARTESIAN_POINT ( 'NONE',  ( -0.8134642310582372859, 22.17477653155656725, -1.500000000000002220 ) ) ;
#46188 = CARTESIAN_POINT ( 'NONE',  ( -19.88974639711211623, -5.441847772814488948, -1.500000000000002220 ) ) ;
#46189 = ORIENTED_EDGE ( 'NONE', *, *, #95468, .T. ) ;
#46190 = VERTEX_POINT ( 'NONE', #11984 ) ;
#46191 = CARTESIAN_POINT ( 'NONE',  ( -108.9610644980590450, -25.27682616226043777, 4.357072330648456671 ) ) ;
#46192 = CARTESIAN_POINT ( 'NONE',  ( 3.797776442307698286, -5.876774720514427841, 21.83974358974358410 ) ) ;
#46193 = ORIENTED_EDGE ( 'NONE', *, *, #31712, .F. ) ;
#46194 = CARTESIAN_POINT ( 'NONE',  ( -54.52287095715006870, -24.64965694238575011, 8.947790433994203596 ) ) ;
#46195 = ORIENTED_EDGE ( 'NONE', *, *, #34820, .F. ) ;
#46196 = CARTESIAN_POINT ( 'NONE',  ( 30.57287095715025416, 6.119174785681471995, 25.41160796525320720 ) ) ;
#46197 = CARTESIAN_POINT ( 'NONE',  ( -55.62287095715004170, -29.50248789122583659, 2.256150453626215580 ) ) ;
#46198 = CARTESIAN_POINT ( 'NONE',  ( 20.50115541507891948, 3.495740877612329101, -1.500000000000002220 ) ) ;
#46199 = CARTESIAN_POINT ( 'NONE',  ( -9.430186865587145917, -19.61854929170128869, 11.49999999999999645 ) ) ;
#46200 = CARTESIAN_POINT ( 'NONE',  ( -52.62287095715005592, -24.64898659630367561, 1.056161002820821038 ) ) ;
#46201 = CARTESIAN_POINT ( 'NONE',  ( -37.62287095715006302, -24.65952944569304250, 1.056160979905693020 ) ) ;
#46202 = CARTESIAN_POINT ( 'NONE',  ( -15.54266751046811557, -16.22994250641250957, 11.49999999999998934 ) ) ;
#46203 = CARTESIAN_POINT ( 'NONE',  ( -118.5200150627393327, -23.96169478059713853, 10.65365249895717348 ) ) ;
#46204 = EDGE_CURVE ( 'NONE', #98622, #82569, #36271, .T. ) ;
#46205 = ORIENTED_EDGE ( 'NONE', *, *, #95726, .F. ) ;
#46206 = FACE_OUTER_BOUND ( 'NONE', #37201, .T. ) ;
#46207 = CARTESIAN_POINT ( 'NONE',  ( 10.45000000000000462, 1.999999999999998668, 24.00000000000000000 ) ) ;
#46208 = B_SPLINE_CURVE_WITH_KNOTS ( 'NONE', 3,
 ( #76427, #52120, #69331, #100251 ),
 .UNSPECIFIED., .F., .F.,
 ( 4, 4 ),
 ( 0.1588721122365702731, 0.1598728592773357438 ),
 .UNSPECIFIED. ) ;
#46209 = TOROIDAL_SURFACE ( 'NONE', #2478, 80.18232118519038920, 8.160000000000000142 ) ;
#46210 = EDGE_LOOP ( 'NONE', ( #93953, #31168, #16135, #36463 ) ) ;
#46211 = ORIENTED_EDGE ( 'NONE', *, *, #4097, .T. ) ;
#46212 = ORIENTED_EDGE ( 'NONE', *, *, #18829, .T. ) ;
#46213 = CARTESIAN_POINT ( 'NONE',  ( 21.34331307443176584, 0.5271963136488534429, -1.500000000000002220 ) ) ;
#46214 = ORIENTED_EDGE ( 'NONE', *, *, #62720, .F. ) ;
#46215 = CARTESIAN_POINT ( 'NONE',  ( -17.93810645791062441, 10.97360191750010827, 11.49999999999998934 ) ) ;
#46216 = CARTESIAN_POINT ( 'NONE',  ( -30.55801050092156501, -24.27400083755124172, 0.04395666736089842014 ) ) ;
#46217 = EDGE_CURVE ( 'NONE', #73116, #36098, #5478, .T. ) ;
#46218 = CARTESIAN_POINT ( 'NONE',  ( -55.55620429048340725, -23.47593901973091235, -1.443836447539007972 ) ) ;
#46219 = CARTESIAN_POINT ( 'NONE',  ( -79.11611000704996854, -25.18035200424451858, 3.255061677420811428 ) ) ;
#46220 = CARTESIAN_POINT ( 'NONE',  ( 7.969717912702302343, -20.46423023992739942, -1.500000000000002220 ) ) ;
#46221 = CARTESIAN_POINT ( 'NONE',  ( -87.52287095715006160, -24.64898659630528854, 1.056161002820827921 ) ) ;
#46222 = EDGE_LOOP ( 'NONE', ( #48767, #98058, #26971, #82405 ) ) ;
#46223 = CARTESIAN_POINT ( 'NONE',  ( -25.92875734969025814, 3.316774720514426456, 23.50402280011861933 ) ) ;
#46224 = EDGE_CURVE ( 'NONE', #15357, #100201, #52052, .T. ) ;
#46225 = DIRECTION ( 'NONE',  ( 0.9921023176230513441, 0.000000000000000000, -0.1254312216594016538 ) ) ;
#46226 = EDGE_CURVE ( 'NONE', #88353, #79519, #98204, .T. ) ;
#46227 = CARTESIAN_POINT ( 'NONE',  ( 29.68632914399157130, -6.069062472358077720, 27.51067976151145800 ) ) ;
#46228 = EDGE_CURVE ( 'NONE', #14843, #23202, #82000, .T. ) ;
#46229 = DIRECTION ( 'NONE',  ( -0.1254312216594016538, -0.000000000000000000, -0.9921023176230513441 ) ) ;
#46230 = CARTESIAN_POINT ( 'NONE',  ( -0.1255922731526209202, -21.42410932854645722, 10.97511746239722008 ) ) ;
#46231 = CARTESIAN_POINT ( 'NONE',  ( 0.1273799443098547757, 21.28700333820561497, -1.500000000000002220 ) ) ;
#46232 = FACE_OUTER_BOUND ( 'NONE', #41358, .T. ) ;
#46233 = EDGE_CURVE ( 'NONE', #96245, #79255, #34097, .T. ) ;
#46234 = CARTESIAN_POINT ( 'NONE',  ( -52.52287095715006870, -23.47596703998600631, 11.44779298504229104 ) ) ;
#46235 = CIRCLE ( 'NONE', #72180, 251.4258649670780699 ) ;
#46236 = DIRECTION ( 'NONE',  ( 0.7863974287222138537, 0.000000000000000000, 0.6177208787948571533 ) ) ;
#46237 = CARTESIAN_POINT ( 'NONE',  ( -5.154768636056045850, -5.876774720514414518, 19.48351902941045921 ) ) ;
#46238 = CARTESIAN_POINT ( 'NONE',  ( -11.58057713800463162, -19.31455136971746001, -1.500000000000002220 ) ) ;
#46239 = CARTESIAN_POINT ( 'NONE',  ( -111.9729598272094933, -25.06174035403189038, 7.474877196992074424 ) ) ;
#46240 = ORIENTED_EDGE ( 'NONE', *, *, #29050, .T. ) ;
#46242 = CARTESIAN_POINT ( 'NONE',  ( -80.16808653570907950, -25.29573032799826393, 4.512754483485445611 ) ) ;
#46241 = B_SPLINE_CURVE_WITH_KNOTS ( 'NONE', 3,
 ( #36157, #60005, #82814, #66134, #13297, #11813 ),
 .UNSPECIFIED., .F., .F.,
 ( 4, 2, 4 ),
 ( 0.000000000000000000, 0.001380901958385387894, 0.002761803916770775788 ),
 .UNSPECIFIED. ) ;
#46243 = CARTESIAN_POINT ( 'NONE',  ( -16.92291128558595048, 9.936001969431544012, 11.49999999999999645 ) ) ;
#46244 = DIRECTION ( 'NONE',  ( -0.000000000000000000, 1.000000000000000000, -0.000000000000000000 ) ) ;
#46245 = CARTESIAN_POINT ( 'NONE',  ( -76.55620429048339304, -24.64965694238574656, 8.947790433994201820 ) ) ;
#46246 = EDGE_CURVE ( 'NONE', #28213, #33008, #27220, .T. ) ;
#46247 = ORIENTED_EDGE ( 'NONE', *, *, #84335, .F. ) ;
#46248 = B_SPLINE_CURVE_WITH_KNOTS ( 'NONE', 3,
 ( #2715, #80830, #71722, #17424, #26546, #87943, #79816, #10313 ),
 .UNSPECIFIED., .F., .F.,
 ( 4, 2, 2, 4 ),
 ( 0.000000000000000000, 0.0005804693158675770098, 0.0008707039738013634548, 0.001160938631735150117 ),
 .UNSPECIFIED. ) ;
#46249 = AXIS2_PLACEMENT_3D ( 'NONE', #18624, #28241, #11514 ) ;
#46250 = CARTESIAN_POINT ( 'NONE',  ( -88.50297303682343397, -24.66019654487199730, 8.947790411086115725 ) ) ;
#46251 = DIRECTION ( 'NONE',  ( -3.773278334453079618E-23, 0.9999999999976377785, 2.173523156925978705E-06 ) ) ;
#46252 = CARTESIAN_POINT ( 'NONE',  ( -91.96401365818223894, -25.31476272485208412, 5.144091107239472827 ) ) ;
#46253 = CIRCLE ( 'NONE', #28358, 19.30000000000000071 ) ;
#46254 = CARTESIAN_POINT ( 'NONE',  ( -14.27994306655487300, -13.59162091658854798, 11.49999999999998934 ) ) ;
#46255 = ORIENTED_EDGE ( 'NONE', *, *, #78526, .F. ) ;
#46256 = CARTESIAN_POINT ( 'NONE',  ( -109.3584176993576591, -25.28950181196791647, 4.206202504803813191 ) ) ;
#46257 = DIRECTION ( 'NONE',  ( -3.773278334453079618E-23, 0.9999999999976377785, 2.173523156925979975E-06 ) ) ;
#46258 = COORDINATED_UNIVERSAL_TIME_OFFSET ( 0, 0, .AHEAD. ) ;
#46259 = VERTEX_POINT ( 'NONE', #57676 ) ;
#46260 = CARTESIAN_POINT ( 'NONE',  ( -109.6228709571501128, -24.35013146730204525, 9.818937971375104823 ) ) ;
#46261 = CARTESIAN_POINT ( 'NONE',  ( -76.62287095715007013, -24.65952944569304606, 1.056160979905700126 ) ) ;
#46262 = DIRECTION ( 'NONE',  ( 0.000000000000000000, 0.000000000000000000, 1.000000000000000000 ) ) ;
#46263 = DIRECTION ( 'NONE',  ( -3.773278334453079618E-23, 0.9999999999976377785, 2.173523156925979975E-06 ) ) ;
#46264 = DIRECTION ( 'NONE',  ( -0.000000000000000000, 1.000000000000000000, -0.000000000000000000 ) ) ;
#46265 = CARTESIAN_POINT ( 'NONE',  ( 10.34999999999999432, 12.00000000000002309, 2.100000000000000089 ) ) ;
#46266 = CARTESIAN_POINT ( 'NONE',  ( -61.52287095715005449, -24.34917612406837151, 0.1852690917426518535 ) ) ;
#46267 = CARTESIAN_POINT ( 'NONE',  ( 16.79232260237064978, 10.84791536263152523, -1.500000000000002220 ) ) ;
#46268 = ADVANCED_FACE ( 'NONE', ( #42459 ), #88619, .T. ) ;
#46269 = CARTESIAN_POINT ( 'NONE',  ( -95.62287095715002749, -25.00182538069145721, 7.747789668545097541 ) ) ;
#46270 = CARTESIAN_POINT ( 'NONE',  ( -45.58527553150454992, -24.63419186844611986, 9.035850630976927533 ) ) ;
#46271 = VERTEX_POINT ( 'NONE', #41955 ) ;
#46272 = EDGE_CURVE ( 'NONE', #95555, #32256, #93386, .T. ) ;
#46273 = CARTESIAN_POINT ( 'NONE',  ( -119.5886919143434000, -24.51314013834316086, 0.6176544820404245018 ) ) ;
#46274 = VECTOR ( 'NONE', #83338, 1000.000000000000114 ) ;
#46275 = CARTESIAN_POINT ( 'NONE',  ( -73.52287095715007581, -23.47596703998600631, 11.44779298504228748 ) ) ;
#46276 = CARTESIAN_POINT ( 'NONE',  ( 22.02124265030973760, -4.543225279485573864, 15.05402280011862004 ) ) ;
#46277 = CARTESIAN_POINT ( 'NONE',  ( -100.5228709571500616, -25.00182538069145366, 7.747789668545101982 ) ) ;
#46278 = PLANE ( 'NONE',  #43201 ) ;
#46279 = CARTESIAN_POINT ( 'NONE',  ( -83.52214258138457126, -23.48783264082477018, -1.443836473390093689 ) ) ;
#46280 = CARTESIAN_POINT ( 'NONE',  ( -3.004714864173751998, -5.876774720514412742, 19.63296556618507083 ) ) ;
#46281 = EDGE_CURVE ( 'NONE', #96695, #73668, #49932, .T. ) ;
#46282 = CARTESIAN_POINT ( 'NONE',  ( 5.464387484610083057, -5.876774720514419847, 21.31215092858952431 ) ) ;
#46283 = ORIENTED_EDGE ( 'NONE', *, *, #87644, .F. ) ;
#46284 = CARTESIAN_POINT ( 'NONE',  ( -20.27173212042777806, -0.06527795377243154895, -1.500000000000002220 ) ) ;
#46285 = CARTESIAN_POINT ( 'NONE',  ( -122.5551211338554083, -24.15543982623907482, -0.2315651400026565998 ) ) ;
#46286 = EDGE_CURVE ( 'NONE', #32487, #45617, #96253, .T. ) ;
#46287 = FACE_OUTER_BOUND ( 'NONE', #55438, .T. ) ;
#46288 = CARTESIAN_POINT ( 'NONE',  ( -90.52287095715006160, -24.99132157543165889, 2.256160258750667502 ) ) ;
#46289 = ORIENTED_EDGE ( 'NONE', *, *, #70749, .F. ) ;
#46290 = DIRECTION ( 'NONE',  ( 0.1087265912856348327, -0.000000000000000000, 0.9940716917543757081 ) ) ;
#46291 = CARTESIAN_POINT ( 'NONE',  ( 19.96388892861992659, -2.714421270036905032, -1.500000000000002220 ) ) ;
#46292 = CARTESIAN_POINT ( 'NONE',  ( -20.88184962559319402, -2.832954952542597660, 11.49999999999999645 ) ) ;
#46293 = CARTESIAN_POINT ( 'NONE',  ( -13.28819421967561532, -17.68372732473523001, 11.49999999999998934 ) ) ;
#46295 = CARTESIAN_POINT ( 'NONE',  ( 17.96566822227200433, 9.963707542159163211, 11.49999999999998934 ) ) ;
#46294 = PRODUCT_RELATED_PRODUCT_CATEGORY ( 'detail', '', ( #20704 ) ) ;
#46296 = CARTESIAN_POINT ( 'NONE',  ( -95.52214755303867832, -23.48783264082477729, -1.443836473390088804 ) ) ;
#46297 = AXIS2_PLACEMENT_3D ( 'NONE', #53174, #53674, #75980 ) ;
#46298 = CARTESIAN_POINT ( 'NONE',  ( -53.62287095715004881, -23.48783264082478084, -1.443836473390070596 ) ) ;
#46299 = ORIENTED_EDGE ( 'NONE', *, *, #27244, .F. ) ;
#46300 = DIRECTION ( 'NONE',  ( -1.250865172912931245E-15, 6.879758451021121945E-15, -1.000000000000000000 ) ) ;
#46301 = ORIENTED_EDGE ( 'NONE', *, *, #83075, .F. ) ;
#46302 = CARTESIAN_POINT ( 'NONE',  ( -64.52287095715006160, -29.50248528299804818, 1.056150453629034924 ) ) ;
#46303 = CARTESIAN_POINT ( 'NONE',  ( -85.62287095715002749, -25.00182538069145011, 7.747789668545099317 ) ) ;
#46304 = ORIENTED_EDGE ( 'NONE', *, *, #3463, .F. ) ;
#46305 = AXIS2_PLACEMENT_3D ( 'NONE', #57340, #87259, #34482 ) ;
#46306 = ORIENTED_EDGE ( 'NONE', *, *, #12289, .F. ) ;
#46307 = AXIS2_PLACEMENT_3D ( 'NONE', #66012, #57892, #58875 ) ;
#46308 = VERTEX_POINT ( 'NONE', #22075 ) ;
#46309 = CARTESIAN_POINT ( 'NONE',  ( -36.62287095715005592, -29.50250243563736774, 8.947779886222148704 ) ) ;
#46310 = CARTESIAN_POINT ( 'NONE',  ( -50.40895856474225667, -25.03284467579915784, 7.563174216508125269 ) ) ;
#46311 = CARTESIAN_POINT ( 'NONE',  ( -77.55620429048339304, -24.65952944569304606, 1.056160979905698794 ) ) ;
#46312 = CARTESIAN_POINT ( 'NONE',  ( 18.87225196054570020, 8.368929400942139551, -1.500000000000002220 ) ) ;
#46313 = AXIS2_PLACEMENT_3D ( 'NONE', #30887, #78041, #62350 ) ;
#46314 = CARTESIAN_POINT ( 'NONE',  ( -17.57154585214776077, 12.61476001598989782, 11.49999999999999645 ) ) ;
#46315 = ORIENTED_EDGE ( 'NONE', *, *, #92901, .F. ) ;
#46316 = CARTESIAN_POINT ( 'NONE',  ( -100.6228709571500701, -23.47596703998600631, 11.44779298504227860 ) ) ;
#46317 = CARTESIAN_POINT ( 'NONE',  ( 3.252808283508203058, -5.876774720514402972, 18.30939203766361345 ) ) ;
#46318 = CARTESIAN_POINT ( 'NONE',  ( -3.695635658436464244, 22.08213133993951161, -1.500000000000002220 ) ) ;
#46319 = CIRCLE ( 'NONE', #13938, 129.7684398600581233 ) ;
#46320 = CARTESIAN_POINT ( 'NONE',  ( -79.85862890617264043, -25.12205772052471886, 6.918725823854117607 ) ) ;
#46321 = CARTESIAN_POINT ( 'NONE',  ( -53.52287095715008292, -23.47593901973090169, -1.443836447538997092 ) ) ;
#46322 = ORIENTED_EDGE ( 'NONE', *, *, #43272, .T. ) ;
#46323 = CARTESIAN_POINT ( 'NONE',  ( -58.52287095715006160, -24.65952944569304250, 1.056160979905695463 ) ) ;
#46324 = CARTESIAN_POINT ( 'NONE',  ( -29.49875734969026198, 5.965225279485572685, 2.362022800118626531 ) ) ;
#46325 = DIRECTION ( 'NONE',  ( -3.773278334453079030E-23, 0.9999999999976377785, 2.173523156925979128E-06 ) ) ;
#46326 = CARTESIAN_POINT ( 'NONE',  ( -20.36979505965413395, -4.774807507659313721, 11.49999999999998934 ) ) ;
#46327 = ORIENTED_EDGE ( 'NONE', *, *, #14947, .T. ) ;
#46328 = CARTESIAN_POINT ( 'NONE',  ( -67.54434724194248929, -24.35071581493543746, 9.817618358456023486 ) ) ;
#46329 = ORIENTED_EDGE ( 'NONE', *, *, #81386, .F. ) ;
#46330 = CARTESIAN_POINT ( 'NONE',  ( -109.5552926830755069, -23.96169478059713498, 10.65365249895717703 ) ) ;
#46331 = CARTESIAN_POINT ( 'NONE',  ( 14.81885032312887240, -15.09863332352077592, -1.500000000000002220 ) ) ;
#46332 = ORIENTED_EDGE ( 'NONE', *, *, #84822, .T. ) ;
#46333 = CARTESIAN_POINT ( 'NONE',  ( -50.62119766888658035, -23.48783264082476308, -1.443836473390096797 ) ) ;
#46334 = PLANE ( 'NONE',  #32002 ) ;
#46335 = CARTESIAN_POINT ( 'NONE',  ( 6.392671032147439369, 20.83241601264130693, -1.500000000000002220 ) ) ;
#46336 = FACE_OUTER_BOUND ( 'NONE', #78137, .T. ) ;
#46337 = CARTESIAN_POINT ( 'NONE',  ( -81.52287095715006160, -24.64898659630367916, 1.056161002820826145 ) ) ;
#46338 = CARTESIAN_POINT ( 'NONE',  ( 7.460332110455646593, -6.376774720514418959, 20.55293369838740247 ) ) ;
#46339 = CARTESIAN_POINT ( 'NONE',  ( -20.57666286913221754, 7.287794730890116313, -1.500000000000002220 ) ) ;
#46340 = CARTESIAN_POINT ( 'NONE',  ( -41.62287095715006302, -24.64898659630367561, 1.056161002820819261 ) ) ;
#46341 = EDGE_CURVE ( 'NONE', #94971, #37998, #37818, .T. ) ;
#46342 = ORIENTED_EDGE ( 'NONE', *, *, #75431, .F. ) ;
#46343 = CARTESIAN_POINT ( 'NONE',  ( 7.402957069319889172, -5.876774720514418959, 20.34212842306459024 ) ) ;
#46344 = CARTESIAN_POINT ( 'NONE',  ( -69.92287095715006728, -23.47596703998600631, 11.44779298504227860 ) ) ;
#46345 = CARTESIAN_POINT ( 'NONE',  ( -43.62287095715005592, -23.72747288104442021, -1.053458166803663998 ) ) ;
#46346 = ORIENTED_EDGE ( 'NONE', *, *, #18442, .T. ) ;
#46347 = EDGE_LOOP ( 'NONE', ( #26932, #63302, #12975, #39708 ) ) ;
#46348 = VERTEX_POINT ( 'NONE', #60178 ) ;
#46349 = EDGE_CURVE ( 'NONE', #87941, #71994, #3832, .T. ) ;
#46350 = LINE ( 'NONE', #52976, #20559 ) ;
#46351 = CARTESIAN_POINT ( 'NONE',  ( -1.563627757057377110, -21.15500258984412696, -1.500000000000002220 ) ) ;
#46352 = CARTESIAN_POINT ( 'NONE',  ( -94.63645698038313014, -23.73766607897670866, -1.055555164236451349 ) ) ;
#46353 = EDGE_CURVE ( 'NONE', #86043, #94109, #81359, .T. ) ;
#46354 = CARTESIAN_POINT ( 'NONE',  ( -80.08103705783366877, -25.03138289048727216, 7.514832880348969013 ) ) ;
#46355 = DIRECTION ( 'NONE',  ( 0.000000000000000000, 0.000000000000000000, 1.000000000000000000 ) ) ;
#46356 = CARTESIAN_POINT ( 'NONE',  ( -89.40841769935767047, -29.50248914370730091, 2.832395270851967073 ) ) ;
#46357 = CARTESIAN_POINT ( 'NONE',  ( 17.72857150710123619, 7.855407458714720903, -1.500000000000002220 ) ) ;
#46358 = FACE_OUTER_BOUND ( 'NONE', #4642, .T. ) ;
#46359 = VERTEX_POINT ( 'NONE', #76852 ) ;
#46360 = CARTESIAN_POINT ( 'NONE',  ( -16.97169330436246781, 9.548981535075045102, 11.49999999999999645 ) ) ;
#46361 = DIRECTION ( 'NONE',  ( -1.224646799147353207E-16, 1.000000000000000000, 0.000000000000000000 ) ) ;
#46362 = PLANE ( 'NONE',  #72260 ) ;
#46363 = EDGE_CURVE ( 'NONE', #31435, #98063, #93031, .T. ) ;
#46364 = ORIENTED_EDGE ( 'NONE', *, *, #31456, .F. ) ;
#46365 = CARTESIAN_POINT ( 'NONE',  ( -93.62287095715005592, -23.47593901973091235, -1.443836447539002865 ) ) ;
#46366 = PLANE ( 'NONE',  #83642 ) ;
#46367 = AXIS2_PLACEMENT_3D ( 'NONE', #26684, #34298, #71360 ) ;
#46368 = DIRECTION ( 'NONE',  ( -3.773278334444166432E-23, 1.000000000000000000, 0.000000000000000000 ) ) ;
#46369 = CARTESIAN_POINT ( 'NONE',  ( -93.54915263021753447, -24.35071581493543746, 9.817618358456018157 ) ) ;
#46370 = CARTESIAN_POINT ( 'NONE',  ( -11.98250242409135780, 15.54504917500377559, -1.500000000000002220 ) ) ;
#46371 = DIRECTION ( 'NONE',  ( -0.000000000000000000, 1.000000000000000000, -0.000000000000000000 ) ) ;
#46372 = EDGE_LOOP ( 'NONE', ( #78867, #79940, #43434, #80382 ) ) ;
#46373 = CARTESIAN_POINT ( 'NONE',  ( -4.019545577234938882, 21.20919285897865336, -1.500000000000002220 ) ) ;
#46374 = DIRECTION ( 'NONE',  ( 0.000000000000000000, -1.000000000000000000, 0.000000000000000000 ) ) ;
#46375 = CARTESIAN_POINT ( 'NONE',  ( 0.4325450954222598288, 0.000000000000000000, 0.000000000000000000 ) ) ;
#46376 = CARTESIAN_POINT ( 'NONE',  ( 1.000208336950358934, 0.000000000000000000, 2.349999999999999645 ) ) ;
#46377 = CARTESIAN_POINT ( 'NONE',  ( 16.10802587768190008, -16.50329280669357246, -1.500000000000002220 ) ) ;
#46378 = AXIS2_PLACEMENT_3D ( 'NONE', #73011, #88232, #18696 ) ;
#46379 = SHAPE_DEFINITION_REPRESENTATION ( #36109, #60715 ) ;
#46380 = CARTESIAN_POINT ( 'NONE',  ( -129.6228709571500417, -29.50250786944525672, 11.44777988621622633 ) ) ;
#46381 = FACE_OUTER_BOUND ( 'NONE', #34593, .T. ) ;
#46382 = CARTESIAN_POINT ( 'NONE',  ( -121.5894494653266662, -24.35071581493543391, 9.817618358456025263 ) ) ;
#46383 = CARTESIAN_POINT ( 'NONE',  ( -104.5228709571501042, -23.72773821059536914, 11.05748984161097326 ) ) ;
#46384 = AXIS2_PLACEMENT_3D ( 'NONE', #78874, #85498, #15979 ) ;
#46386 = CARTESIAN_POINT ( 'NONE',  ( -109.4090396635228188, -25.25571914749011881, 3.901050301940306664 ) ) ;
#46385 = VECTOR ( 'NONE', #90265, 1000.000000000000000 ) ;
#46387 = CARTESIAN_POINT ( 'NONE',  ( -129.5896348228089323, -24.51314013834316796, 0.6176544820404222813 ) ) ;
#46388 = CARTESIAN_POINT ( 'NONE',  ( -114.5882167185886260, -24.51419770103159124, 9.386484678747160970 ) ) ;
#46389 = CARTESIAN_POINT ( 'NONE',  ( 3.219775368129482285, -19.64489633315863770, -1.500000000000002220 ) ) ;
#46390 = CIRCLE ( 'NONE', #73929, 129.7684398600581517 ) ;
#46391 = CARTESIAN_POINT ( 'NONE',  ( -41.58953762381673158, -23.48783264082477729, -1.443836473390071928 ) ) ;
#46392 = CARTESIAN_POINT ( 'NONE',  ( 18.55763160240848109, 7.024834138330111166, -1.500000000000002220 ) ) ;
#46393 = VECTOR ( 'NONE', #26582, 1000.000000000000114 ) ;
#46394 = CARTESIAN_POINT ( 'NONE',  ( -56.53342923132996845, -24.65952944569304250, 1.056160979905696795 ) ) ;
#46395 = ADVANCED_FACE ( 'NONE', ( #13971 ), #61176, .T. ) ;
#46396 = CARTESIAN_POINT ( 'NONE',  ( -39.04530173637052570, -25.10925879726424625, 4.154357150429498269 ) ) ;
#46397 = DIRECTION ( 'NONE',  ( -0.000000000000000000, 2.173523156925979552E-06, -0.9999999999976378895 ) ) ;
#46398 = CARTESIAN_POINT ( 'NONE',  ( -16.63904852704994042, -12.34428335884295969, 11.49999999999999645 ) ) ;
#46399 = LINE ( 'NONE', #16944, #58081 ) ;
#46400 = CARTESIAN_POINT ( 'NONE',  ( -50.05581273115511465, -25.31439285659850214, 5.236521717157118339 ) ) ;
#46402 = ADVANCED_FACE ( 'NONE', ( #29705 ), #6371, .F. ) ;
#46401 = CARTESIAN_POINT ( 'NONE',  ( -20.46125754976198508, 9.905080999540670561, 11.49999999999999645 ) ) ;
#46403 = ORIENTED_EDGE ( 'NONE', *, *, #43736, .T. ) ;
#46404 = DIRECTION ( 'NONE',  ( 1.000000000000000000, 3.773278334444166432E-23, 8.201307841325785021E-29 ) ) ;
#46405 = DIRECTION ( 'NONE',  ( 0.9913618264504691080, 7.885106708985488048E-16, -0.1311553622875927805 ) ) ;
#46406 = ORIENTED_EDGE ( 'NONE', *, *, #47764, .F. ) ;
#46407 = CARTESIAN_POINT ( 'NONE',  ( 19.60372117168125072, 4.849774137724135237, -1.500000000000002220 ) ) ;
#46408 = PLANE ( 'NONE',  #9520 ) ;
#46409 = CARTESIAN_POINT ( 'NONE',  ( -57.62287095715004881, -29.50250786944525672, 11.44777988621623876 ) ) ;
#46410 = VECTOR ( 'NONE', #68304, 1000.000000000000114 ) ;
#46411 = ORIENTED_EDGE ( 'NONE', *, *, #49791, .F. ) ;
#46412 = ORIENTED_EDGE ( 'NONE', *, *, #33541, .T. ) ;
#46413 = CARTESIAN_POINT ( 'NONE',  ( -80.35919894935767616, -29.50249278017872712, 4.505472193924938473 ) ) ;
#46414 = CARTESIAN_POINT ( 'NONE',  ( -2.380104427745746154, 22.76713797270899065, -1.500000000000002220 ) ) ;
#46415 = CARTESIAN_POINT ( 'NONE',  ( -29.52491602809394422, -24.57633962600280597, 1.056161296257513094 ) ) ;
#46416 = CARTESIAN_POINT ( 'NONE',  ( -5.517532219241116032, 20.92096086382833064, -1.500000000000002220 ) ) ;
#46417 = CARTESIAN_POINT ( 'NONE',  ( -29.49875734969025842, -0.3587747205144262708, 23.37402280011862743 ) ) ;
#46418 = CARTESIAN_POINT ( 'NONE',  ( -114.6228709571500133, -24.33832256527049154, 0.1851278514138625098 ) ) ;
#46419 = CARTESIAN_POINT ( 'NONE',  ( -17.98194200498208062, 10.70670730041394947, 11.49999999999999645 ) ) ;
#46420 = ORIENTED_EDGE ( 'NONE', *, *, #85156, .F. ) ;
#46421 = CARTESIAN_POINT ( 'NONE',  ( -69.32616065491644974, -25.24754329150182741, 5.234946919193567361 ) ) ;
#46422 = CARTESIAN_POINT ( 'NONE',  ( -16.14483305390557888, 14.99321182834783528, 11.49999999999998934 ) ) ;
#46423 = EDGE_CURVE ( 'NONE', #97857, #47577, #53559, .T. ) ;
#46424 = FACE_OUTER_BOUND ( 'NONE', #77846, .T. ) ;
#46425 = CARTESIAN_POINT ( 'NONE',  ( -66.52287095715006160, -24.64965694238407323, 8.947790433994200043 ) ) ;
#46426 = ORIENTED_EDGE ( 'NONE', *, *, #97352, .F. ) ;
#46427 = CARTESIAN_POINT ( 'NONE',  ( -72.62287095715005592, -29.50250243563736774, 8.947779886222143375 ) ) ;
#46428 = CARTESIAN_POINT ( 'NONE',  ( -9.278253834636469577, -6.376774720514426953, 21.48128695274316158 ) ) ;
#46429 = ORIENTED_EDGE ( 'NONE', *, *, #57111, .T. ) ;
#46430 = CARTESIAN_POINT ( 'NONE',  ( -72.54527135507231606, -24.35071581493542681, 9.817618358456032368 ) ) ;
#46431 = B_SPLINE_CURVE_WITH_KNOTS ( 'NONE', 3,
 ( #99403, #98397, #52742, #83681 ),
 .UNSPECIFIED., .F., .F.,
 ( 4, 4 ),
 ( 2.775557561562891351E-17, 9.999999999996123101E-05 ),
 .UNSPECIFIED. ) ;
#46432 = VERTEX_POINT ( 'NONE', #75370 ) ;
#46433 = ORIENTED_EDGE ( 'NONE', *, *, #39416, .F. ) ;
#46434 = CARTESIAN_POINT ( 'NONE',  ( -71.64477584057199522, -23.73791477778911840, 11.05961554403170766 ) ) ;
#46435 = CARTESIAN_POINT ( 'NONE',  ( -95.62287095715005592, -24.83620972994591725, 8.398175272781362111 ) ) ;
#46436 = CARTESIAN_POINT ( 'NONE',  ( -4.533825836049095059, -5.876774720514411854, 19.59623724171353132 ) ) ;
#46437 = CARTESIAN_POINT ( 'NONE',  ( -13.28352777634190396, 15.58691228024164310, -1.500000000000002220 ) ) ;
#46438 = VERTEX_POINT ( 'NONE', #37331 ) ;
#46439 = DIRECTION ( 'NONE',  ( 0.000000000000000000, 2.173523156925980399E-06, -0.9999999999976378895 ) ) ;
#46440 = EDGE_CURVE ( 'NONE', #14898, #24603, #5868, .T. ) ;
#46441 = CARTESIAN_POINT ( 'NONE',  ( -10.35374248095108030, 5.304213687372781649, 27.98611676734227771 ) ) ;
#46442 = CYLINDRICAL_SURFACE ( 'NONE', #12629, 3.549999999999999378 ) ;
#46443 = CARTESIAN_POINT ( 'NONE',  ( -22.27612280437926273, 0.2766752662994830247, -1.500000000000002220 ) ) ;
#46444 = ADVANCED_FACE ( 'NONE', ( #41319 ), #1758, .T. ) ;
#46445 = VECTOR ( 'NONE', #81942, 1000.000000000000000 ) ;
#46446 = CARTESIAN_POINT ( 'NONE',  ( -10.34999999999999254, 1.999999999999999112, 2.499999999999999112 ) ) ;
#46447 = FACE_OUTER_BOUND ( 'NONE', #37445, .T. ) ;
#46448 = EDGE_LOOP ( 'NONE', ( #48733, #66559, #77875, #99716 ) ) ;
#46449 = CARTESIAN_POINT ( 'NONE',  ( -73.52287095715007581, -29.50250243563736774, 8.947779886222143375 ) ) ;
#46450 = CARTESIAN_POINT ( 'NONE',  ( -28.54076794517382965, -24.63646022460865836, 8.057462240486939820 ) ) ;
#46451 = CARTESIAN_POINT ( 'NONE',  ( -15.88994834598175387, -13.44966708658631838, 11.49999999999998934 ) ) ;
#46452 = ORIENTED_EDGE ( 'NONE', *, *, #55274, .T. ) ;
#46454 = VERTEX_POINT ( 'NONE', #2266 ) ;
#46453 = CARTESIAN_POINT ( 'NONE',  ( -29.49875734969026198, -0.3587747205144262708, 0.1180228001186258285 ) ) ;
#46455 = VECTOR ( 'NONE', #48800, 1000.000000000000000 ) ;
#46456 = CARTESIAN_POINT ( 'NONE',  ( -50.99155954085787812, -25.25854544672502655, 6.987757701561226220 ) ) ;
#46457 = ORIENTED_EDGE ( 'NONE', *, *, #17013, .T. ) ;
#46458 = CIRCLE ( 'NONE', #83746, 1.325999999999969647 ) ;
#46459 = CARTESIAN_POINT ( 'NONE',  ( 31.13709916799238897, -5.945958180706680807, -1.190136329645604230 ) ) ;
#46460 = CARTESIAN_POINT ( 'NONE',  ( -55.62287095715004170, -24.91570333823098693, 8.075032458375554612 ) ) ;
#46461 = CARTESIAN_POINT ( 'NONE',  ( 9.214646252612421762, -3.316774720514544583, -27.04520690475792222 ) ) ;
#46462 = VECTOR ( 'NONE', #81038, 1000.000000000000114 ) ;
#46463 = CARTESIAN_POINT ( 'NONE',  ( -51.55620429048339304, -24.65952944569304606, 1.056160979905694131 ) ) ;
#46464 = CARTESIAN_POINT ( 'NONE',  ( -92.56173786369195966, -23.48786465467241413, 11.44779295918254469 ) ) ;
#46465 = CARTESIAN_POINT ( 'NONE',  ( 25.61870917940689196, -0.3587747205144265483, 29.49402280011862487 ) ) ;
#46466 = EDGE_CURVE ( 'NONE', #17101, #21, #84942, .T. ) ;
#46468 = EDGE_LOOP ( 'NONE', ( #53040, #29381, #92358, #29712 ) ) ;
#46467 = CARTESIAN_POINT ( 'NONE',  ( -10.71655374829924767, -19.46388382022006525, 11.49999999999999645 ) ) ;
#46469 = CARTESIAN_POINT ( 'NONE',  ( -38.62287095715005592, -23.48783264082477373, -1.443836473390072594 ) ) ;
#46470 = ORIENTED_EDGE ( 'NONE', *, *, #60948, .T. ) ;
#46471 = CARTESIAN_POINT ( 'NONE',  ( 13.37577147909557773, 18.27418014603220442, 11.49999999999998934 ) ) ;
#46472 = AXIS2_PLACEMENT_3D ( 'NONE', #15068, #44026, #36912 ) ;
#46474 = ORIENTED_EDGE ( 'NONE', *, *, #31267, .T. ) ;
#46473 = DIRECTION ( 'NONE',  ( 1.000000000000000000, 0.000000000000000000, 0.000000000000000000 ) ) ;
#46475 = VERTEX_POINT ( 'NONE', #86980 ) ;
#46476 = DIRECTION ( 'NONE',  ( 0.000000000000000000, -0.000000000000000000, 1.000000000000000000 ) ) ;
#46477 = EDGE_CURVE ( 'NONE', #98350, #97460, #2767, .T. ) ;
#46478 = CARTESIAN_POINT ( 'NONE',  ( -20.09103079077430820, 1.113595961413322177, -1.500000000000002220 ) ) ;
#46479 = ADVANCED_FACE ( 'NONE', ( #64684 ), #94091, .F. ) ;
#46480 = DIRECTION ( 'NONE',  ( -3.504491870660219321E-16, 1.000000000000000000, 0.000000000000000000 ) ) ;
#46481 = EDGE_LOOP ( 'NONE', ( #98136, #93764, #56821, #52452 ) ) ;
#46482 = CARTESIAN_POINT ( 'NONE',  ( -42.62287095715004881, -24.66019654487199020, 8.947790411086135265 ) ) ;
#46483 = CARTESIAN_POINT ( 'NONE',  ( -6.430504157862594994, -21.42354456762059201, -1.500000000000002220 ) ) ;
#46484 = EDGE_CURVE ( 'NONE', #20042, #9985, #33198, .T. ) ;
#46485 = VERTEX_POINT ( 'NONE', #56054 ) ;
#46486 = EDGE_LOOP ( 'NONE', ( #73747, #68763, #86366, #94116 ) ) ;
#46487 = CARTESIAN_POINT ( 'NONE',  ( -101.4810573493621177, -25.25341147194796676, 6.435288862326006054 ) ) ;
#46488 = CARTESIAN_POINT ( 'NONE',  ( -119.6228709571500559, -23.95044443724992433, 10.65354141964649592 ) ) ;
#46489 = DIRECTION ( 'NONE',  ( 1.000000000000000000, 3.773278334444166432E-23, 8.201307841325785021E-29 ) ) ;
#46490 = VECTOR ( 'NONE', #50570, 1000.000000000000114 ) ;
#46491 = FACE_OUTER_BOUND ( 'NONE', #93206, .T. ) ;
#46492 = EDGE_CURVE ( 'NONE', #42771, #404, #78359, .T. ) ;
#46493 = CARTESIAN_POINT ( 'NONE',  ( -11.16000000000000014, -10.15233964170348457, 0.003711184059992174607 ) ) ;
#46494 = CARTESIAN_POINT ( 'NONE',  ( 6.866622826037362515, -18.30913693658520103, -1.500000000000002220 ) ) ;
#46495 = CARTESIAN_POINT ( 'NONE',  ( -111.6228709571500559, -29.50250243563736774, 8.947779886222136270 ) ) ;
#46496 = CARTESIAN_POINT ( 'NONE',  ( 21.22668844964908885, 3.412186807495566132, 11.49999999999998934 ) ) ;
#46497 = CIRCLE ( 'NONE', #82136, 1.249999999999997558 ) ;
#46498 = CARTESIAN_POINT ( 'NONE',  ( -128.5220661547153043, -23.73766607897671932, -1.055555164236423149 ) ) ;
#46499 = CARTESIAN_POINT ( 'NONE',  ( 29.73860345376319358, 4.772803916115708311, -4.021109907510727943 ) ) ;
#46500 = CARTESIAN_POINT ( 'NONE',  ( -71.52287095715007581, -23.48786465467241058, 11.44779295918254647 ) ) ;
#46501 = CARTESIAN_POINT ( 'NONE',  ( -107.6228709571500701, -23.47596703998600631, 11.44779298504227860 ) ) ;
#46502 = CARTESIAN_POINT ( 'NONE',  ( 12.51456667378993259, 19.11410217522374921, -1.500000000000002220 ) ) ;
#46503 = PERSON_AND_ORGANIZATION ( #70597, #27821 ) ;
#46504 = CARTESIAN_POINT ( 'NONE',  ( -85.62287095715005592, -23.48786465467241413, 11.44779295918254114 ) ) ;
#46505 = FACE_OUTER_BOUND ( 'NONE', #54269, .T. ) ;
#46506 = CARTESIAN_POINT ( 'NONE',  ( 20.03642891561555928, 0.6179553080306146029, 11.49999999999999645 ) ) ;
#46507 = CARTESIAN_POINT ( 'NONE',  ( -79.52287095715004739, -23.48783264082476663, -1.443836473390090358 ) ) ;
#46508 = DIRECTION ( 'NONE',  ( 0.000000000000000000, 1.000000000000000000, 0.000000000000000000 ) ) ;
#46509 = CARTESIAN_POINT ( 'NONE',  ( -15.54901181048698255, 6.376774720514426953, -55.62515100798455592 ) ) ;
#46510 = CARTESIAN_POINT ( 'NONE',  ( 2.899999999999999023, 33.29999999999999716, 2.100000000000000089 ) ) ;
#46511 = ORIENTED_EDGE ( 'NONE', *, *, #58263, .T. ) ;
#46512 = CYLINDRICAL_SURFACE ( 'NONE', #29976, 1.699999999999996625 ) ;
#46513 = CARTESIAN_POINT ( 'NONE',  ( -109.2319509041356582, -25.19177197432999904, 3.341196461261103590 ) ) ;
#46514 = CARTESIAN_POINT ( 'NONE',  ( -15.31764660673900558, 15.41647822393392175, -1.500000000000002220 ) ) ;
#46515 = LINE ( 'NONE', #69857, #91695 ) ;
#46516 = CARTESIAN_POINT ( 'NONE',  ( 18.62133539762988121, 6.091496293051981148, -1.500000000000002220 ) ) ;
#46517 = VECTOR ( 'NONE', #28267, 1000.000000000000114 ) ;
#46518 = CARTESIAN_POINT ( 'NONE',  ( -85.52287095715003318, -25.00182538069145011, 7.747789668545101094 ) ) ;
#46519 = ADVANCED_FACE ( 'NONE', ( #86484 ), #78856, .T. ) ;
#46520 = CARTESIAN_POINT ( 'NONE',  ( -109.9698394925872549, -25.31698189487863715, 5.331473593049757653 ) ) ;
#46521 = ITEM_DEFINED_TRANSFORMATION ( 'NONE', 'NONE', #95834,  #37391 ) ;
#46522 = CARTESIAN_POINT ( 'NONE',  ( -91.62578307729398830, -24.51419770103159124, 9.386484678747176957 ) ) ;
#46523 = CARTESIAN_POINT ( 'NONE',  ( 2.832419239133125544, -5.876774720514422512, 21.23415460623727213 ) ) ;
#46524 = CARTESIAN_POINT ( 'NONE',  ( 4.502618398017903090, 20.03723546437915104, 11.49999999999999645 ) ) ;
#46525 = LINE ( 'NONE', #45535, #84591 ) ;
#46526 = CIRCLE ( 'NONE', #12479, 2.500000000000000444 ) ;
#46527 = CARTESIAN_POINT ( 'NONE',  ( -120.5539087145323833, -24.52300882791530512, 0.6510814631126412566 ) ) ;
#46528 = ORIENTED_EDGE ( 'NONE', *, *, #23633, .F. ) ;
#46529 =( LENGTH_UNIT ( ) NAMED_UNIT ( * ) SI_UNIT ( .MILLI., .METRE. ) );
#46530 = CARTESIAN_POINT ( 'NONE',  ( -100.6814946224345846, -25.31296450754352279, 4.736250530731430430 ) ) ;
#46531 = CARTESIAN_POINT ( 'NONE',  ( -39.81688933929658702, -25.28892465615578544, 3.494185961199250290 ) ) ;
#46532 = CIRCLE ( 'NONE', #2799, 1.149999999999998135 ) ;
#46533 = CARTESIAN_POINT ( 'NONE',  ( 20.57455539870835182, -3.407774720514426647, -18.22080502500614330 ) ) ;
#46534 = FACE_BOUND ( 'NONE', #27339, .T. ) ;
#46535 = VECTOR ( 'NONE', #24752, 1000.000000000000000 ) ;
#46536 = B_SPLINE_CURVE_WITH_KNOTS ( 'NONE', 3,
 ( #43282, #74221, #100019, #22895, #76199, #23399, #85826, #47272, #78197, #61996 ),
 .UNSPECIFIED., .F., .F.,
 ( 4, 2, 2, 2, 4 ),
 ( -1.423960876792978737E-05, 0.0005136504108877040049, 0.001041540430543337831, 0.001569430450198971549, 0.002097320469854605483 ),
 .UNSPECIFIED. ) ;
#46537 = LINE ( 'NONE', #56162, #62993 ) ;
#46538 = CARTESIAN_POINT ( 'NONE',  ( -124.6228709571501128, -23.96177878511308634, 10.65340807706329507 ) ) ;
#46539 = CARTESIAN_POINT ( 'NONE',  ( 18.33865528945960577, 14.04639130150205872, 11.49999999999999645 ) ) ;
#46540 = CARTESIAN_POINT ( 'NONE',  ( -18.69919181139871966, -13.08804974640095686, 11.49999999999998934 ) ) ;
#46541 = CARTESIAN_POINT ( 'NONE',  ( 4.653846153846159517, -5.876774720514419847, 19.99999999999999289 ) ) ;
#46542 = CARTESIAN_POINT ( 'NONE',  ( -75.52287095715013265, -24.14406661686762945, 10.28769366194083901 ) ) ;
#46543 = CARTESIAN_POINT ( 'NONE',  ( -123.5228709571501042, -23.48783264082477018, -1.443836473390084141 ) ) ;
#46544 = CARTESIAN_POINT ( 'NONE',  ( -21.67104271438225638, 5.786422744429515319, 11.49999999999999645 ) ) ;
#46545 = ORIENTED_EDGE ( 'NONE', *, *, #25605, .T. ) ;
#46546 = CARTESIAN_POINT ( 'NONE',  ( -106.5562042904834215, -24.64898659630529210, 1.056161002820828587 ) ) ;
#46547 = DIRECTION ( 'NONE',  ( 0.000000000000000000, -2.173523156925979552E-06, 0.9999999999976378895 ) ) ;
#46548 = CARTESIAN_POINT ( 'NONE',  ( -19.33260374144687077, -10.33727041909969380, 11.49999999999998934 ) ) ;
#46549 = B_SPLINE_CURVE_WITH_KNOTS ( 'NONE', 3,
 ( #2940, #10531, #95770, #26261 ),
 .UNSPECIFIED., .F., .F.,
 ( 4, 4 ),
 ( 0.000000000000000000, 1.000000000000000000 ),
 .UNSPECIFIED. ) ;
#46550 = CARTESIAN_POINT ( 'NONE',  ( -19.80875734969026425, 5.965225279485572685, 31.02402280011862246 ) ) ;
#46551 = EDGE_CURVE ( 'NONE', #70905, #57983, #16969, .T. ) ;
#46552 = CARTESIAN_POINT ( 'NONE',  ( -72.52287095715007581, -29.50248528299804818, 1.056150453629036701 ) ) ;
#46553 = DIRECTION ( 'NONE',  ( 0.1478094111296165691, -0.9890158633619158257, 0.000000000000000000 ) ) ;
#46554 = CARTESIAN_POINT ( 'NONE',  ( -49.02504946315652035, -25.17378427848792910, 6.789324151856864553 ) ) ;
#46555 = DIRECTION ( 'NONE',  ( 0.000000000000000000, 1.000000000000000000, 0.000000000000000000 ) ) ;
#46556 = ORIENTED_EDGE ( 'NONE', *, *, #533, .T. ) ;
#46557 = CARTESIAN_POINT ( 'NONE',  ( 10.21088607376515789, 17.76353854702842483, -1.500000000000002220 ) ) ;
#46558 = ORIENTED_EDGE ( 'NONE', *, *, #9579, .F. ) ;
#46559 = ORIENTED_EDGE ( 'NONE', *, *, #70799, .T. ) ;
#46560 = ORIENTED_EDGE ( 'NONE', *, *, #11723, .T. ) ;
#46561 = ORIENTED_EDGE ( 'NONE', *, *, #13538, .F. ) ;
#46562 = CARTESIAN_POINT ( 'NONE',  ( -14.75821945985506645, 17.75411527500383002, -1.500000000000002220 ) ) ;
#46563 = CARTESIAN_POINT ( 'NONE',  ( -82.52287095715006160, -23.94994826722564696, -0.6494450866342720285 ) ) ;
#46564 = CARTESIAN_POINT ( 'NONE',  ( 0.7435384974594729801, 20.27106041150680937, -1.500000000000002220 ) ) ;
#46565 = VERTEX_POINT ( 'NONE', #64180 ) ;
#46566 = ADVANCED_FACE ( 'NONE', ( #95101 ), #41734, .T. ) ;
#46567 = VECTOR ( 'NONE', #44854, 999.9999999999998863 ) ;
#46568 = CARTESIAN_POINT ( 'NONE',  ( -48.52287095715006870, -23.72773821059535848, 11.05748984161097326 ) ) ;
#46569 = ADVANCED_FACE ( 'NONE', ( #59045 ), #26087, .T. ) ;
#46570 = CARTESIAN_POINT ( 'NONE',  ( -92.56173453440464982, -23.48783264082477729, -1.443836473390063713 ) ) ;
#46571 = EDGE_CURVE ( 'NONE', #75883, #87540, #35705, .T. ) ;
#46572 = DIRECTION ( 'NONE',  ( 0.000000000000000000, -0.9999999999976377785, -2.173523156925979975E-06 ) ) ;
#46573 = CARTESIAN_POINT ( 'NONE',  ( -70.58187943343651227, -24.83618233451450052, 1.606449574219541487 ) ) ;
#46575 = ORIENTED_EDGE ( 'NONE', *, *, #6946, .T. ) ;
#46574 = CARTESIAN_POINT ( 'NONE',  ( 8.645823604709390153, 19.67543227842514852, 11.49999999999999645 ) ) ;
#46576 = CARTESIAN_POINT ( 'NONE',  ( -2.499999999999986677, 22.00000000000000000, 2.100000000000000089 ) ) ;
#46577 = CARTESIAN_POINT ( 'NONE',  ( 14.97946386127326157, 3.496757005395687123, -28.37921330198105352 ) ) ;
#46578 = ADVANCED_FACE ( 'NONE', ( #73272 ), #16842, .F. ) ;
#46579 = ORIENTED_EDGE ( 'NONE', *, *, #84311, .F. ) ;
#46580 = VECTOR ( 'NONE', #8809, 1000.000000000000114 ) ;
#46581 = CARTESIAN_POINT ( 'NONE',  ( 6.562613027033147084, 19.67253995144353240, -1.500000000000002220 ) ) ;
#46582 = ORIENTED_EDGE ( 'NONE', *, *, #35762, .T. ) ;
#46583 = B_SPLINE_CURVE_WITH_KNOTS ( 'NONE', 3,
 ( #14084, #83094, #52663, #91707, #91215, #68882, #22189, #14587 ),
 .UNSPECIFIED., .F., .F.,
 ( 4, 2, 2, 4 ),
 ( -0.001224873891641433234, -0.0002244903592271136998, 0.0007758931731872054007, 0.002776660238015844252 ),
 .UNSPECIFIED. ) ;
#46585 = VERTEX_POINT ( 'NONE', #88994 ) ;
#46584 = DIRECTION ( 'NONE',  ( 0.000000000000000000, 0.000000000000000000, 1.000000000000000000 ) ) ;
#46586 = B_SPLINE_SURFACE_WITH_KNOTS ( 'NONE', 3, 3, ( 
 ( #98359, #21729, #43099, #29355 ),
 ( #83133, #28864, #74042, #90261 ),
 ( #74534, #52702, #21234, #35486 ),
 ( #83640, #89766, #5025, #37476 ),
 ( #91747, #76021, #68426, #35973 ),
 ( #20737, #52205, #60828, #59318 ),
 ( #99361, #66943, #44091, #67434 ) ),
 .UNSPECIFIED., .F., .F., .F.,
 ( 4, 3, 4 ),
 ( 4, 4 ),
 ( 0.7945040050992241421, 0.8970133687736505657, 0.9995227324480768782 ),
 ( 0.9297302545846050092, 0.9311722043212208311 ),
 .UNSPECIFIED. ) ;
#46587 = CARTESIAN_POINT ( 'NONE',  ( -111.5501932863792973, -24.66019654487200441, 8.947790411086105067 ) ) ;
#46588 = LINE ( 'NONE', #63329, #38901 ) ;
#46589 = VERTEX_POINT ( 'NONE', #3765 ) ;
#46590 = ORIENTED_EDGE ( 'NONE', *, *, #34917, .T. ) ;
#46591 = LINE ( 'NONE', #77515, #16979 ) ;
#46592 = FACE_OUTER_BOUND ( 'NONE', #4142, .T. ) ;
#46593 = CARTESIAN_POINT ( 'NONE',  ( -65.49893136555071749, -24.40034930558991277, 0.3402023900116039612 ) ) ;
#46594 = EDGE_CURVE ( 'NONE', #67442, #40077, #47395, .T. ) ;
#46595 = CARTESIAN_POINT ( 'NONE',  ( -2.093881351098874521, -21.91542971883435698, 11.49999999999999645 ) ) ;
#46596 = CARTESIAN_POINT ( 'NONE',  ( -39.04303308397305727, -25.28006866179717349, 4.215216948383927686 ) ) ;
#46597 = CARTESIAN_POINT ( 'NONE',  ( -5.352388609804938469, -21.92410630658433845, 11.49999999999998934 ) ) ;
#46598 = TOROIDAL_SURFACE ( 'NONE', #93568, 253.2618649670780826, 1.835999999999999854 ) ;
#46599 = CARTESIAN_POINT ( 'NONE',  ( 20.99820426035194032, -0.1900765340283884497, -1.500000000000002220 ) ) ;
#46600 = B_SPLINE_CURVE_WITH_KNOTS ( 'NONE', 3,
 ( #73812, #81434, #11915, #26139, #43379, #82418, #97644, #3819, #20512, #58111 ),
 .UNSPECIFIED., .F., .F.,
 ( 4, 2, 2, 2, 4 ),
 ( 1.734723475976807094E-18, 0.001417051740733931559, 0.002125577611100896037, 0.002479840546284378926, 0.002834103481467860949 ),
 .UNSPECIFIED. ) ;
#46601 = B_SPLINE_CURVE_WITH_KNOTS ( 'NONE', 3,
 ( #702, #31649, #62618, #39759 ),
 .UNSPECIFIED., .F., .F.,
 ( 4, 4 ),
 ( 0.000000000000000000, 1.000000000000000000 ),
 .UNSPECIFIED. ) ;
#46602 = CARTESIAN_POINT ( 'NONE',  ( 8.271845302688321411, -0.3854532800250839442, -3.722136940144805450 ) ) ;
#46604 = EDGE_CURVE ( 'NONE', #66723, #34190, #96593, .T. ) ;
#46603 = ORIENTED_EDGE ( 'NONE', *, *, #12125, .F. ) ;
#46605 = VERTEX_POINT ( 'NONE', #28091 ) ;
#46606 = CARTESIAN_POINT ( 'NONE',  ( -59.62287095715007013, -23.95044443724992433, 10.65354141964650125 ) ) ;
#46607 = ADVANCED_FACE ( 'NONE', ( #12845 ), #89984, .F. ) ;
#46608 = AXIS2_PLACEMENT_3D ( 'NONE', #87989, #78851, #40312 ) ;
#46609 = CARTESIAN_POINT ( 'NONE',  ( -11.62584540149672385, -18.10649092712023389, -1.500000000000002220 ) ) ;
#46610 = CARTESIAN_POINT ( 'NONE',  ( -114.6228709571500559, -23.47593901973091235, -1.443836447538999312 ) ) ;
#46611 = ORIENTED_EDGE ( 'NONE', *, *, #45154, .T. ) ;
#46612 = CARTESIAN_POINT ( 'NONE',  ( 14.81885032312887240, -15.09863332352077592, -1.500000000000002220 ) ) ;
#46613 = CARTESIAN_POINT ( 'NONE',  ( -126.6228709571501128, -23.73907113216991860, -1.053371485793222373 ) ) ;
#46614 = CARTESIAN_POINT ( 'NONE',  ( -60.72593597384194908, -25.31249728293746770, 5.276660823416809087 ) ) ;
#46615 = CARTESIAN_POINT ( 'NONE',  ( -121.5550122312708652, -24.15543982623907127, -0.2315651400026573492 ) ) ;
#46616 = AXIS2_PLACEMENT_3D ( 'NONE', #72091, #10678, #9676 ) ;
#46617 = CARTESIAN_POINT ( 'NONE',  ( -109.6228709571500559, -24.66019654487199730, 8.947790411086124607 ) ) ;
#46618 = CARTESIAN_POINT ( 'NONE',  ( -81.22287095715009286, -23.47593901973090169, -1.443836447538997092 ) ) ;
#46619 = CARTESIAN_POINT ( 'NONE',  ( 7.527104757430762128, -20.84474501729809859, -1.500000000000002220 ) ) ;
#46620 = CARTESIAN_POINT ( 'NONE',  ( -71.49854048978230026, -24.51314013834315730, 0.6176544820404130665 ) ) ;
#46621 = EDGE_CURVE ( 'NONE', #78091, #90318, #70397, .T. ) ;
#46622 = ORIENTED_EDGE ( 'NONE', *, *, #96644, .F. ) ;
#46623 = DIRECTION ( 'NONE',  ( -0.000000000000000000, -1.000000000000000000, -0.000000000000000000 ) ) ;
#46624 = LINE ( 'NONE', #56247, #71926 ) ;
#46625 = CARTESIAN_POINT ( 'NONE',  ( -40.01839366089613748, -25.30501058306510487, 5.509688048021296858 ) ) ;
#46626 = ADVANCED_FACE ( 'NONE', ( #49948 ), #27595, .F. ) ;
#46627 = PLANE ( 'NONE',  #62547 ) ;
#46628 = CARTESIAN_POINT ( 'NONE',  ( -39.55620429048340725, -24.64965694238574656, 8.947790433994205372 ) ) ;
#46629 = ADVANCED_FACE ( 'NONE', ( #65183 ), #72777, .T. ) ;
#46630 = CARTESIAN_POINT ( 'NONE',  ( 13.32768686175602646, -14.16729652289716057, -1.500000000000002220 ) ) ;
#46631 = CARTESIAN_POINT ( 'NONE',  ( 2.027878592902508270, 21.29203748114955985, 11.49999999999998934 ) ) ;
#46632 = CARTESIAN_POINT ( 'NONE',  ( -62.62365711165048054, -24.65952944569303895, 1.056160979905693686 ) ) ;
#46633 = CARTESIAN_POINT ( 'NONE',  ( -94.62287095715005592, -24.65952944569304606, 1.056160979905700348 ) ) ;
#46634 = CARTESIAN_POINT ( 'NONE',  ( -72.52287095715010423, -23.95044443724992789, 10.65354141964649592 ) ) ;
#46635 = CARTESIAN_POINT ( 'NONE',  ( -101.0947412695425385, -25.18440065684229623, 3.544729342112358683 ) ) ;
#46636 = CARTESIAN_POINT ( 'NONE',  ( -6.316168294299441932, 21.79233575779346310, -1.500000000000002220 ) ) ;
#46637 = B_SPLINE_CURVE_WITH_KNOTS ( 'NONE', 3,
 ( #97544, #4206, #36153, #34660, #81328, #97047, #20401, #73224, #26547, #5194, #66130 ),
 .UNSPECIFIED., .F., .F.,
 ( 4, 1, 1, 1, 1, 1, 1, 1, 4 ),
 ( 0.000000000000000000, 0.1105883385953350950, 0.2245417540535963874, 0.3425034940501046066, 0.4643240984173571118, 0.5907560327017662427, 0.7222274753555133486, 0.8588428362087243695, 1.000000000000000000 ),
 .UNSPECIFIED. ) ;
#46638 = CARTESIAN_POINT ( 'NONE',  ( -103.6228709571500275, -24.51283580621364067, 0.6167428607019885822 ) ) ;
#46639 = CARTESIAN_POINT ( 'NONE',  ( 31.63608488009066733, 3.316774720514426456, 27.34773273846990094 ) ) ;
#46640 = CARTESIAN_POINT ( 'NONE',  ( 7.211006999188390942, 18.53272205163514030, 11.49999999999999645 ) ) ;
#46641 = CARTESIAN_POINT ( 'NONE',  ( -123.6243254326775087, -24.35071581493544812, 9.817618358456018157 ) ) ;
#46642 = CARTESIAN_POINT ( 'NONE',  ( -51.52287095715006870, -24.64965694238407323, 8.947790433994203596 ) ) ;
#46643 = VERTEX_POINT ( 'NONE', #26596 ) ;
#46644 = CARTESIAN_POINT ( 'NONE',  ( -119.5228709571500758, -29.50247984919015209, -1.443849546365046699 ) ) ;
#46645 = CARTESIAN_POINT ( 'NONE',  ( -6.100820854657341918, -5.876774720514413630, 19.76359802465961124 ) ) ;
#46646 = CARTESIAN_POINT ( 'NONE',  ( -87.58953762381671027, -23.47596703998600631, 11.44779298504227683 ) ) ;
#46647 = CARTESIAN_POINT ( 'NONE',  ( 21.13687465659472409, 4.681744431724916389, 11.49999999999998934 ) ) ;
#46648 = AXIS2_PLACEMENT_3D ( 'NONE', #20492, #51463, #80907 ) ;
#46649 = CARTESIAN_POINT ( 'NONE',  ( -124.5562042904833646, -24.64898659630529565, 1.056161002820835026 ) ) ;
#46650 = CARTESIAN_POINT ( 'NONE',  ( 13.32768686175602646, -14.16729652289716057, -1.500000000000002220 ) ) ;
#46651 = CARTESIAN_POINT ( 'NONE',  ( -114.5895376238167103, -24.64965694238407679, 8.947790433994649462 ) ) ;
#46652 = CARTESIAN_POINT ( 'NONE',  ( -61.62287095715004881, -23.47596703998600631, 11.44779298504227505 ) ) ;
#46653 = CARTESIAN_POINT ( 'NONE',  ( -11.71124675921804403, 15.99993322257668282, 11.49999999999998934 ) ) ;
#46654 = ORIENTED_EDGE ( 'NONE', *, *, #47939, .F. ) ;
#46655 = CARTESIAN_POINT ( 'NONE',  ( -18.82316870354832616, 7.800066519331792847, 11.49999999999999645 ) ) ;
#46656 = CARTESIAN_POINT ( 'NONE',  ( -80.55274853021465731, -24.15503026093913164, -0.2815557561904567518 ) ) ;
#46657 = CARTESIAN_POINT ( 'NONE',  ( -10.79305683637731406, -5.965225279485594001, -27.49869550653260930 ) ) ;
#46658 = VERTEX_POINT ( 'NONE', #34212 ) ;
#46659 = DIRECTION ( 'NONE',  ( -3.773278334453079618E-23, 0.9999999999976377785, 2.173523156925979975E-06 ) ) ;
#46660 = DIRECTION ( 'NONE',  ( -0.000000000000000000, 0.000000000000000000, -1.000000000000000000 ) ) ;
#46661 = CARTESIAN_POINT ( 'NONE',  ( -49.70686029532972583, -25.25214431742755394, 4.960084010147586930 ) ) ;
#46662 = CARTESIAN_POINT ( 'NONE',  ( -128.6228709571500417, -23.48783264082479505, -1.443836473390056829 ) ) ;
#46663 = CARTESIAN_POINT ( 'NONE',  ( -9.150000000000000355, -5.876774720514426953, -15.69999999999999929 ) ) ;
#46664 = CARTESIAN_POINT ( 'NONE',  ( 5.780499401231428358, -19.25771307485560158, -1.500000000000002220 ) ) ;
#46665 = DIRECTION ( 'NONE',  ( -0.000000000000000000, -0.000000000000000000, -1.000000000000000000 ) ) ;
#46666 = VERTEX_POINT ( 'NONE', #57558 ) ;
#46667 = CARTESIAN_POINT ( 'NONE',  ( -91.62287095715009855, -23.73934037231758154, 11.05740245334328442 ) ) ;
#46668 = VECTOR ( 'NONE', #40397, 1000.000000000000000 ) ;
#46669 = CARTESIAN_POINT ( 'NONE',  ( 15.42672287639063100, 16.92133821996916865, 11.49999999999999645 ) ) ;
#46670 = CARTESIAN_POINT ( 'NONE',  ( -4.086358941109507370, -22.34742993483353146, -1.500000000000002220 ) ) ;
#46671 = ORIENTED_EDGE ( 'NONE', *, *, #90901, .T. ) ;
#46672 = CARTESIAN_POINT ( 'NONE',  ( -23.59123376470063960, 6.143225279485574397, 24.50402280011862288 ) ) ;
#46673 = CARTESIAN_POINT ( 'NONE',  ( -51.52287095715006870, -23.47596703998600631, 11.44779298504229104 ) ) ;
#46674 = CARTESIAN_POINT ( 'NONE',  ( -40.45829750704997707, -25.19502912051678223, 3.293943094755625633 ) ) ;
#46675 = PLANE ( 'NONE',  #78884 ) ;
#46676 = AXIS2_PLACEMENT_3D ( 'NONE', #72788, #25602, #4271 ) ;
#46677 = CARTESIAN_POINT ( 'NONE',  ( -128.6240059821712975, -23.96169478059714919, 10.65365249895716993 ) ) ;
#46678 = CARTESIAN_POINT ( 'NONE',  ( -62.62287095715004881, -29.50248528299804818, 1.056150453629034924 ) ) ;
#46679 = ORIENTED_EDGE ( 'NONE', *, *, #37915, .F. ) ;
#46680 = EDGE_CURVE ( 'NONE', #46766, #59937, #99479, .T. ) ;
#46681 = AXIS2_PLACEMENT_3D ( 'NONE', #4573, #66493, #58363 ) ;
#46682 = CARTESIAN_POINT ( 'NONE',  ( -0.5597704280004801580, 20.37679164443051505, -1.500000000000002220 ) ) ;
#46684 = EDGE_CURVE ( 'NONE', #23928, #69379, #42827, .T. ) ;
#46683 = ORIENTED_EDGE ( 'NONE', *, *, #47945, .F. ) ;
#46685 = CARTESIAN_POINT ( 'NONE',  ( -22.77861398648627400, -3.026084143414268013, -1.500000000000002220 ) ) ;
#46686 = CARTESIAN_POINT ( 'NONE',  ( -45.52287095715006870, -23.84047902841602706, -0.8780736468305712084 ) ) ;
#46687 = ADVANCED_FACE ( 'NONE', ( #35207 ), #82858, .T. ) ;
#46688 = VERTEX_POINT ( 'NONE', #52426 ) ;
#46689 = CARTESIAN_POINT ( 'NONE',  ( -108.5121515958373095, -24.66019654487200086, 8.947790411086106843 ) ) ;
#46690 = EDGE_CURVE ( 'NONE', #45742, #93240, #22442, .T. ) ;
#46692 = EDGE_CURVE ( 'NONE', #25473, #294, #36695, .T. ) ;
#46691 = CARTESIAN_POINT ( 'NONE',  ( 3.004381791450704942, -6.376774720514420736, 20.78526834885430219 ) ) ;
#46693 = CARTESIAN_POINT ( 'NONE',  ( -111.5228709571500758, -24.50321055353805377, 9.387540953477511607 ) ) ;
#46695 = ORIENTED_EDGE ( 'NONE', *, *, #88714, .F. ) ;
#46694 = CARTESIAN_POINT ( 'NONE',  ( 13.79380260783658407, 16.28676726024703214, 11.49999999999999645 ) ) ;
#46696 = ORIENTED_EDGE ( 'NONE', *, *, #17339, .F. ) ;
#46697 = CARTESIAN_POINT ( 'NONE',  ( 13.49617185221842952, 17.62045156095830123, -1.500000000000002220 ) ) ;
#46698 = CARTESIAN_POINT ( 'NONE',  ( 15.34805171112899203, -13.82090413600154299, 11.49999999999998934 ) ) ;
#46699 = ORIENTED_EDGE ( 'NONE', *, *, #65753, .T. ) ;
#46700 = ORIENTED_EDGE ( 'NONE', *, *, #71886, .F. ) ;
#46701 = DIRECTION ( 'NONE',  ( -1.000000000000000000, 0.000000000000000000, -7.994117400814786717E-16 ) ) ;
#46702 = CARTESIAN_POINT ( 'NONE',  ( -70.78956819130432621, -25.31392322340849432, 5.203679841770401104 ) ) ;
#46703 = VERTEX_POINT ( 'NONE', #98075 ) ;
#46704 = CARTESIAN_POINT ( 'NONE',  ( -51.62287095715005592, -23.48786465467241413, 11.44779295918254824 ) ) ;
#46705 = ORIENTED_EDGE ( 'NONE', *, *, #57570, .F. ) ;
#46706 = CARTESIAN_POINT ( 'NONE',  ( -58.51505936317359158, -23.73791477778912196, 11.05961554403170588 ) ) ;
#46707 = CARTESIAN_POINT ( 'NONE',  ( -115.6228709571500559, -23.47596703998600631, 11.44779298504227860 ) ) ;
#46708 = CARTESIAN_POINT ( 'NONE',  ( -16.21995886604411297, 13.06735728859114509, -1.500000000000002220 ) ) ;
#46709 = EDGE_CURVE ( 'NONE', #74103, #94609, #5550, .T. ) ;
#46710 = CARTESIAN_POINT ( 'NONE',  ( -19.00758693998263738, -10.61793046214600089, 11.49999999999999645 ) ) ;
#46711 = DIRECTION ( 'NONE',  ( 1.000000000000000000, 3.773278334444167608E-23, 8.201307833595939069E-29 ) ) ;
#46712 = CARTESIAN_POINT ( 'NONE',  ( -78.49838375731654594, -24.66019654487200441, 8.947790411086119278 ) ) ;
#46713 = CARTESIAN_POINT ( 'NONE',  ( -16.74552829020559130, -14.98668287627115170, 11.49999999999998934 ) ) ;
#46714 = CARTESIAN_POINT ( 'NONE',  ( -38.51306538520876188, -23.73766607897670511, -1.055555164236442689 ) ) ;
#46715 = DIRECTION ( 'NONE',  ( 0.000000000000000000, 0.9999999999976377785, 2.173523156925979128E-06 ) ) ;
#46716 = CARTESIAN_POINT ( 'NONE',  ( 4.967948717948723392, -5.876774720514415407, 20.00140224358974095 ) ) ;
#46717 = EDGE_CURVE ( 'NONE', #80526, #17884, #45315, .T. ) ;
#46718 = B_SPLINE_SURFACE_WITH_KNOTS ( 'NONE', 3, 3, ( 
 ( #36634, #84801, #45749, #46250 ),
 ( #99017, #76670, #60492, #7176 ),
 ( #44757, #83301, #75681, #92410 ),
 ( #98520, #6181, #22388, #38630 ),
 ( #29017, #73, #22881, #53372 ),
 ( #14784, #53869, #29513, #38125 ),
 ( #45255, #90423, #100005, #6679 ) ),
 .UNSPECIFIED., .F., .F., .F.,
 ( 4, 3, 4 ),
 ( 4, 4 ),
 ( 0.7945040050992240310, 0.8970133687736500105, 0.9995227324480759901 ),
 ( 0.4196006235780267435, 0.4208070636251879937 ),
 .UNSPECIFIED. ) ;
#46719 = ORIENTED_EDGE ( 'NONE', *, *, #2377, .F. ) ;
#46720 = ORIENTED_EDGE ( 'NONE', *, *, #98973, .T. ) ;
#46721 = ORIENTED_EDGE ( 'NONE', *, *, #79417, .T. ) ;
#46722 = CARTESIAN_POINT ( 'NONE',  ( -10.68834330497911189, 18.46263264838738039, -1.500000000000002220 ) ) ;
#46723 = ORIENTED_EDGE ( 'NONE', *, *, #28011, .T. ) ;
#46724 = CARTESIAN_POINT ( 'NONE',  ( -10.38599875782317206, -18.32754119035049101, -1.500000000000002220 ) ) ;
#46725 = CARTESIAN_POINT ( 'NONE',  ( -30.54278559372614055, -24.67075338507718385, 1.095666116063849449 ) ) ;
#46726 = CARTESIAN_POINT ( 'NONE',  ( -19.77041435686880533, -2.435487021107205940, -1.500000000000002220 ) ) ;
#46727 = CARTESIAN_POINT ( 'NONE',  ( -99.58403181145372685, -25.24012543510424678, 3.741775170833818276 ) ) ;
#46728 = PLANE ( 'NONE',  #91956 ) ;
#46729 = CARTESIAN_POINT ( 'NONE',  ( -19.44315311050126382, -10.23602577120861667, -1.500000000000002220 ) ) ;
#46730 = CARTESIAN_POINT ( 'NONE',  ( -68.62287095715005592, -23.47596703998600631, 11.44779298504227505 ) ) ;
#46731 = ORIENTED_EDGE ( 'NONE', *, *, #60925, .T. ) ;
#46732 = DIRECTION ( 'NONE',  ( 0.000000000000000000, 2.173523156925980399E-06, -0.9999999999976378895 ) ) ;
#46733 = DIRECTION ( 'NONE',  ( 0.000000000000000000, -2.173523156925979552E-06, 0.9999999999976378895 ) ) ;
#46734 = CARTESIAN_POINT ( 'NONE',  ( -5.376107494350208960, -20.15860285114975525, 11.49999999999999645 ) ) ;
#46735 = CIRCLE ( 'NONE', #59715, 1.699999999999999289 ) ;
#46736 = EDGE_CURVE ( 'NONE', #91432, #95809, #14838, .T. ) ;
#46737 = CARTESIAN_POINT ( 'NONE',  ( 31.65328924465878302, -5.892800044774432422, 28.08003312682333785 ) ) ;
#46738 = PLANE ( 'NONE',  #48987 ) ;
#46739 = FACE_OUTER_BOUND ( 'NONE', #22626, .T. ) ;
#46740 = CARTESIAN_POINT ( 'NONE',  ( 11.00477826368897283, 18.22718707545001138, 11.49999999999998934 ) ) ;
#46741 = CARTESIAN_POINT ( 'NONE',  ( -29.55620429048338949, -24.56885446186112532, 8.947790474426803087 ) ) ;
#46742 = CARTESIAN_POINT ( 'NONE',  ( -107.5890161267547711, -24.35071581493543746, 9.817618358456021710 ) ) ;
#46743 = EDGE_CURVE ( 'NONE', #1643, #25180, #38175, .T. ) ;
#46744 = CARTESIAN_POINT ( 'NONE',  ( -69.86226385320381382, -29.50248914370730091, 2.832395270851967073 ) ) ;
#46745 = CARTESIAN_POINT ( 'NONE',  ( -5.533628790199073499, -5.876774720514418071, 19.87297243748313491 ) ) ;
#46746 = CARTESIAN_POINT ( 'NONE',  ( -1.797493081057526032, -22.44471576765463183, -1.500000000000002220 ) ) ;
#46747 = LINE ( 'NONE', #7168, #84699 ) ;
#46748 = EDGE_LOOP ( 'NONE', ( #76028, #85352, #88396, #28468 ) ) ;
#46749 = CARTESIAN_POINT ( 'NONE',  ( -89.62287095715002749, -23.48783264082478439, -1.443836473390063713 ) ) ;
#46750 = CARTESIAN_POINT ( 'NONE',  ( -9.385407830382300531, 17.29636241635495608, 11.49999999999999645 ) ) ;
#46751 = DIRECTION ( 'NONE',  ( -1.000000000000000000, -3.773278334444166432E-23, -8.201307841325785021E-29 ) ) ;
#46752 = VECTOR ( 'NONE', #81837, 1000.000000000000000 ) ;
#46753 = PLANE ( 'NONE',  #39869 ) ;
#46754 = ORIENTED_EDGE ( 'NONE', *, *, #88374, .F. ) ;
#46755 = CARTESIAN_POINT ( 'NONE',  ( 5.184553252003285984, -6.475225279485573360, -28.06387035751381731 ) ) ;
#46756 = CARTESIAN_POINT ( 'NONE',  ( -36.52287095715006870, -24.64965694238407323, 8.947790433994205372 ) ) ;
#46757 = CARTESIAN_POINT ( 'NONE',  ( -89.90409546361829030, -25.12049752546737835, 2.832404795212227100 ) ) ;
#46758 = CARTESIAN_POINT ( 'NONE',  ( 22.02124265030973760, -6.143225279485574397, 12.85402280011862430 ) ) ;
#46759 = CARTESIAN_POINT ( 'NONE',  ( 15.33752688427012778, 12.42672799324400934, 11.49999999999998934 ) ) ;
#46760 = CIRCLE ( 'NONE', #24069, 2.399999999999999911 ) ;
#46761 = ORIENTED_EDGE ( 'NONE', *, *, #300, .T. ) ;
#46762 = B_SPLINE_CURVE_WITH_KNOTS ( 'NONE', 3,
 ( #8064, #9561, #448, #8570, #48651, #87189, #33395, #71480, #17173, #39518, #63882, #24292, #94293, #64387, #70470, #31403, #94796, #955, #31905 ),
 .UNSPECIFIED., .F., .F.,
 ( 4, 1, 1, 1, 1, 1, 1, 1, 1, 1, 1, 1, 1, 1, 1, 1, 4 ),
 ( 0.000000000000000000, 0.06523080374203017728, 0.1284048960032230235, 0.1900670715964783708, 0.2509433657682806351, 0.3115458328521427123, 0.3728628021568293205, 0.4350236738562381356, 0.4990717247070431406, 0.5630910750496627148, 0.6255101063303755149, 0.6866800359296488798, 0.7472825030135124003, 0.8085634952159584943, 0.8707421035159862432, 0.9343409515059130088, 1.000000000000000000 ),
 .UNSPECIFIED. ) ;
#46763 = FACE_OUTER_BOUND ( 'NONE', #20682, .T. ) ;
#46764 = B_SPLINE_CURVE_WITH_KNOTS ( 'NONE', 3,
 ( #82757, #43709, #74645, #67062 ),
 .UNSPECIFIED., .F., .F.,
 ( 4, 4 ),
 ( 0.03878246734470643803, 0.03978321438547192945 ),
 .UNSPECIFIED. ) ;
#46765 = DATE_AND_TIME ( #37644, #10149 ) ;
#46766 = VERTEX_POINT ( 'NONE', #13844 ) ;
#46767 = FACE_OUTER_BOUND ( 'NONE', #19513, .T. ) ;
#46768 = LINE ( 'NONE', #7187, #36125 ) ;
#46769 = CARTESIAN_POINT ( 'NONE',  ( -55.63765809019586328, -24.52300882791528736, 0.6510814631126286001 ) ) ;
#46770 = CARTESIAN_POINT ( 'NONE',  ( -98.94109201664207376, -25.03144944621345758, 6.485444833557155064 ) ) ;
#46771 = CARTESIAN_POINT ( 'NONE',  ( -85.52287095715006160, -23.48783264082476663, -1.443836473390089470 ) ) ;
#46772 = CARTESIAN_POINT ( 'NONE',  ( -91.94687923781920347, -25.22391124735684187, 6.409327647371628522 ) ) ;
#46773 = CARTESIAN_POINT ( 'NONE',  ( -107.5130078572901766, -24.51314013834316086, 0.6176544820404228364 ) ) ;
#46774 = CARTESIAN_POINT ( 'NONE',  ( 17.55240489776628721, -9.587225365216566431, 11.49999999999998934 ) ) ;
#46775 = DIRECTION ( 'NONE',  ( 6.267148949376394486E-16, 1.000000000000000000, -5.583826031377232793E-16 ) ) ;
#46776 = FACE_OUTER_BOUND ( 'NONE', #82650, .T. ) ;
#46777 = ORIENTED_EDGE ( 'NONE', *, *, #4531, .F. ) ;
#46778 = FACE_OUTER_BOUND ( 'NONE', #19096, .T. ) ;
#46779 = CARTESIAN_POINT ( 'NONE',  ( -109.4679719608024300, -25.29012830856320093, 3.778970069853266445 ) ) ;
#46780 = CARTESIAN_POINT ( 'NONE',  ( -120.6228709571500417, -24.92579138211019796, 1.929029949965668012 ) ) ;
#46781 = CARTESIAN_POINT ( 'NONE',  ( -28.62287095715004881, -24.19626334920329214, 9.819127031579586884 ) ) ;
#46782 = CARTESIAN_POINT ( 'NONE',  ( -38.62287095715005592, -23.48783264082477373, -1.443836473390072594 ) ) ;
#46783 = CARTESIAN_POINT ( 'NONE',  ( -83.54731854358884391, -24.34968618360933590, 0.1864209137778810865 ) ) ;
#46784 = B_SPLINE_SURFACE_WITH_KNOTS ( 'NONE', 3, 3, ( 
 ( #35398, #30825, #23197, #61790 ),
 ( #53676, #14086, #76481, #15589 ),
 ( #6987, #67905, #53176, #98826 ),
 ( #68393, #29820, #52666, #7984 ),
 ( #6491, #99808, #8491, #60791 ),
 ( #37442, #60293, #38933, #84106 ),
 ( #91217, #93214, #22690, #92217 ) ),
 .UNSPECIFIED., .F., .F., .F.,
 ( 4, 3, 4 ),
 ( 4, 4 ),
 ( 0.0004766839783815015100, 0.1029713700210894561, 0.2054660560637974198 ),
 ( 0.5196261812711125971, 0.5208786603924070446 ),
 .UNSPECIFIED. ) ;
#46785 = CARTESIAN_POINT ( 'NONE',  ( -2.959136224476847765, -5.876774720514413630, 19.53857357749110335 ) ) ;
#46786 = CARTESIAN_POINT ( 'NONE',  ( 5.331146515430939203, -5.876774720514419847, 20.91308853528358469 ) ) ;
#46787 = VERTEX_POINT ( 'NONE', #100057 ) ;
#46788 = VECTOR ( 'NONE', #36545, 1000.000000000000000 ) ;
#46789 = EDGE_CURVE ( 'NONE', #48376, #71418, #30572, .T. ) ;
#46790 = VECTOR ( 'NONE', #72776, 1000.000000000000114 ) ;
#46791 = CARTESIAN_POINT ( 'NONE',  ( 16.59675031405745571, -11.69241480613374407, -1.500000000000002220 ) ) ;
#46792 = CARTESIAN_POINT ( 'NONE',  ( -109.6228709571500417, -23.48783264082478794, -1.443836473390060382 ) ) ;
#46793 = EDGE_CURVE ( 'NONE', #86907, #98076, #53427, .T. ) ;
#46794 = VECTOR ( 'NONE', #21103, 1000.000000000000000 ) ;
#46795 = PLANE ( 'NONE',  #57366 ) ;
#46796 = ADVANCED_FACE ( 'NONE', ( #13344 ), #5741, .T. ) ;
#46797 = VERTEX_POINT ( 'NONE', #6237 ) ;
#46798 = CARTESIAN_POINT ( 'NONE',  ( -86.52287095715006160, -23.48786465467241058, 11.44779295918254292 ) ) ;
#46799 = CARTESIAN_POINT ( 'NONE',  ( 16.71511084712224360, -11.16500066668146829, -1.500000000000002220 ) ) ;
#46800 = EDGE_CURVE ( 'NONE', #26363, #54720, #83860, .T. ) ;
#46801 = CARTESIAN_POINT ( 'NONE',  ( 18.35617536642501690, 10.39506492455470088, 11.49999999999999645 ) ) ;
#46802 = VECTOR ( 'NONE', #4486, 1000.000000000000000 ) ;
#46803 = CARTESIAN_POINT ( 'NONE',  ( -8.904070064990065703, -20.24664451029508783, -1.500000000000002220 ) ) ;
#46804 = ADVANCED_FACE ( 'NONE', ( #37194 ), #7227, .F. ) ;
#46805 = CARTESIAN_POINT ( 'NONE',  ( 4.502618398017903090, 20.03723546437915104, 11.49999999999998934 ) ) ;
#46806 = CARTESIAN_POINT ( 'NONE',  ( 15.94332860179727618, 4.994534053091038039, -27.96060887785597515 ) ) ;
#46807 = ORIENTED_EDGE ( 'NONE', *, *, #50155, .T. ) ;
#46808 = DIRECTION ( 'NONE',  ( -3.773278334453080206E-23, 0.9999999999976377785, 2.173523156925979975E-06 ) ) ;
#46809 = VERTEX_POINT ( 'NONE', #68149 ) ;
#46810 = CARTESIAN_POINT ( 'NONE',  ( -70.62287095715005592, -29.50250786944525672, 11.44777988621623699 ) ) ;
#46811 = B_SPLINE_CURVE_WITH_KNOTS ( 'NONE', 3,
 ( #10177, #24393, #55363, #17285, #23888, #47241, #9169, #63487, #33019, #71083, #10679, #63994, #48248, #32009 ),
 .UNSPECIFIED., .F., .F.,
 ( 4, 2, 2, 2, 2, 2, 4 ),
 ( 0.000000000000000000, 0.0001575354624298309881, 0.0003150709248596619762, 0.0006301418497193228682, 0.0009452127745789835975, 0.001102748237008804259, 0.001260283699438624703 ),
 .UNSPECIFIED. ) ;
#46812 = CARTESIAN_POINT ( 'NONE',  ( -110.6228709571500701, -23.48786465467241769, 11.44779295918254114 ) ) ;
#46813 = ORIENTED_EDGE ( 'NONE', *, *, #33624, .T. ) ;
#46814 = ORIENTED_EDGE ( 'NONE', *, *, #84842, .F. ) ;
#46815 = AXIS2_PLACEMENT_3D ( 'NONE', #9594, #39545, #40553 ) ;
#46816 = B_SPLINE_CURVE_WITH_KNOTS ( 'NONE', 3,
 ( #767, #54558, #25094, #9876 ),
 .UNSPECIFIED., .F., .F.,
 ( 4, 4 ),
 ( 0.000000000000000000, 1.000000000000000000 ),
 .UNSPECIFIED. ) ;
#46817 = ORIENTED_EDGE ( 'NONE', *, *, #22863, .T. ) ;
#46818 = CARTESIAN_POINT ( 'NONE',  ( -23.62875734969026453, 6.143225279485574397, 24.50402280011862288 ) ) ;
#46819 = CARTESIAN_POINT ( 'NONE',  ( -49.54700823480037997, -25.07535432491515692, 7.358156397503878843 ) ) ;
#46820 = CARTESIAN_POINT ( 'NONE',  ( -19.77875734969026311, -3.316774720514426456, 27.45402280011862572 ) ) ;
#46821 = CARTESIAN_POINT ( 'NONE',  ( 0.06016934085327452914, 20.63536315578604174, -1.500000000000002220 ) ) ;
#46822 = CARTESIAN_POINT ( 'NONE',  ( 7.401388779597747103, 20.28278527911644247, 11.49999999999999645 ) ) ;
#46823 = ORIENTED_EDGE ( 'NONE', *, *, #91704, .T. ) ;
#46824 = CARTESIAN_POINT ( 'NONE',  ( -83.62287095715002749, -23.94994826722515668, -0.6494450866351706431 ) ) ;
#46825 = CARTESIAN_POINT ( 'NONE',  ( 3.183477995988301945, -5.876774720514404748, 18.35601591497023577 ) ) ;
#46826 = CARTESIAN_POINT ( 'NONE',  ( 3.152853332073482839, 22.16862046936333286, 11.49999999999998934 ) ) ;
#46827 = ADVANCED_FACE ( 'NONE', ( #61543 ), #53925, .F. ) ;
#46828 = DIRECTION ( 'NONE',  ( -3.773278334453079030E-23, 0.9999999999976377785, 2.173523156925979128E-06 ) ) ;
#46829 = PLANE ( 'NONE',  #72404 ) ;
#46830 = ORIENTED_EDGE ( 'NONE', *, *, #100082, .T. ) ;
#46831 = CARTESIAN_POINT ( 'NONE',  ( -99.57937527035555547, -25.29211892742296541, 4.244792190146649880 ) ) ;
#46832 = CARTESIAN_POINT ( 'NONE',  ( -67.62287095715005592, -23.48786465467241058, 11.44779295918254647 ) ) ;
#46833 = CARTESIAN_POINT ( 'NONE',  ( -0.7727808018759799724, -20.89725122839497828, 11.49999999999998934 ) ) ;
#46834 = ORIENTED_EDGE ( 'NONE', *, *, #97067, .F. ) ;
#46835 = CARTESIAN_POINT ( 'NONE',  ( -120.6228709571500417, -29.50248789122583659, 2.256150453626215580 ) ) ;
#46836 = ORIENTED_EDGE ( 'NONE', *, *, #95504, .F. ) ;
#46837 = CARTESIAN_POINT ( 'NONE',  ( -109.5126105237879841, -24.66019654487200441, 8.947790411086113949 ) ) ;
#46838 = CARTESIAN_POINT ( 'NONE',  ( -17.86006801910157193, 11.38285951858322242, -1.500000000000002220 ) ) ;
#46839 = ORIENTED_EDGE ( 'NONE', *, *, #73631, .F. ) ;
#46840 = CARTESIAN_POINT ( 'NONE',  ( -50.63860451389618333, -24.52300882791530157, 0.6510814631126389251 ) ) ;
#46841 = CARTESIAN_POINT ( 'NONE',  ( 10.97640485992876691, 18.82695874702771377, -1.500000000000002220 ) ) ;
#46842 = CARTESIAN_POINT ( 'NONE',  ( -121.5228709571500332, -23.73934037231757443, 11.05740245334328087 ) ) ;
#46843 = DIRECTION ( 'NONE',  ( -3.773278334453079618E-23, 0.9999999999976377785, 2.173523156925979975E-06 ) ) ;
#46844 = LINE ( 'NONE', #85389, #88663 ) ;
#46845 = CARTESIAN_POINT ( 'NONE',  ( 21.63681353182189682, 2.665401433100548889, -1.500000000000002220 ) ) ;
#46846 = CARTESIAN_POINT ( 'NONE',  ( 6.429811694900724461, -5.876774720514425177, 21.48000018967326596 ) ) ;
#46847 = ORIENTED_EDGE ( 'NONE', *, *, #94638, .F. ) ;
#46848 = CARTESIAN_POINT ( 'NONE',  ( 7.107139210497321002, -5.876774720514413630, 19.78447747620696617 ) ) ;
#46849 = LINE ( 'NONE', #31109, #97815 ) ;
#46850 = ORIENTED_EDGE ( 'NONE', *, *, #24568, .F. ) ;
#46851 = ORIENTED_EDGE ( 'NONE', *, *, #34078, .T. ) ;
#46852 = EDGE_LOOP ( 'NONE', ( #65940, #55824, #42437, #51946, #69028, #95146, #74407 ) ) ;
#46853 = CARTESIAN_POINT ( 'NONE',  ( -28.04362312726946271, -24.81012858093322038, 2.323251710168637185 ) ) ;
#46854 = CARTESIAN_POINT ( 'NONE',  ( -44.62287095715004881, -23.72747288104469732, -1.053458166803227458 ) ) ;
#46855 = CARTESIAN_POINT ( 'NONE',  ( 7.993063233546146229, -19.64520799392144568, 11.49999999999998934 ) ) ;
#46856 = CARTESIAN_POINT ( 'NONE',  ( -94.51552831490990059, -23.96119346886881019, -0.6495511937832051386 ) ) ;
#46857 = CARTESIAN_POINT ( 'NONE',  ( -95.62287095715005592, -23.47596703998600631, 11.44779298504227860 ) ) ;
#46858 = CARTESIAN_POINT ( 'NONE',  ( -80.48900664166535535, -25.13313949306887807, 7.101635536975466678 ) ) ;
#46859 = DIRECTION ( 'NONE',  ( -0.000000000000000000, -1.000000000000000000, -0.000000000000000000 ) ) ;
#46860 = CARTESIAN_POINT ( 'NONE',  ( 7.147005326088517130, -18.03964237587283037, 11.49999999999998934 ) ) ;
#46861 = ADVANCED_FACE ( 'NONE', ( #77227 ), #91467, .F. ) ;
#46862 = CARTESIAN_POINT ( 'NONE',  ( -39.98075019704535293, -25.25978494880519776, 3.590542803917028181 ) ) ;
#46863 = ORIENTED_EDGE ( 'NONE', *, *, #61611, .T. ) ;
#46864 = VECTOR ( 'NONE', #4378, 1000.000000000000114 ) ;
#46865 = CARTESIAN_POINT ( 'NONE',  ( -14.69715086760845857, -12.76062437926726290, 11.49999999999999645 ) ) ;
#46866 = CARTESIAN_POINT ( 'NONE',  ( 20.60020833695035236, 1.530808498934189845E-16, -1.249999999999998446 ) ) ;
#46867 = AXIS2_PLACEMENT_3D ( 'NONE', #98891, #61353, #7049 ) ;
#46868 = CARTESIAN_POINT ( 'NONE',  ( -107.5228709571500758, -24.65952944569304961, 1.056160979905704123 ) ) ;
#46869 = EDGE_CURVE ( 'NONE', #97499, #41750, #44321, .T. ) ;
#46870 = VERTEX_POINT ( 'NONE', #98580 ) ;
#46871 = CARTESIAN_POINT ( 'NONE',  ( -93.62287095715004170, -23.94994826722515668, -0.6494450866351687557 ) ) ;
#46872 = DIRECTION ( 'NONE',  ( 0.9980236263794188822, 0.000000000000000000, -0.06283980576413539243 ) ) ;
#46873 = B_SPLINE_CURVE_WITH_KNOTS ( 'NONE', 3,
 ( #33315, #25203, #371, #56181, #87106, #31318, #70897, #63295, #48572, #79496, #64302, #25706, #35333, #3395, #49564, #26214 ),
 .UNSPECIFIED., .F., .F.,
 ( 4, 2, 2, 2, 2, 2, 2, 4 ),
 ( 0.000000000000000000, 0.0002741513364169689197, 0.0005483026728339378394, 0.0008224540092509068133, 0.001096605345667875679, 0.001644908018501813627, 0.001919059354918762651, 0.002193210691335711893 ),
 .UNSPECIFIED. ) ;
#46874 = CARTESIAN_POINT ( 'NONE',  ( -3.826923076923078426, -6.376774720514408301, 19.19230769230769695 ) ) ;
#46875 = CARTESIAN_POINT ( 'NONE',  ( -93.50526767657690641, -24.66019654487200441, 8.947790411086105067 ) ) ;
#46876 = CARTESIAN_POINT ( 'NONE',  ( 19.42422255247381457, -2.945173967302487039, 11.49999999999998934 ) ) ;
#46877 = CIRCLE ( 'NONE', #64737, 10.80000000000000782 ) ;
#46878 = CARTESIAN_POINT ( 'NONE',  ( -4.686006777320704586, 0.3587747205144265483, 29.60911411231907309 ) ) ;
#46879 = VERTEX_POINT ( 'NONE', #60050 ) ;
#46880 = CARTESIAN_POINT ( 'NONE',  ( 18.62697458635512859, 10.92912097662538251, -1.500000000000002220 ) ) ;
#46881 = VECTOR ( 'NONE', #35069, 1000.000000000000000 ) ;
#46882 = CARTESIAN_POINT ( 'NONE',  ( -40.60175827569378981, -24.15503026093912453, -0.2815557561904605266 ) ) ;
#46883 = CARTESIAN_POINT ( 'NONE',  ( 8.000000000000003553, -5.876774720514426953, 0.000000000000000000 ) ) ;
#46884 = CARTESIAN_POINT ( 'NONE',  ( -15.77545706029219730, -16.76941864122914083, -1.500000000000002220 ) ) ;
#46885 = CC_DESIGN_PERSON_AND_ORGANIZATION_ASSIGNMENT ( #23158, #85074, ( #31288 ) ) ;
#46886 = SECURITY_CLASSIFICATION_LEVEL ( 'unclassified' ) ;
#46887 = FACE_OUTER_BOUND ( 'NONE', #90157, .T. ) ;
#46888 = CARTESIAN_POINT ( 'NONE',  ( 4.639188450898540594, -6.376774720514418959, 20.39229233339611014 ) ) ;
#46889 = CARTESIAN_POINT ( 'NONE',  ( -40.85509153498097845, -25.20774029359534296, 6.732786232439175400 ) ) ;
#46890 = CARTESIAN_POINT ( 'NONE',  ( -101.8274488899549368, -25.20041407164857361, 6.674697471738888943 ) ) ;
#46891 = CARTESIAN_POINT ( 'NONE',  ( -110.6079876523469920, -25.10921379075584525, 2.855977848569461575 ) ) ;
#46892 = CARTESIAN_POINT ( 'NONE',  ( -121.6228709571500275, -24.66019654487200441, 8.947790411086119278 ) ) ;
#46893 = CARTESIAN_POINT ( 'NONE',  ( -99.25286268653823640, -25.26400796470216292, 4.527133510428875240 ) ) ;
#46894 = CARTESIAN_POINT ( 'NONE',  ( 15.94990109002195489, -11.90149544800030590, 11.49999999999998934 ) ) ;
#46895 = CARTESIAN_POINT ( 'NONE',  ( -101.2870029445573010, -25.25608464488718496, 3.797624798826384040 ) ) ;
#46896 = CARTESIAN_POINT ( 'NONE',  ( -7.754168067426306266, 18.25094163199162622, -1.500000000000002220 ) ) ;
#46897 = PLANE ( 'NONE',  #32973 ) ;
#46898 = CARTESIAN_POINT ( 'NONE',  ( -39.57984969116796492, -25.29116578775463964, 3.109569074945083944 ) ) ;
#46899 = CARTESIAN_POINT ( 'NONE',  ( -42.52287095715006870, -23.94994826722564696, -0.6494450866342741380 ) ) ;
#46900 = CARTESIAN_POINT ( 'NONE',  ( -19.59449498831206782, -6.737714454370689054, 11.49999999999999645 ) ) ;
#46901 = CARTESIAN_POINT ( 'NONE',  ( -7.640476926272304681, -6.376774720514415407, 20.25188360057253689 ) ) ;
#46902 = CARTESIAN_POINT ( 'NONE',  ( -78.52287095715007581, -23.72773821059536914, 11.05748984161097503 ) ) ;
#46903 = VECTOR ( 'NONE', #41166, 1000.000000000000114 ) ;
#46904 = CARTESIAN_POINT ( 'NONE',  ( 20.42703387425654427, 10.12935691860780985, 11.49999999999999645 ) ) ;
#46905 = ORIENTED_EDGE ( 'NONE', *, *, #88074, .T. ) ;
#46906 = FACE_OUTER_BOUND ( 'NONE', #89273, .T. ) ;
#46907 = DIRECTION ( 'NONE',  ( 0.7512896232465892110, 0.000000000000000000, 0.6599726524652350657 ) ) ;
#46908 = ORIENTED_EDGE ( 'NONE', *, *, #91847, .F. ) ;
#46909 = CARTESIAN_POINT ( 'NONE',  ( -16.67386609800740516, 11.36076560755915033, 11.49999999999998934 ) ) ;
#46910 = B_SPLINE_CURVE_WITH_KNOTS ( 'NONE', 3,
 ( #92073, #22544, #14944, #5351, #5847, #45915 ),
 .UNSPECIFIED., .F., .F.,
 ( 4, 2, 4 ),
 ( 0.000000000000000000, 0.001380764517854764532, 0.002761529035709529064 ),
 .UNSPECIFIED. ) ;
#46911 = CARTESIAN_POINT ( 'NONE',  ( -19.37210865224160017, 5.965225279485592225, -21.60955166348795586 ) ) ;
#46912 = CARTESIAN_POINT ( 'NONE',  ( -69.58953762381672448, -23.48783264082478084, -1.443836473390067265 ) ) ;
#46913 = VERTEX_POINT ( 'NONE', #90977 ) ;
#46914 = ORIENTED_EDGE ( 'NONE', *, *, #7154, .T. ) ;
#46915 = CARTESIAN_POINT ( 'NONE',  ( 14.52511747680497933, -5.965225279485572685, -27.86035006098926559 ) ) ;
#46916 = CARTESIAN_POINT ( 'NONE',  ( 7.980177114813061579, 21.45908683785374649, 11.49999999999998934 ) ) ;
#46917 = CARTESIAN_POINT ( 'NONE',  ( -41.86995616089614458, -25.28979658489737048, 4.210709715701590028 ) ) ;
#46918 = CARTESIAN_POINT ( 'NONE',  ( 11.52859134480388903, -18.33581920571378632, -1.500000000000002220 ) ) ;
#46919 = CARTESIAN_POINT ( 'NONE',  ( 20.60020833695035236, 0.000000000000000000, 0.000000000000000000 ) ) ;
#46920 = EDGE_CURVE ( 'NONE', #56862, #94573, #95923, .T. ) ;
#46921 = CARTESIAN_POINT ( 'NONE',  ( 20.33208665566141704, 4.825383418962623239, 11.49999999999999645 ) ) ;
#46922 = ORIENTED_EDGE ( 'NONE', *, *, #13322, .F. ) ;
#46923 = CARTESIAN_POINT ( 'NONE',  ( -69.42561217104606897, -25.24754309793884843, 5.145891976043102112 ) ) ;
#46924 = CARTESIAN_POINT ( 'NONE',  ( -7.807709442696729063, 20.60712426125841645, 11.49999999999998934 ) ) ;
#46925 = ADVANCED_FACE ( 'NONE', ( #60551 ), #85866, .T. ) ;
#46926 = AXIS2_PLACEMENT_3D ( 'NONE', #34682, #72753, #89466 ) ;
#46927 = CARTESIAN_POINT ( 'NONE',  ( 9.940598223437577374, -6.376774720514426953, 22.08128695274315945 ) ) ;
#46928 = CARTESIAN_POINT ( 'NONE',  ( -65.62287095715005592, -24.99156045073393173, 7.747789690856161648 ) ) ;
#46929 = ORIENTED_EDGE ( 'NONE', *, *, #62159, .T. ) ;
#46930 = CARTESIAN_POINT ( 'NONE',  ( -49.56515190845122021, -25.18440198093164639, 3.736414966849777475 ) ) ;
#46931 = CARTESIAN_POINT ( 'NONE',  ( -46.52287095715007581, -23.48783264082477018, -1.443836473390096797 ) ) ;
#46932 = ORIENTED_EDGE ( 'NONE', *, *, #96086, .F. ) ;
#46933 = CARTESIAN_POINT ( 'NONE',  ( -25.92875734969026524, 5.356774720514425603, -0.08597719988137648983 ) ) ;
#46934 = ORIENTED_EDGE ( 'NONE', *, *, #47154, .F. ) ;
#46935 = VECTOR ( 'NONE', #57066, 1000.000000000000000 ) ;
#46936 = VERTEX_POINT ( 'NONE', #79747 ) ;
#46937 = CARTESIAN_POINT ( 'NONE',  ( -106.6228709571500559, -24.65952944569304606, 1.056160979905703012 ) ) ;
#46938 = DIRECTION ( 'NONE',  ( 1.955152872784845154E-15, 1.000000000000000000, -3.740001113483016365E-15 ) ) ;
#46940 = EDGE_CURVE ( 'NONE', #80243, #43471, #23435, .T. ) ;
#46939 = CARTESIAN_POINT ( 'NONE',  ( -4.147110899021980934, -5.876774720514418071, 20.45311193189268906 ) ) ;
#46941 = B_SPLINE_CURVE_WITH_KNOTS ( 'NONE', 3,
 ( #56513, #54632, #41274, #57014, #17935, #79822, #15052, #46024 ),
 .UNSPECIFIED., .F., .F.,
 ( 4, 2, 2, 4 ),
 ( -0.001224554619866339558, -0.0002241820295893590283, 0.0007761905606876215013, 0.002776935741241573670 ),
 .UNSPECIFIED. ) ;
#46942 = CARTESIAN_POINT ( 'NONE',  ( 6.539103723289373171, -19.38406401830294712, -1.500000000000002220 ) ) ;
#46943 = ORIENTED_EDGE ( 'NONE', *, *, #87867, .F. ) ;
#46944 = CARTESIAN_POINT ( 'NONE',  ( -79.52287095715010423, -23.47593901973090524, -1.443836447538996870 ) ) ;
#46945 = AXIS2_PLACEMENT_3D ( 'NONE', #69685, #24497, #23996 ) ;
#46946 = CARTESIAN_POINT ( 'NONE',  ( -62.52287095715006160, -23.48783264082477018, -1.443836473390091912 ) ) ;
#46947 = CARTESIAN_POINT ( 'NONE',  ( -77.58953762381673869, -24.64898659630367916, 1.056161002820385830 ) ) ;
#46948 = CARTESIAN_POINT ( 'NONE',  ( 20.80681148587913754, 8.022540738981085440, 11.49999999999998934 ) ) ;
#46949 = CARTESIAN_POINT ( 'NONE',  ( -28.32169924589829080, -0.3587747205143964613, -8.244178532169451401 ) ) ;
#46950 = CARTESIAN_POINT ( 'NONE',  ( -124.6228709571500559, -29.50247984919015209, -1.443849546365046699 ) ) ;
#46951 = EDGE_LOOP ( 'NONE', ( #98462, #64078, #84825, #97493, #34839, #43328, #10529, #29578 ) ) ;
#46952 = DIRECTION ( 'NONE',  ( 0.1478094111296165691, -0.9890158633619158257, 0.000000000000000000 ) ) ;
#46953 = VECTOR ( 'NONE', #11132, 1000.000000000000114 ) ;
#46954 = PLANE ( 'NONE',  #81549 ) ;
#46955 = VECTOR ( 'NONE', #44809, 1000.000000000000000 ) ;
#46956 = CARTESIAN_POINT ( 'NONE',  ( -4.186882374726557110, 20.40937146592452223, -1.500000000000002220 ) ) ;
#46957 = ORIENTED_EDGE ( 'NONE', *, *, #20955, .T. ) ;
#46959 = EDGE_LOOP ( 'NONE', ( #3793, #75899, #42937, #44100 ) ) ;
#46958 = DIRECTION ( 'NONE',  ( -3.773278334453079030E-23, 0.9999999999976377785, 2.173523156925979128E-06 ) ) ;
#46960 = VERTEX_POINT ( 'NONE', #2148 ) ;
#46961 = AXIS2_PLACEMENT_3D ( 'NONE', #13005, #43482, #43971 ) ;
#46962 = CARTESIAN_POINT ( 'NONE',  ( -58.52287095715006160, -24.64965694238407323, 8.947790433994201820 ) ) ;
#46963 = CARTESIAN_POINT ( 'NONE',  ( 8.737904895026865404, 19.08465823478955414, -1.500000000000002220 ) ) ;
#46964 = ORIENTED_EDGE ( 'NONE', *, *, #7401, .T. ) ;
#46965 = CARTESIAN_POINT ( 'NONE',  ( -110.6228709571500275, -24.91544648472627088, 1.928969306349440194 ) ) ;
#46966 = CARTESIAN_POINT ( 'NONE',  ( 2.230654205607476293, 0.1647943925233646134, -7.514475724998474108E-17 ) ) ;
#46967 = CARTESIAN_POINT ( 'NONE',  ( 10.22845072388260768, -5.356774720514425603, -24.98266432381545954 ) ) ;
#46968 = CARTESIAN_POINT ( 'NONE',  ( -51.58953762381673158, -24.65952944569304606, 1.056160979905695463 ) ) ;
#46969 = CARTESIAN_POINT ( 'NONE',  ( -92.55803716275170245, -23.73791477778912196, 11.05961554403170588 ) ) ;
#46970 = CARTESIAN_POINT ( 'NONE',  ( -119.6228709571500559, -23.48783264082479150, -1.443836473390058384 ) ) ;
#46972 = ORIENTED_EDGE ( 'NONE', *, *, #25636, .F. ) ;
#46971 = CARTESIAN_POINT ( 'NONE',  ( -21.91774099701738621, 3.392077650570975766, 11.49999999999999645 ) ) ;
#46973 = DIRECTION ( 'NONE',  ( -3.773278334453079618E-23, 0.9999999999976377785, 2.173523156925979975E-06 ) ) ;
#46974 = PLANE ( 'NONE',  #91002 ) ;
#46975 = ORIENTED_EDGE ( 'NONE', *, *, #51743, .T. ) ;
#46976 = CARTESIAN_POINT ( 'NONE',  ( -16.08347380570801377, -15.98036338121420030, -1.500000000000002220 ) ) ;
#46978 = ORIENTED_EDGE ( 'NONE', *, *, #87257, .F. ) ;
#46977 = DIRECTION ( 'NONE',  ( 0.000000000000000000, 0.000000000000000000, 1.000000000000000000 ) ) ;
#46979 = EDGE_CURVE ( 'NONE', #42205, #92012, #80101, .T. ) ;
#46980 = ORIENTED_EDGE ( 'NONE', *, *, #74006, .F. ) ;
#46981 = CARTESIAN_POINT ( 'NONE',  ( 31.27206728860909024, 4.132774720514318822, -3.930752063305056332 ) ) ;
#46982 = ADVANCED_FACE ( 'NONE', ( #31570 ), #31065, .T. ) ;
#46983 = CARTESIAN_POINT ( 'NONE',  ( 19.96388892861992659, -2.714421270036905032, 11.49999999999998934 ) ) ;
#46984 = CARTESIAN_POINT ( 'NONE',  ( 24.71017632900191074, 5.356774720514427379, -0.3523920347467613956 ) ) ;
#46985 = ORIENTED_EDGE ( 'NONE', *, *, #54143, .F. ) ;
#46986 = LINE ( 'NONE', #23624, #94081 ) ;
#46987 = CARTESIAN_POINT ( 'NONE',  ( -5.491053050139323766, 21.65304554001118120, -1.500000000000002220 ) ) ;
#46988 = ORIENTED_EDGE ( 'NONE', *, *, #34691, .F. ) ;
#46989 = VERTEX_POINT ( 'NONE', #87360 ) ;
#46990 = CARTESIAN_POINT ( 'NONE',  ( -101.4810573493621177, -25.16257346776554371, 6.435289059764511599 ) ) ;
#46991 = CARTESIAN_POINT ( 'NONE',  ( -89.62287095715002749, -24.50321055353805022, 9.387540953477527594 ) ) ;
#46992 = CARTESIAN_POINT ( 'NONE',  ( -65.62287095715005592, -25.00158670708909270, 2.256160236439166855 ) ) ;
#46993 = FACE_BOUND ( 'NONE', #13629, .T. ) ;
#46994 = CARTESIAN_POINT ( 'NONE',  ( -97.25593758936675215, -24.04615231314291890, -0.4716817114508916609 ) ) ;
#46995 = CARTESIAN_POINT ( 'NONE',  ( -13.18904525526904692, 14.46673508071025971, -1.500000000000002220 ) ) ;
#46996 = DIRECTION ( 'NONE',  ( -3.773278334453079618E-23, 0.9999999999976377785, 2.173523156925979975E-06 ) ) ;
#46997 = CARTESIAN_POINT ( 'NONE',  ( 17.49997855696484095, 12.48231381050728928, 11.49999999999998934 ) ) ;
#46998 = CARTESIAN_POINT ( 'NONE',  ( -128.5215775092486865, -24.34968618360935011, 0.1864209137779018477 ) ) ;
#46999 = DIRECTION ( 'NONE',  ( 0.000000000000000000, -1.000000000000000000, 0.000000000000000000 ) ) ;
#47000 = CARTESIAN_POINT ( 'NONE',  ( 1.600000000000000977, 24.00000000000000000, 0.000000000000000000 ) ) ;
#47001 = AXIS2_PLACEMENT_3D ( 'NONE', #39315, #46938, #54065 ) ;
#47002 = CARTESIAN_POINT ( 'NONE',  ( -28.98875734969026041, -5.965225279485572685, 15.62202280011862321 ) ) ;
#47003 = CARTESIAN_POINT ( 'NONE',  ( 17.53461989915211916, -14.66684187699354425, -1.500000000000002220 ) ) ;
#47004 = ADVANCED_FACE ( 'NONE', ( #40695 ), #71148, .F. ) ;
#47005 = APPROVAL ( #92663, 'UNSPECIFIED' ) ;
#47006 = B_SPLINE_CURVE_WITH_KNOTS ( 'NONE', 3,
 ( #52145, #51650, #20680, #13564 ),
 .UNSPECIFIED., .F., .F.,
 ( 4, 4 ),
 ( 0.000000000000000000, 0.0001000000000000028644 ),
 .UNSPECIFIED. ) ;
#47007 = PERSON_AND_ORGANIZATION_ROLE ( 'creator' ) ;
#47008 = PLANE ( 'NONE',  #49935 ) ;
#47009 = DIRECTION ( 'NONE',  ( 0.000000000000000000, -0.9999999999976377785, -2.173523156925979975E-06 ) ) ;
#47010 = CARTESIAN_POINT ( 'NONE',  ( -8.782848147209532996, 18.00178819457707746, 11.49999999999999645 ) ) ;
#47011 = CARTESIAN_POINT ( 'NONE',  ( -78.94303308397306296, -25.31594635886830957, 5.977536581945547489 ) ) ;
#47012 = CARTESIAN_POINT ( 'NONE',  ( 30.09341516180546350, 1.477225279485574028, -11.39311774897855933 ) ) ;
#47013 = VECTOR ( 'NONE', #57945, 1000.000000000000000 ) ;
#47014 = B_SPLINE_CURVE_WITH_KNOTS ( 'NONE', 3,
 ( #388, #16108, #45579, #67921 ),
 .UNSPECIFIED., .F., .F.,
 ( 4, 4 ),
 ( 0.000000000000000000, 0.0001000000000000028644 ),
 .UNSPECIFIED. ) ;
#47015 = DIRECTION ( 'NONE',  ( 0.000000000000000000, 2.173523156893721996E-06, -0.9999999999976377785 ) ) ;
#47016 = LINE ( 'NONE', #62755, #52144 ) ;
#47017 = ORIENTED_EDGE ( 'NONE', *, *, #75034, .T. ) ;
#47018 = CARTESIAN_POINT ( 'NONE',  ( -110.6228709571500559, -23.47593901973091235, -1.443836447538999312 ) ) ;
#47019 = CARTESIAN_POINT ( 'NONE',  ( 9.899741330608472722, -19.37759744025533593, 11.49999999999998934 ) ) ;
#47020 = ADVANCED_FACE ( 'NONE', ( #39682 ), #69646, .F. ) ;
#47021 = DIRECTION ( 'NONE',  ( 1.000000000000000000, 3.773278334444167608E-23, 8.201307833595939069E-29 ) ) ;
#47022 = VECTOR ( 'NONE', #3271, 1000.000000000000000 ) ;
#47023 = CARTESIAN_POINT ( 'NONE',  ( -19.15281226579456231, 4.489446101945751444, -1.500000000000002220 ) ) ;
#47024 = CARTESIAN_POINT ( 'NONE',  ( -38.58953762381672448, -23.48786465467240703, 11.44779295918255180 ) ) ;
#47025 = CIRCLE ( 'NONE', #74603, 1.149999999999998135 ) ;
#47026 = CARTESIAN_POINT ( 'NONE',  ( -41.46019029217195850, -25.26930233494256584, 4.061970619173578712 ) ) ;
#47027 = COORDINATED_UNIVERSAL_TIME_OFFSET ( 0, 0, .AHEAD. ) ;
#47028 = VECTOR ( 'NONE', #63935, 1000.000000000000114 ) ;
#47029 = CARTESIAN_POINT ( 'NONE',  ( -91.59147232029850727, -24.15620529776628445, 10.23563542870660115 ) ) ;
#47030 = FACE_OUTER_BOUND ( 'NONE', #73024, .T. ) ;
#47031 = CARTESIAN_POINT ( 'NONE',  ( 1.511266892140219920, 20.53031905857337591, 11.49999999999999645 ) ) ;
#47032 = LINE ( 'NONE', #21665, #14905 ) ;
#47033 = CARTESIAN_POINT ( 'NONE',  ( -120.5543864198989183, -24.40034930558991633, 0.3402023900116107336 ) ) ;
#47034 = VECTOR ( 'NONE', #18899, 1000.000000000000114 ) ;
#47035 = CARTESIAN_POINT ( 'NONE',  ( 22.48748499206561746, 2.281147167042596013, 11.49999999999999645 ) ) ;
#47036 = ORIENTED_EDGE ( 'NONE', *, *, #21959, .F. ) ;
#47037 = CARTESIAN_POINT ( 'NONE',  ( -100.0631793594960044, -25.26387431326939037, 4.632689007454804830 ) ) ;
#47038 = CARTESIAN_POINT ( 'NONE',  ( -60.58953762381673158, -24.99132157543084531, 2.256160258750496972 ) ) ;
#47039 = VECTOR ( 'NONE', #17095, 1000.000000000000114 ) ;
#47040 = CARTESIAN_POINT ( 'NONE',  ( -125.6257034592155861, -23.85049219812686516, 10.88485053497526778 ) ) ;
#47041 = DIRECTION ( 'NONE',  ( -0.5630016722799275897, 0.000000000000000000, 0.8264557562326038109 ) ) ;
#47042 = EDGE_CURVE ( 'NONE', #53195, #41736, #7486, .T. ) ;
#47043 = CARTESIAN_POINT ( 'NONE',  ( -26.14934357328621317, -24.61459939561487786, 7.450065485979896707 ) ) ;
#47044 = CARTESIAN_POINT ( 'NONE',  ( 32.65112488154859705, 3.727967435732443047, -2.714891177973568492 ) ) ;
#47045 = ORIENTED_EDGE ( 'NONE', *, *, #56427, .F. ) ;
#47046 = CARTESIAN_POINT ( 'NONE',  ( -8.497478458550677516, -21.44862750780143656, 11.49999999999999645 ) ) ;
#47047 = B_SPLINE_CURVE_WITH_KNOTS ( 'NONE', 3,
 ( #57779, #87723, #89218, #3491 ),
 .UNSPECIFIED., .F., .F.,
 ( 4, 4 ),
 ( 0.2499644179499421748, 0.2589708492220576530 ),
 .UNSPECIFIED. ) ;
#47048 = CARTESIAN_POINT ( 'NONE',  ( 19.59772090806136902, -11.66877021596143926, 11.49999999999998934 ) ) ;
#47049 = PLANE ( 'NONE',  #59998 ) ;
#47050 = CARTESIAN_POINT ( 'NONE',  ( -96.55782209890644197, -23.73766607897670511, -1.055555164236452681 ) ) ;
#47051 = FACE_OUTER_BOUND ( 'NONE', #62849, .T. ) ;
#47052 = CARTESIAN_POINT ( 'NONE',  ( 21.09243369641204069, 7.689775423913054908, 11.49999999999999645 ) ) ;
#47053 = ORIENTED_EDGE ( 'NONE', *, *, #73622, .F. ) ;
#47054 = DIRECTION ( 'NONE',  ( 0.1875268396392987258, 0.000000000000000000, 0.9822594791677485837 ) ) ;
#47055 = B_SPLINE_CURVE_WITH_KNOTS ( 'NONE', 3,
 ( #98120, #29614, #68190, #36246 ),
 .UNSPECIFIED., .F., .F.,
 ( 4, 4 ),
 ( 0.000000000000000000, 1.000000000000000000 ),
 .UNSPECIFIED. ) ;
#47056 = CARTESIAN_POINT ( 'NONE',  ( -34.62287095715005592, -23.95044443724991368, 10.65354141964650303 ) ) ;
#47057 = CARTESIAN_POINT ( 'NONE',  ( 15.37660858059359725, 15.65766701038582021, -1.500000000000002220 ) ) ;
#47058 = EDGE_CURVE ( 'NONE', #79151, #77983, #78727, .T. ) ;
#47059 = CARTESIAN_POINT ( 'NONE',  ( -5.023036858974360364, -5.876774720514408301, 19.14743589743590491 ) ) ;
#47060 = FACE_OUTER_BOUND ( 'NONE', #13415, .T. ) ;
#47061 = CARTESIAN_POINT ( 'NONE',  ( -74.62287095715005592, -23.48786465467241058, 11.44779295918254469 ) ) ;
#47062 = ORIENTED_EDGE ( 'NONE', *, *, #69130, .T. ) ;
#47063 = LINE ( 'NONE', #83600, #24885 ) ;
#47064 = CARTESIAN_POINT ( 'NONE',  ( 30.53060340732036337, -5.329285123471891872, 3.289350009555732868 ) ) ;
#47065 = VERTEX_POINT ( 'NONE', #94972 ) ;
#47066 = CARTESIAN_POINT ( 'NONE',  ( -3.437008290023895185, 20.19323497536227663, 11.49999999999998934 ) ) ;
#47067 = ORIENTED_EDGE ( 'NONE', *, *, #11877, .F. ) ;
#47068 = EDGE_LOOP ( 'NONE', ( #67832, #95663, #51819, #76079 ) ) ;
#47069 = ORIENTED_EDGE ( 'NONE', *, *, #54638, .T. ) ;
#47070 = ORIENTED_EDGE ( 'NONE', *, *, #55328, .F. ) ;
#47071 = CARTESIAN_POINT ( 'NONE',  ( -10.32085834726444595, 20.65377284989807194, 11.49999999999998934 ) ) ;
#47073 = EDGE_CURVE ( 'NONE', #95103, #32116, #15925, .T. ) ;
#47072 = CARTESIAN_POINT ( 'NONE',  ( -49.98363062963033343, -25.13033135890777459, 2.887186111250463760 ) ) ;
#47074 = CARTESIAN_POINT ( 'NONE',  ( -3.904290608643684379, -19.93223805144805283, -1.500000000000002220 ) ) ;
#47075 = ORIENTED_EDGE ( 'NONE', *, *, #26088, .T. ) ;
#47076 = CARTESIAN_POINT ( 'NONE',  ( 29.76209104404536987, 5.356774720514427379, 26.42884784083909366 ) ) ;
#47077 = CARTESIAN_POINT ( 'NONE',  ( -92.59760823315281186, -23.73766607897671221, -1.055555164236430477 ) ) ;
#47078 = EDGE_CURVE ( 'NONE', #36444, #26340, #70638, .T. ) ;
#47079 = CARTESIAN_POINT ( 'NONE',  ( -39.62287095715005592, -23.47596703998600276, 11.44779298504227505 ) ) ;
#47080 = CARTESIAN_POINT ( 'NONE',  ( 4.281720980632043094, -6.376774720514408301, 18.71132571341777151 ) ) ;
#47082 = ORIENTED_EDGE ( 'NONE', *, *, #66649, .T. ) ;
#47081 = CARTESIAN_POINT ( 'NONE',  ( -21.26083644630951142, -3.357327265692296780, 11.49999999999999645 ) ) ;
#47083 = FACE_OUTER_BOUND ( 'NONE', #42652, .T. ) ;
#47084 = CARTESIAN_POINT ( 'NONE',  ( 15.89146238746078765, 3.595713655330297520, -28.00617091144485826 ) ) ;
#47085 = ORIENTED_EDGE ( 'NONE', *, *, #44738, .T. ) ;
#47086 = CARTESIAN_POINT ( 'NONE',  ( -14.15296684469643118, 15.14645709676483420, -1.500000000000002220 ) ) ;
#47087 = CIRCLE ( 'NONE', #97335, 1.020000000000000018 ) ;
#47088 = ORIENTED_EDGE ( 'NONE', *, *, #98511, .T. ) ;
#47090 = ORIENTED_EDGE ( 'NONE', *, *, #44413, .T. ) ;
#47089 = DIRECTION ( 'NONE',  ( 1.000000000000000000, 0.000000000000000000, 0.000000000000000000 ) ) ;
#47091 = CARTESIAN_POINT ( 'NONE',  ( -41.58131642490323543, -24.51419770103157347, 9.386484678747180510 ) ) ;
#47092 = CARTESIAN_POINT ( 'NONE',  ( 13.91401389203221406, -0.3587747205144265483, 158.0376437107427137 ) ) ;
#47093 = VERTEX_POINT ( 'NONE', #1133 ) ;
#47094 = ORIENTED_EDGE ( 'NONE', *, *, #73265, .T. ) ;
#47095 = CARTESIAN_POINT ( 'NONE',  ( -28.52287095715005805, -24.49960542107631056, 8.947790409070465856 ) ) ;
#47096 = CARTESIAN_POINT ( 'NONE',  ( -77.62287095715005592, -24.50321055353804667, 9.387540953477524042 ) ) ;
#47097 = FACE_OUTER_BOUND ( 'NONE', #93433, .T. ) ;
#47098 = CARTESIAN_POINT ( 'NONE',  ( -14.32918165687622825, -16.72005635474405949, 11.49999999999999645 ) ) ;
#47099 = DIRECTION ( 'NONE',  ( -1.000000000000000000, 0.000000000000000000, 0.000000000000000000 ) ) ;
#47100 = CARTESIAN_POINT ( 'NONE',  ( -3.310667818835141940, 22.29536907041311977, 11.49999999999998934 ) ) ;
#47101 = CARTESIAN_POINT ( 'NONE',  ( -7.324709186033012465, -19.69651249574825513, 11.49999999999998934 ) ) ;
#47102 = DIRECTION ( 'NONE',  ( 0.000000000000000000, -1.000000000000000000, 0.000000000000000000 ) ) ;
#47104 = ORIENTED_EDGE ( 'NONE', *, *, #77018, .T. ) ;
#47103 = CARTESIAN_POINT ( 'NONE',  ( -70.52287095715007581, -29.50250243563736774, 8.947779886222143375 ) ) ;
#47105 = VECTOR ( 'NONE', #99136, 1000.000000000000114 ) ;
#47106 = B_SPLINE_CURVE_WITH_KNOTS ( 'NONE', 3,
 ( #50417, #89967, #74729, #66664, #34193, #81361 ),
 .UNSPECIFIED., .F., .F.,
 ( 4, 2, 4 ),
 ( 0.000000000000000000, 0.001380764517854769953, 0.002761529035709539906 ),
 .UNSPECIFIED. ) ;
#47107 = EDGE_LOOP ( 'NONE', ( #86623, #7590, #93971, #53303 ) ) ;
#47108 = AXIS2_PLACEMENT_3D ( 'NONE', #90120, #28219, #51068 ) ;
#47109 = CARTESIAN_POINT ( 'NONE',  ( -77.62287095715005592, -29.50248528299804818, 1.056150453629038477 ) ) ;
#47110 = AXIS2_PLACEMENT_3D ( 'NONE', #96791, #95791, #11548 ) ;
#47111 = EDGE_CURVE ( 'NONE', #3020, #16367, #63046, .T. ) ;
#47112 = DIRECTION ( 'NONE',  ( 0.000000000000000000, 0.000000000000000000, 1.000000000000000000 ) ) ;
#47113 = ORIENTED_EDGE ( 'NONE', *, *, #25399, .F. ) ;
#47114 = CARTESIAN_POINT ( 'NONE',  ( 10.98566517548414012, -18.08203305749968592, 11.49999999999998934 ) ) ;
#47115 = CARTESIAN_POINT ( 'NONE',  ( -126.6228709571500559, -24.34917612406838927, 0.1852690917426733086 ) ) ;
#47116 = CARTESIAN_POINT ( 'NONE',  ( -51.87944994387085274, -25.03148522597936321, 6.553577993683898484 ) ) ;
#47117 = CARTESIAN_POINT ( 'NONE',  ( -121.5181200719720493, -24.65952944569305316, 1.056160979905709008 ) ) ;
#47118 = DIRECTION ( 'NONE',  ( 0.000000000000000000, 0.9999999999976377785, 2.173523156925979975E-06 ) ) ;
#47119 = CARTESIAN_POINT ( 'NONE',  ( -0.02075734969026423599, 5.965225279485572685, -28.54397719988136828 ) ) ;
#47120 = CARTESIAN_POINT ( 'NONE',  ( -10.57539506955483333, 19.50334513348995813, -1.500000000000002220 ) ) ;
#47121 = FACE_OUTER_BOUND ( 'NONE', #39672, .T. ) ;
#47122 = ORIENTED_EDGE ( 'NONE', *, *, #52101, .T. ) ;
#47123 = CARTESIAN_POINT ( 'NONE',  ( 11.54156857142115911, -5.965225279485592225, -28.05134709678029381 ) ) ;
#47124 = CARTESIAN_POINT ( 'NONE',  ( -37.60901958438072512, -23.73766607897671221, -1.055555164236442023 ) ) ;
#47125 = CARTESIAN_POINT ( 'NONE',  ( -40.45206973576002696, -25.30357236805550158, 5.543059975338419321 ) ) ;
#47126 = CARTESIAN_POINT ( 'NONE',  ( -29.49875734969026198, 5.965225279485572685, 2.362022800118626531 ) ) ;
#47127 = CARTESIAN_POINT ( 'NONE',  ( 3.797776442307698286, -6.376774720514401196, 18.16025641025640525 ) ) ;
#47128 = CARTESIAN_POINT ( 'NONE',  ( 4.201609111248720829, -18.99613120386805676, 11.49999999999998934 ) ) ;
#47129 = CARTESIAN_POINT ( 'NONE',  ( -20.78045986758521835, -5.208592277829342088, 11.49999999999998934 ) ) ;
#47130 = CARTESIAN_POINT ( 'NONE',  ( -62.57945775862675220, -24.65952944569303895, 1.056160979905693686 ) ) ;
#47131 = DIRECTION ( 'NONE',  ( 0.000000000000000000, 0.000000000000000000, 1.000000000000000000 ) ) ;
#47132 = DIRECTION ( 'NONE',  ( 1.000000000000000000, 3.773278334444166432E-23, 8.201307841325785021E-29 ) ) ;
#47133 = CARTESIAN_POINT ( 'NONE',  ( -20.27875734969026311, 7.743225279485574042, 24.00402280011862288 ) ) ;
#47134 = CARTESIAN_POINT ( 'NONE',  ( -14.80616194778269623, -17.16973004002414882, -1.500000000000002220 ) ) ;
#47135 = EDGE_CURVE ( 'NONE', #5380, #80239, #84708, .T. ) ;
#47136 = EDGE_CURVE ( 'NONE', #89504, #88443, #55426, .T. ) ;
#47137 = CARTESIAN_POINT ( 'NONE',  ( -118.5228709571500758, -29.50250243563736774, 8.947779886222134493 ) ) ;
#47138 = PLANE ( 'NONE',  #58981 ) ;
#47139 = CARTESIAN_POINT ( 'NONE',  ( 8.478510716907816658, 17.93336729499101523, 11.49999999999999645 ) ) ;
#47140 = DIRECTION ( 'NONE',  ( -0.000000000000000000, -0.000000000000000000, -1.000000000000000000 ) ) ;
#47141 = CARTESIAN_POINT ( 'NONE',  ( -108.5228709571500616, -23.48786465467241769, 11.44779295918253936 ) ) ;
#47142 = CARTESIAN_POINT ( 'NONE',  ( -50.92287095715006018, -23.47593901973090169, -1.443836447538997980 ) ) ;
#47143 = ORIENTED_EDGE ( 'NONE', *, *, #52231, .F. ) ;
#47144 = CARTESIAN_POINT ( 'NONE',  ( 8.160000000000000142, -10.65233964170348635, 1.628518864987183790 ) ) ;
#47145 = CARTESIAN_POINT ( 'NONE',  ( -80.52287095715004739, -24.51254535375850807, 9.355368624242062836 ) ) ;
#47146 = CARTESIAN_POINT ( 'NONE',  ( -51.60452015029387951, -25.27412385504897685, 3.558372972795847744 ) ) ;
#47147 = CARTESIAN_POINT ( 'NONE',  ( -5.395268184683536639, 21.00466093859614958, 11.49999999999998934 ) ) ;
#47148 = EDGE_CURVE ( 'NONE', #13751, #51301, #12332, .T. ) ;
#47149 = CARTESIAN_POINT ( 'NONE',  ( -124.5895376238167103, -24.64898659630368627, 1.056161002820393158 ) ) ;
#47150 = CARTESIAN_POINT ( 'NONE',  ( 9.746180923669104601, -16.83516941858706417, -1.500000000000002220 ) ) ;
#47151 = EDGE_CURVE ( 'NONE', #22015, #53195, #94654, .T. ) ;
#47152 = CARTESIAN_POINT ( 'NONE',  ( -123.6228709571500701, -24.51387760970725083, 9.387446482453407626 ) ) ;
#47153 = ORIENTED_EDGE ( 'NONE', *, *, #32854, .F. ) ;
#47154 = EDGE_CURVE ( 'NONE', #5356, #29214, #71656, .T. ) ;
#47155 = CARTESIAN_POINT ( 'NONE',  ( -14.79517943714664518, -13.99575967537150412, 11.49999999999999645 ) ) ;
#47156 = CARTESIAN_POINT ( 'NONE',  ( -80.50192592861780838, -24.52300882791530157, 0.6510814631126378149 ) ) ;
#47157 = DIRECTION ( 'NONE',  ( 0.000000000000000000, 0.000000000000000000, -1.000000000000000000 ) ) ;
#47158 = ORIENTED_EDGE ( 'NONE', *, *, #60800, .T. ) ;
#47159 = CARTESIAN_POINT ( 'NONE',  ( -40.45829750704997707, -25.19502912051678223, 3.293943094755625633 ) ) ;
#47160 = CARTESIAN_POINT ( 'NONE',  ( -61.64687923781919920, -25.14083923594766645, 2.947789366383931853 ) ) ;
#47161 = CARTESIAN_POINT ( 'NONE',  ( -40.52319934060825091, -24.92592662359560762, 8.075495903017996469 ) ) ;
#47162 = CARTESIAN_POINT ( 'NONE',  ( -0.9540731552372990754, -6.376774720514411854, 19.74568812963596542 ) ) ;
#47163 = CARTESIAN_POINT ( 'NONE',  ( 17.00595499256408871, 10.69956108467327205, -1.500000000000002220 ) ) ;
#47164 = ADVANCED_FACE ( 'NONE', ( #65062 ), #89366, .T. ) ;
#47165 = DIRECTION ( 'NONE',  ( -1.000000000000000000, 0.000000000000000000, 0.000000000000000000 ) ) ;
#47166 = ORIENTED_EDGE ( 'NONE', *, *, #15465, .T. ) ;
#47167 = DIRECTION ( 'NONE',  ( 0.000000000000000000, 1.000000000000000000, -0.000000000000000000 ) ) ;
#47168 = B_SPLINE_CURVE_WITH_KNOTS ( 'NONE', 3,
 ( #94808, #47152, #70482, #39529, #56276, #63390 ),
 .UNSPECIFIED., .F., .F.,
 ( 4, 2, 4 ),
 ( 1.570887131794333942E-05, 0.001396322306279761073, 0.002776935741241578874 ),
 .UNSPECIFIED. ) ;
#47169 = CIRCLE ( 'NONE', #1827, 2.899999999999999911 ) ;
#47170 = CARTESIAN_POINT ( 'NONE',  ( -13.69284064830502423, 18.33895024417757469, 11.49999999999999645 ) ) ;
#47171 = CARTESIAN_POINT ( 'NONE',  ( 4.564784964189898098, -22.25151590922551748, 11.49999999999998934 ) ) ;
#47172 = VERTEX_POINT ( 'NONE', #80761 ) ;
#47173 = CARTESIAN_POINT ( 'NONE',  ( -71.64150769953161557, -25.20622457644260805, 6.632340821967897426 ) ) ;
#47174 = CARTESIAN_POINT ( 'NONE',  ( -114.5228709571500616, -23.47596703998600631, 11.44779298504228038 ) ) ;
#47175 = FACE_OUTER_BOUND ( 'NONE', #91267, .T. ) ;
#47176 = CARTESIAN_POINT ( 'NONE',  ( -73.55620429048340725, -23.48783264082478084, -1.443836473390067265 ) ) ;
#47177 = EDGE_CURVE ( 'NONE', #88166, #47537, #4136, .T. ) ;
#47178 = CARTESIAN_POINT ( 'NONE',  ( -128.6241757553235345, -23.73791477778912196, 11.05961554403169522 ) ) ;
#47179 = ADVANCED_FACE ( 'NONE', ( #41201 ), #15165, .T. ) ;
#47180 = CARTESIAN_POINT ( 'NONE',  ( -98.89396085167129513, -25.25460717992483950, 6.074556580732870970 ) ) ;
#47181 = ORIENTED_EDGE ( 'NONE', *, *, #75734, .F. ) ;
#47182 = CARTESIAN_POINT ( 'NONE',  ( 20.35419724272142616, 1.316291261081859787, -1.500000000000002220 ) ) ;
#47183 = ORIENTED_EDGE ( 'NONE', *, *, #43781, .F. ) ;
#47184 = CARTESIAN_POINT ( 'NONE',  ( 12.94906671069258763, 19.00495796004926419, -1.500000000000002220 ) ) ;
#47186 = EDGE_CURVE ( 'NONE', #39879, #58273, #41480, .T. ) ;
#47185 = CARTESIAN_POINT ( 'NONE',  ( -7.318926569091948942, -5.876774720514417183, 20.09505574050193033 ) ) ;
#47187 = CARTESIAN_POINT ( 'NONE',  ( 26.73860345374794534, -5.356774720496559894, 3.440769881205036427E-15 ) ) ;
#47188 = VERTEX_POINT ( 'NONE', #60313 ) ;
#47189 = CARTESIAN_POINT ( 'NONE',  ( -108.5964301896317892, -23.48786465467241413, 11.44779295918253759 ) ) ;
#47190 = EDGE_CURVE ( 'NONE', #22003, #67705, #40986, .T. ) ;
#47191 = EDGE_CURVE ( 'NONE', #56219, #90373, #75231, .T. ) ;
#47192 = CARTESIAN_POINT ( 'NONE',  ( 30.93860345374796594, 6.475225279485573360, 19.84760796525321780 ) ) ;
#47194 = ORIENTED_EDGE ( 'NONE', *, *, #72810, .T. ) ;
#47193 = CARTESIAN_POINT ( 'NONE',  ( 5.124585555570928541, 20.71496159572455653, 11.49999999999999645 ) ) ;
#47195 = ORIENTED_EDGE ( 'NONE', *, *, #67363, .T. ) ;
#47196 = CARTESIAN_POINT ( 'NONE',  ( -22.22723998432330106, 0.1330083165726352878, 11.49999999999998934 ) ) ;
#47197 = CARTESIAN_POINT ( 'NONE',  ( -6.358105417860958397, -19.66046682221446318, -1.500000000000002220 ) ) ;
#47198 = ORIENTED_EDGE ( 'NONE', *, *, #13626, .T. ) ;
#47199 = CARTESIAN_POINT ( 'NONE',  ( -4.752075056065355518, -5.876774720514406525, 19.17724329193115551 ) ) ;
#47200 = B_SPLINE_CURVE_WITH_KNOTS ( 'NONE', 3,
 ( #57638, #18555, #95186, #56641, #48526, #49528 ),
 .UNSPECIFIED., .F., .F.,
 ( 4, 2, 4 ),
 ( 0.000000000000000000, 0.001380901958385390930, 0.002761803916770781860 ),
 .UNSPECIFIED. ) ;
#47201 = CARTESIAN_POINT ( 'NONE',  ( -95.50150560350351725, -25.00182538069147142, 7.747789668545043362 ) ) ;
#47202 = ORIENTED_EDGE ( 'NONE', *, *, #89531, .F. ) ;
#47203 = CARTESIAN_POINT ( 'NONE',  ( -51.62287095715006302, -23.73934037231757443, 11.05740245334329153 ) ) ;
#47204 = ORIENTED_EDGE ( 'NONE', *, *, #32369, .T. ) ;
#47205 = CARTESIAN_POINT ( 'NONE',  ( 27.86270917940689174, -0.3587747205144265483, 29.49402280011862487 ) ) ;
#47206 = CARTESIAN_POINT ( 'NONE',  ( -48.52287095715006870, -24.50216790748205042, 0.6166512839542480640 ) ) ;
#47207 = CARTESIAN_POINT ( 'NONE',  ( -15.12424899162716230, 14.39509690008720177, -1.500000000000002220 ) ) ;
#47208 = CARTESIAN_POINT ( 'NONE',  ( -21.69466673205137752, 2.402554924997643226, 11.49999999999999645 ) ) ;
#47209 = CARTESIAN_POINT ( 'NONE',  ( 25.06060784212036907, -5.114160763660862585, -9.130698857930203971 ) ) ;
#47210 = CARTESIAN_POINT ( 'NONE',  ( -99.95716258256356923, -25.04656903514557698, 7.498856445056238051 ) ) ;
#47211 = CARTESIAN_POINT ( 'NONE',  ( 6.846561153812083411, -21.39451737393737574, -1.500000000000002220 ) ) ;
#47212 = CARTESIAN_POINT ( 'NONE',  ( -118.5174234704193310, -24.51419770103160189, 9.386484678747169852 ) ) ;
#47213 = DIRECTION ( 'NONE',  ( -0.1311553622875928082, -6.454799914155188842E-16, -0.9913618264504692190 ) ) ;
#47214 = CARTESIAN_POINT ( 'NONE',  ( -13.36367879947601445, -5.876774720514426953, 20.00000000000000355 ) ) ;
#47215 = VERTEX_POINT ( 'NONE', #72154 ) ;
#47216 = VERTEX_POINT ( 'NONE', #42219 ) ;
#47217 = VECTOR ( 'NONE', #37881, 1000.000000000000114 ) ;
#47218 = VERTEX_POINT ( 'NONE', #93735 ) ;
#47219 = CARTESIAN_POINT ( 'NONE',  ( -15.06583839362908961, -15.15408912208086534, -1.500000000000002220 ) ) ;
#47220 = CARTESIAN_POINT ( 'NONE',  ( -17.59303920844588376, -13.82112144285918731, 11.49999999999999645 ) ) ;
#47221 = ORIENTED_EDGE ( 'NONE', *, *, #22650, .F. ) ;
#47222 = CARTESIAN_POINT ( 'NONE',  ( -8.945158345017247825, -19.07159632999312393, -1.500000000000002220 ) ) ;
#47223 = CARTESIAN_POINT ( 'NONE',  ( -103.6228709571500559, -29.50247984919015209, -1.443849546365050029 ) ) ;
#47224 = CARTESIAN_POINT ( 'NONE',  ( -13.68957358570155769, -14.46295258127404892, -1.500000000000002220 ) ) ;
#47225 = CARTESIAN_POINT ( 'NONE',  ( -6.914873625533459744, 0.3587747205144265483, 29.95171384920748281 ) ) ;
#47226 = B_SPLINE_CURVE_WITH_KNOTS ( 'NONE', 3,
 ( #89224, #50664, #81612, #26821, #58773, #89725, #74489, #36426 ),
 .UNSPECIFIED., .F., .F.,
 ( 4, 2, 2, 4 ),
 ( -0.001240666984356068306, -0.0002401179793396698847, 0.0007604310256767281024, 0.002761529035709520824 ),
 .UNSPECIFIED. ) ;
#47227 = CARTESIAN_POINT ( 'NONE',  ( -49.96215261998537471, -25.05234313451448713, 7.519799490366015249 ) ) ;
#47228 = CARTESIAN_POINT ( 'NONE',  ( -15.01370250125036421, 16.05796621403891677, -1.500000000000002220 ) ) ;
#47229 = DIRECTION ( 'NONE',  ( 0.000000000000000000, -0.000000000000000000, -1.000000000000000000 ) ) ;
#47230 = VERTEX_POINT ( 'NONE', #31343 ) ;
#47231 = DIRECTION ( 'NONE',  ( -3.773278334444166432E-23, 1.000000000000000000, 0.000000000000000000 ) ) ;
#47232 = DIRECTION ( 'NONE',  ( 0.000000000000000000, -0.9999999999976377785, -2.173523156925979128E-06 ) ) ;
#47233 = CARTESIAN_POINT ( 'NONE',  ( -17.17656601037699104, 11.78060583124977256, 11.49999999999999645 ) ) ;
#47234 = CARTESIAN_POINT ( 'NONE',  ( -74.52287095715007581, -24.65952944569304606, 1.056160979905697239 ) ) ;
#47235 = VECTOR ( 'NONE', #44268, 1000.000000000000114 ) ;
#47236 = CARTESIAN_POINT ( 'NONE',  ( 33.12653832968932477, 5.965225279485572685, -7.315055336576597789 ) ) ;
#47237 = PRODUCT_DEFINITION_FORMATION_WITH_SPECIFIED_SOURCE ( 'ANY', '', #28832, .NOT_KNOWN. ) ;
#47238 = CARTESIAN_POINT ( 'NONE',  ( 29.73860345376316872, -5.356774720514427379, 17.30421508979847189 ) ) ;
#47239 = CARTESIAN_POINT ( 'NONE',  ( -10.68834330497911189, 18.46263264838738039, 11.49999999999998934 ) ) ;
#47240 = DIRECTION ( 'NONE',  ( 3.469446951953611033E-15, 1.000000000000000000, 0.000000000000000000 ) ) ;
#47241 = CARTESIAN_POINT ( 'NONE',  ( -51.16008406385073926, -25.23528994651498891, 3.604084673499913904 ) ) ;
#47242 = DIRECTION ( 'NONE',  ( 0.000000000000000000, 0.9999999999976377785, 2.173523156925979128E-06 ) ) ;
#47243 = CARTESIAN_POINT ( 'NONE',  ( -69.33173068595476707, -25.22594453560301631, 6.517383687127669134 ) ) ;
#47244 = CARTESIAN_POINT ( 'NONE',  ( 21.70358988458699301, 5.938112137899119070, -1.500000000000002220 ) ) ;
#47245 = EDGE_CURVE ( 'NONE', #58299, #3436, #72737, .T. ) ;
#47246 = FACE_OUTER_BOUND ( 'NONE', #52096, .T. ) ;
#47247 = VERTEX_POINT ( 'NONE', #54694 ) ;
#47248 = EDGE_CURVE ( 'NONE', #51956, #35854, #96985, .T. ) ;
#47249 = FACE_OUTER_BOUND ( 'NONE', #53249, .T. ) ;
#47250 = CARTESIAN_POINT ( 'NONE',  ( 2.905472630834636139, -5.876774720514415407, 19.87563926270137671 ) ) ;
#47251 = CARTESIAN_POINT ( 'NONE',  ( -17.62174901100306101, -8.731699659924187173, 11.49999999999999645 ) ) ;
#47252 = DIRECTION ( 'NONE',  ( -1.457939797397921811E-16, 0.1087265912856345829, -0.9940716917543757081 ) ) ;
#47253 = FACE_OUTER_BOUND ( 'NONE', #1683, .T. ) ;
#47254 = ORIENTED_EDGE ( 'NONE', *, *, #42845, .F. ) ;
#47255 = ADVANCED_FACE ( 'NONE', ( #99346 ), #53248, .T. ) ;
#47256 = CARTESIAN_POINT ( 'NONE',  ( 29.57907552799941087, -5.965225279485572685, 29.21818156447043791 ) ) ;
#47257 = CARTESIAN_POINT ( 'NONE',  ( -39.58953762381673158, -24.65952944569304606, 1.056160979905693686 ) ) ;
#47258 = CARTESIAN_POINT ( 'NONE',  ( -100.4277023991755442, -25.25095780761413522, 5.215800478967231868 ) ) ;
#47259 = EDGE_CURVE ( 'NONE', #75060, #23364, #55202, .T. ) ;
#47260 = EDGE_CURVE ( 'NONE', #58493, #71422, #7504, .T. ) ;
#47261 = PLANE ( 'NONE',  #33474 ) ;
#47262 = CARTESIAN_POINT ( 'NONE',  ( 3.553741186906278493, -19.43417129498564577, 11.49999999999998934 ) ) ;
#47263 = VERTEX_POINT ( 'NONE', #45085 ) ;
#47264 = EDGE_CURVE ( 'NONE', #12032, #59480, #21838, .T. ) ;
#47265 = CARTESIAN_POINT ( 'NONE',  ( 9.777643287007670381, 6.376774720514424288, -24.98776412748719977 ) ) ;
#47266 = AXIS2_PLACEMENT_3D ( 'NONE', #88288, #3554, #11646 ) ;
#47267 = ITEM_DEFINED_TRANSFORMATION ( 'NONE', 'NONE', #84451,  #37391 ) ;
#47268 = EDGE_LOOP ( 'NONE', ( #86112, #61230, #87486, #40494 ) ) ;
#47269 = DIRECTION ( 'NONE',  ( -1.000000000000000000, 0.000000000000000000, 0.000000000000000000 ) ) ;
#47270 = PLANE ( 'NONE',  #92826 ) ;
#47271 = DIRECTION ( 'NONE',  ( -0.000000000000000000, 1.000000000000000000, -0.000000000000000000 ) ) ;
#47272 = CARTESIAN_POINT ( 'NONE',  ( 32.04341656622251122, -4.806217029847265287, -4.198923130344409671 ) ) ;
#47273 = CARTESIAN_POINT ( 'NONE',  ( -1.653359744423585465, -5.876774720514413630, 19.34586827028017098 ) ) ;
#47274 = CARTESIAN_POINT ( 'NONE',  ( -67.58953762381672448, -24.64965694238407323, 8.947790433994653014 ) ) ;
#47275 = CARTESIAN_POINT ( 'NONE',  ( -107.6235340116869423, -24.65952944569304606, 1.056160979905704789 ) ) ;
#47276 = CARTESIAN_POINT ( 'NONE',  ( 1.468936567494551593, -19.95401460376903913, 11.49999999999998934 ) ) ;
#47277 = B_SPLINE_CURVE_WITH_KNOTS ( 'NONE', 3,
 ( #39011, #15676, #78558, #77561 ),
 .UNSPECIFIED., .F., .F.,
 ( 4, 4 ),
 ( 0.000000000000000000, 0.002085937500000023537 ),
 .UNSPECIFIED. ) ;
#47278 = EDGE_CURVE ( 'NONE', #62379, #72159, #21682, .T. ) ;
#47279 = CARTESIAN_POINT ( 'NONE',  ( -99.77116551335946326, -25.10935072017632308, 2.990445978756222978 ) ) ;
#47280 = CARTESIAN_POINT ( 'NONE',  ( -116.5876139491709154, -24.66019654487199730, 8.947790411086115725 ) ) ;
#47281 = ORIENTED_EDGE ( 'NONE', *, *, #15169, .T. ) ;
#47282 = ADVANCED_FACE ( 'NONE', ( #100328 ), #31398, .T. ) ;
#47283 = CARTESIAN_POINT ( 'NONE',  ( -79.58490835860241930, -24.51419770103157347, 9.386484678747176957 ) ) ;
#47284 = CARTESIAN_POINT ( 'NONE',  ( -110.3009842343709721, -25.29012725628788516, 3.294836594238610417 ) ) ;
#47285 = CARTESIAN_POINT ( 'NONE',  ( -65.62287095715005592, -29.50248789122583659, 2.256150453626215580 ) ) ;
#47286 = LINE ( 'NONE', #78213, #6260 ) ;
#47287 = VECTOR ( 'NONE', #6328, 1000.000000000000000 ) ;
#47288 = FACE_OUTER_BOUND ( 'NONE', #20969, .T. ) ;
#47289 = DIRECTION ( 'NONE',  ( 0.000000000000000000, 0.9999999999976377785, 2.173523156925979128E-06 ) ) ;
#47290 = ADVANCED_FACE ( 'NONE', ( #71925 ), #86132, .T. ) ;
#47291 = PLANE ( 'NONE',  #57667 ) ;
#47292 = CARTESIAN_POINT ( 'NONE',  ( -36.52287095715006870, -24.64965694238407323, 8.947790433994205372 ) ) ;
#47293 = ORIENTED_EDGE ( 'NONE', *, *, #91347, .F. ) ;
#47294 = CARTESIAN_POINT ( 'NONE',  ( -11.07518157712430096, -17.02944518001645946, 11.49999999999998934 ) ) ;
#47295 = PLANE ( 'NONE',  #80923 ) ;
#47296 = CARTESIAN_POINT ( 'NONE',  ( -88.58953762381671027, -23.48786465467241769, 11.44779295918254114 ) ) ;
#47298 = EDGE_LOOP ( 'NONE', ( #43110, #66205, #90887, #94341 ) ) ;
#47297 = ADVANCED_FACE ( 'NONE', ( #34354 ), #64330, .F. ) ;
#47299 = DIRECTION ( 'NONE',  ( -1.000000000000000000, -3.773278334444167608E-23, -8.201307833595939069E-29 ) ) ;
#47300 = CIRCLE ( 'NONE', #16429, 1.000000000000000000 ) ;
#47301 = CARTESIAN_POINT ( 'NONE',  ( 19.31759285448427477, -5.727529672960866236, -1.500000000000002220 ) ) ;
#47302 = CARTESIAN_POINT ( 'NONE',  ( 17.87031378931267867, -11.31994873005049129, 11.49999999999999645 ) ) ;
#47303 = LOCAL_TIME ( 0, 54, 15.00000000000000000, #28045 ) ;
#47304 = CARTESIAN_POINT ( 'NONE',  ( 21.80885565983754404, 3.581153529568561478, -1.500000000000002220 ) ) ;
#47305 = EDGE_CURVE ( 'NONE', #68548, #95766, #46137, .T. ) ;
#47306 = CARTESIAN_POINT ( 'NONE',  ( -17.20787902393383462, -11.26661214947554157, 11.49999999999998934 ) ) ;
#47307 = CARTESIAN_POINT ( 'NONE',  ( -60.62821588322990607, -24.83618233451449697, 1.606449574219536380 ) ) ;
#47308 = ORIENTED_EDGE ( 'NONE', *, *, #1754, .F. ) ;
#47309 = CARTESIAN_POINT ( 'NONE',  ( -88.52287095715006160, -23.47596703998600631, 11.44779298504228393 ) ) ;
#47310 = ORIENTED_EDGE ( 'NONE', *, *, #75938, .T. ) ;
#47311 = CARTESIAN_POINT ( 'NONE',  ( -29.49875734969025842, -0.3587747205144265483, 25.61802280011862720 ) ) ;
#47312 = CARTESIAN_POINT ( 'NONE',  ( -61.62287095715007013, -23.73934037231757088, 11.05740245334329330 ) ) ;
#47313 = VERTEX_POINT ( 'NONE', #26736 ) ;
#47314 = VERTEX_POINT ( 'NONE', #17116 ) ;
#47315 = VERTEX_POINT ( 'NONE', #3419 ) ;
#47316 = PLANE ( 'NONE',  #31057 ) ;
#47317 = CARTESIAN_POINT ( 'NONE',  ( 7.010993867624484288, -6.376774720514417183, 20.34381700913260715 ) ) ;
#47318 = CARTESIAN_POINT ( 'NONE',  ( -68.49379447780960106, -24.66019654487199375, 8.947790411086122830 ) ) ;
#47319 = CARTESIAN_POINT ( 'NONE',  ( 7.614520588612671226, -19.20288753073135268, -1.500000000000002220 ) ) ;
#47320 = EDGE_CURVE ( 'NONE', #85117, #14223, #94740, .T. ) ;
#47321 = B_SPLINE_CURVE_WITH_KNOTS ( 'NONE', 3,
 ( #67994, #76081, #45158, #14181 ),
 .UNSPECIFIED., .F., .F.,
 ( 4, 4 ),
 ( 0.000000000000000000, 9.999999999998897304E-05 ),
 .UNSPECIFIED. ) ;
#47322 = CARTESIAN_POINT ( 'NONE',  ( -21.46818342838279392, -2.986162219498790904, 11.49999999999999645 ) ) ;
#47323 = ORIENTED_EDGE ( 'NONE', *, *, #77456, .T. ) ;
#47324 = CARTESIAN_POINT ( 'NONE',  ( -37.62287095715005592, -29.50248528299804818, 1.056150453629031594 ) ) ;
#47325 = FACE_OUTER_BOUND ( 'NONE', #4910, .T. ) ;
#47326 = CARTESIAN_POINT ( 'NONE',  ( -1.986123035288760885, 22.30159847666916662, 11.49999999999998934 ) ) ;
#47327 = CARTESIAN_POINT ( 'NONE',  ( -47.57718451496743484, -24.66019654487199730, 8.947790411086117501 ) ) ;
#47328 = CARTESIAN_POINT ( 'NONE',  ( -120.6228709571500417, -24.99156045073393528, 7.747789690856161648 ) ) ;
#47329 = ORIENTED_EDGE ( 'NONE', *, *, #96413, .T. ) ;
#47330 = CARTESIAN_POINT ( 'NONE',  ( -116.7734038585102354, -25.37178273948851626, 5.922773836801656699 ) ) ;
#47331 = CARTESIAN_POINT ( 'NONE',  ( -35.62710583289069177, -23.48786465467240703, 11.44779295918255180 ) ) ;
#47332 = VERTEX_POINT ( 'NONE', #25734 ) ;
#47333 = B_SPLINE_CURVE_WITH_KNOTS ( 'NONE', 3,
 ( #59895, #27931, #73611, #58398 ),
 .UNSPECIFIED., .F., .F.,
 ( 4, 4 ),
 ( 0.000000000000000000, 9.999999999998897304E-05 ),
 .UNSPECIFIED. ) ;
#47334 = DIRECTION ( 'NONE',  ( -1.000000000000000000, 0.000000000000000000, 0.000000000000000000 ) ) ;
#47335 = ORIENTED_EDGE ( 'NONE', *, *, #21830, .T. ) ;
#47336 = VECTOR ( 'NONE', #55232, 1000.000000000000000 ) ;
#47337 = CARTESIAN_POINT ( 'NONE',  ( -109.6260462722971454, -24.35071581493543746, 9.817618358456025263 ) ) ;
#47338 = CARTESIAN_POINT ( 'NONE',  ( 20.71511372717374755, 4.256074106246791722, -1.500000000000002220 ) ) ;
#47339 = ORIENTED_EDGE ( 'NONE', *, *, #40743, .T. ) ;
#47340 = CARTESIAN_POINT ( 'NONE',  ( -50.56030698869226114, -23.85016227208580020, -0.8807180028928345283 ) ) ;
#47341 = CARTESIAN_POINT ( 'NONE',  ( -20.57666286913221754, 7.287794730890116313, -1.500000000000002220 ) ) ;
#47342 = CARTESIAN_POINT ( 'NONE',  ( -38.52287095715006870, -23.47596703998600631, 11.44779298504229281 ) ) ;
#47343 = DIRECTION ( 'NONE',  ( 0.000000000000000000, 0.000000000000000000, -1.000000000000000000 ) ) ;
#47344 = CARTESIAN_POINT ( 'NONE',  ( 30.32108885906865936, 4.540774720514427543, 3.274824222184972822 ) ) ;
#47345 = CARTESIAN_POINT ( 'NONE',  ( -12.45635911906152771, -17.91357634596933934, -1.500000000000002220 ) ) ;
#47346 = CYLINDRICAL_SURFACE ( 'NONE', #31755, 2.399999999999999911 ) ;
#47347 = ORIENTED_EDGE ( 'NONE', *, *, #73163, .F. ) ;
#47348 = DIRECTION ( 'NONE',  ( 0.000000000000000000, -0.9999999999976377785, -2.173523156925979128E-06 ) ) ;
#47349 = CARTESIAN_POINT ( 'NONE',  ( -85.63839554153061329, -24.15602025860895807, 10.28564288303535967 ) ) ;
#47350 = EDGE_LOOP ( 'NONE', ( #57424, #83637, #94751, #1563 ) ) ;
#47351 = ORIENTED_EDGE ( 'NONE', *, *, #6847, .F. ) ;
#47352 = ORIENTED_EDGE ( 'NONE', *, *, #77012, .F. ) ;
#47353 = AXIS2_PLACEMENT_3D ( 'NONE', #29660, #74832, #51018 ) ;
#47354 = CARTESIAN_POINT ( 'NONE',  ( -58.62287095715004881, -24.64965695001468404, 8.947790433994185832 ) ) ;
#47355 = CARTESIAN_POINT ( 'NONE',  ( 8.071512145086533252, -9.528487854913509025, -6.499999999999998224 ) ) ;
#47356 = CARTESIAN_POINT ( 'NONE',  ( -6.410030533929251817, 20.24415959294862333, -1.500000000000002220 ) ) ;
#47357 = CIRCLE ( 'NONE', #78115, 0.8159999999999660858 ) ;
#47358 = CARTESIAN_POINT ( 'NONE',  ( -94.50778353013456012, -24.51314013834316086, 0.6176544820404165081 ) ) ;
#47359 = CARTESIAN_POINT ( 'NONE',  ( -79.14729083585920932, -25.27791806053743073, 6.795304352983273510 ) ) ;
#47360 = DIRECTION ( 'NONE',  ( -3.773278334453079030E-23, 0.9999999999976377785, 2.173523156925979128E-06 ) ) ;
#47361 = DIRECTION ( 'NONE',  ( -3.773278334453079030E-23, 0.9999999999976377785, 2.173523156925979128E-06 ) ) ;
#47362 = CARTESIAN_POINT ( 'NONE',  ( 8.665315094346039970, 17.34094453737590769, 11.49999999999998934 ) ) ;
#47363 = EDGE_CURVE ( 'NONE', #56601, #89282, #28078, .T. ) ;
#47364 = CARTESIAN_POINT ( 'NONE',  ( -39.02714944717881451, -25.25978494880519776, 3.590542803917028181 ) ) ;
#47365 = ORIENTED_EDGE ( 'NONE', *, *, #84579, .T. ) ;
#47366 = EDGE_CURVE ( 'NONE', #86594, #38515, #81176, .T. ) ;
#47367 = CARTESIAN_POINT ( 'NONE',  ( -17.64752530894654470, 8.349842952099315596, 11.49999999999999645 ) ) ;
#47368 = CARTESIAN_POINT ( 'NONE',  ( 5.395440699609677537, 5.965225279485594001, -28.51842087987364138 ) ) ;
#47369 = EDGE_CURVE ( 'NONE', #96261, #59330, #40019, .T. ) ;
#47370 = CARTESIAN_POINT ( 'NONE',  ( -91.94687923781920347, -29.50249691823240994, 6.409318347766594037 ) ) ;
#47371 = ORIENTED_EDGE ( 'NONE', *, *, #37326, .T. ) ;
#47372 = EDGE_CURVE ( 'NONE', #53534, #17650, #73993, .T. ) ;
#47373 = CARTESIAN_POINT ( 'NONE',  ( -98.55620429048339304, -24.66019654487199730, 8.947790411086124607 ) ) ;
#47374 = DIRECTION ( 'NONE',  ( -0.06975647374412548285, -0.9975640502598241977, 0.000000000000000000 ) ) ;
#47375 = EDGE_CURVE ( 'NONE', #15961, #82260, #63828, .T. ) ;
#47376 = CARTESIAN_POINT ( 'NONE',  ( -106.5228709571500332, -23.94994826722564696, -0.6494450866342710293 ) ) ;
#47377 = VECTOR ( 'NONE', #67627, 1000.000000000000000 ) ;
#47378 = CARTESIAN_POINT ( 'NONE',  ( -34.58953762381672448, -23.48786465467240347, 11.44779295918255535 ) ) ;
#47379 = CARTESIAN_POINT ( 'NONE',  ( 16.91694316922610497, -9.995573847407506207, -1.500000000000002220 ) ) ;
#47380 = LINE ( 'NONE', #694, #83350 ) ;
#47382 = ORIENTED_EDGE ( 'NONE', *, *, #7474, .T. ) ;
#47381 = APPROVAL_PERSON_ORGANIZATION ( #37144, #82835, #29523 ) ;
#47383 = CARTESIAN_POINT ( 'NONE',  ( 21.36531308999010648, 3.172564587314818052, 11.49999999999998934 ) ) ;
#47384 = CARTESIAN_POINT ( 'NONE',  ( -40.52987890412448024, -24.73486907724917927, 1.287355809206960577 ) ) ;
#47385 = PLANE ( 'NONE',  #6660 ) ;
#47386 = CARTESIAN_POINT ( 'NONE',  ( -23.05830607064937965, -0.9945063503333604338, -1.500000000000002220 ) ) ;
#47387 = CALENDAR_DATE ( 2026, 9, 10 ) ;
#47388 = CARTESIAN_POINT ( 'NONE',  ( -121.6228709571500417, -29.50247984919015209, -1.443849546365046699 ) ) ;
#47389 = CARTESIAN_POINT ( 'NONE',  ( -90.52287095715006160, -24.91570333825770334, 8.075032458260366752 ) ) ;
#47390 = CARTESIAN_POINT ( 'NONE',  ( -121.5543276637445018, -24.35071581493543746, 9.817618358456025263 ) ) ;
#47391 = DIRECTION ( 'NONE',  ( -0.000000000000000000, 2.173523156925979552E-06, -0.9999999999976378895 ) ) ;
#47392 = CARTESIAN_POINT ( 'NONE',  ( -111.7814946224345789, -25.29824137189153532, 4.332404408885398794 ) ) ;
#47393 = CARTESIAN_POINT ( 'NONE',  ( -129.5558065563047876, -24.34968618360934300, 0.1864209137778921610 ) ) ;
#47394 = VECTOR ( 'NONE', #10892, 1000.000000000000114 ) ;
#47395 = B_SPLINE_CURVE_WITH_KNOTS ( 'NONE', 3,
 ( #34705, #36202, #66178, #5244 ),
 .UNSPECIFIED., .F., .F.,
 ( 4, 4 ),
 ( 0.3390065795743660848, 0.3400073266151316109 ),
 .UNSPECIFIED. ) ;
#47396 = CARTESIAN_POINT ( 'NONE',  ( -49.58953762381673158, -23.47593901973091235, -1.443836447539009749 ) ) ;
#47397 = CARTESIAN_POINT ( 'NONE',  ( -16.79965634883036074, 10.71410036745690597, -1.500000000000002220 ) ) ;
#47398 = CYLINDRICAL_SURFACE ( 'NONE', #63040, 1.249999999999997558 ) ;
#47399 = CARTESIAN_POINT ( 'NONE',  ( 13.99221305778824487, -14.08248706038611964, -1.500000000000002220 ) ) ;
#47400 = CARTESIAN_POINT ( 'NONE',  ( -23.59123376470063960, 6.143225279485574397, 24.50402280011862288 ) ) ;
#47401 = DIRECTION ( 'NONE',  ( -0.000000000000000000, 1.000000000000000000, -0.000000000000000000 ) ) ;
#47402 = CARTESIAN_POINT ( 'NONE',  ( -35.62287095715006302, -24.51254535404254398, 9.355368623467647637 ) ) ;
#47403 = CARTESIAN_POINT ( 'NONE',  ( -3.546427018491999483, -20.45703643143680850, 11.49999999999999645 ) ) ;
#47404 = LINE ( 'NONE', #63139, #67849 ) ;
#47405 = CARTESIAN_POINT ( 'NONE',  ( -106.5112401517874190, -24.65952944569304961, 1.056160979905703456 ) ) ;
#47406 = CARTESIAN_POINT ( 'NONE',  ( -21.69093436787670726, -6.948586514802197023, 11.49999999999999645 ) ) ;
#47407 = VECTOR ( 'NONE', #40386, 1000.000000000000000 ) ;
#47408 = ORIENTED_EDGE ( 'NONE', *, *, #89855, .T. ) ;
#47409 = B_SPLINE_SURFACE_WITH_KNOTS ( 'NONE', 3, 1, ( 
 ( #72814, #65716 ),
 ( #89032, #4296 ),
 ( #49986, #26634 ),
 ( #74299, #90025 ),
 ( #81912, #81417 ),
 ( #43363, #34248 ),
 ( #80913, #20497 ),
 ( #74784, #28131 ),
 ( #3317, #50975 ),
 ( #10907, #65223 ),
 ( #4791, #96629 ),
 ( #96147, #57098 ),
 ( #80413, #88035 ),
 ( #27132, #42867 ),
 ( #27636, #11404 ) ),
 .UNSPECIFIED., .F., .F., .F.,
 ( 4, 1, 1, 1, 1, 1, 1, 1, 1, 1, 1, 1, 4 ),
 ( 2, 2 ),
 ( 0.000000000000000000, 0.09468725186755398704, 0.1819941557072748128, 0.2643769486105100874, 0.3421798619477735559, 0.4186176108621474934, 0.4965090753719113015, 0.5773690916117304450, 0.6615105924541956339, 0.7467325508291923208, 0.8312579843277431157, 0.9152056162136544826, 1.000000000000000000 ),
 ( 0.000000000000000000, 1.000000000000000000 ),
 .UNSPECIFIED. ) ;
#47410 = CARTESIAN_POINT ( 'NONE',  ( -83.62287095715007013, -24.66019654487199730, 8.947790411086126383 ) ) ;
#47411 = CARTESIAN_POINT ( 'NONE',  ( -106.6228709571500559, -23.47593901973091235, -1.443836447538999312 ) ) ;
#47412 = ORIENTED_EDGE ( 'NONE', *, *, #24395, .T. ) ;
#47413 = B_SPLINE_CURVE_WITH_KNOTS ( 'NONE', 3,
 ( #74119, #11706, #20309, #35062, #90336, #58896 ),
 .UNSPECIFIED., .F., .F.,
 ( 4, 2, 4 ),
 ( 0.000000000000000000, 0.001380764517854769519, 0.002761529035709539039 ),
 .UNSPECIFIED. ) ;
#47414 = CARTESIAN_POINT ( 'NONE',  ( -16.64171244834553676, 11.49637152377623828, 11.49999999999998934 ) ) ;
#47415 = CARTESIAN_POINT ( 'NONE',  ( -77.52287095715006160, -23.48786465467241058, 11.44779295918254469 ) ) ;
#47416 = CARTESIAN_POINT ( 'NONE',  ( -97.62287095714999907, -24.33927499327854704, 9.819080762295818943 ) ) ;
#47417 = ORIENTED_EDGE ( 'NONE', *, *, #12453, .F. ) ;
#47418 = CARTESIAN_POINT ( 'NONE',  ( -70.62287095715004170, -24.14406661707768009, 10.28769366152058673 ) ) ;
#47419 = CARTESIAN_POINT ( 'NONE',  ( -22.88579126497628025, -1.409509213828211927, 11.49999999999998934 ) ) ;
#47420 = CARTESIAN_POINT ( 'NONE',  ( -40.80373042471702405, -25.12778184171447649, 2.872918476217471540 ) ) ;
#47421 = CARTESIAN_POINT ( 'NONE',  ( -4.285004571687458963, -21.18589511591401831, -1.500000000000002220 ) ) ;
#47422 = DIRECTION ( 'NONE',  ( 3.773278334444166432E-23, -1.000000000000000000, 0.000000000000000000 ) ) ;
#47423 = AXIS2_PLACEMENT_3D ( 'NONE', #32778, #63758, #47009 ) ;
#47424 = CARTESIAN_POINT ( 'NONE',  ( -2.499008156623981236, -20.81284420272260860, 11.49999999999999645 ) ) ;
#47425 = ORIENTED_EDGE ( 'NONE', *, *, #46940, .F. ) ;
#47426 = CARTESIAN_POINT ( 'NONE',  ( -73.58953762381672448, -23.48786465467241058, 11.44779295918254469 ) ) ;
#47427 = CARTESIAN_POINT ( 'NONE',  ( -69.23586867255411903, -25.31612525200183228, 5.333582893051659113 ) ) ;
#47428 = CARTESIAN_POINT ( 'NONE',  ( 4.628415685485613551, -21.52068878818806752, -1.500000000000002220 ) ) ;
#47429 = EDGE_CURVE ( 'NONE', #1915, #26773, #60707, .T. ) ;
#47430 = DIRECTION ( 'NONE',  ( 1.000000000000000000, 0.000000000000000000, 0.000000000000000000 ) ) ;
#47431 = EDGE_LOOP ( 'NONE', ( #79113, #92635, #5130, #61040 ) ) ;
#47432 = CARTESIAN_POINT ( 'NONE',  ( -49.86550021440504565, -25.27344785826827689, 3.414711230909520001 ) ) ;
#47433 = ADVANCED_FACE ( 'NONE', ( #89633 ), #81025, .F. ) ;
#47434 = CARTESIAN_POINT ( 'NONE',  ( -122.6228709571500417, -24.64965695001469115, 8.947790433994175174 ) ) ;
#47435 = ORIENTED_EDGE ( 'NONE', *, *, #58645, .F. ) ;
#47436 = CARTESIAN_POINT ( 'NONE',  ( -86.62287095715004170, -29.50248528299804818, 1.056150453629040253 ) ) ;
#47437 = VERTEX_POINT ( 'NONE', #12993 ) ;
#47438 = ORIENTED_EDGE ( 'NONE', *, *, #53662, .F. ) ;
#47439 = DIRECTION ( 'NONE',  ( 0.000000000000000000, 0.000000000000000000, 1.000000000000000000 ) ) ;
#47440 = CARTESIAN_POINT ( 'NONE',  ( -71.62287095715005592, -23.47596703998600631, 11.44779298504227683 ) ) ;
#47441 = CARTESIAN_POINT ( 'NONE',  ( -25.92875734969026524, -5.356774720514425603, 0.7300228001186309656 ) ) ;
#47442 = CARTESIAN_POINT ( 'NONE',  ( -19.82921842031888104, 5.099586017421429140, -1.500000000000002220 ) ) ;
#47443 = ORIENTED_EDGE ( 'NONE', *, *, #90736, .T. ) ;
#47444 = CARTESIAN_POINT ( 'NONE',  ( -99.30054463691881494, -25.25874007465087701, 6.071601063123229558 ) ) ;
#47445 = CARTESIAN_POINT ( 'NONE',  ( -44.65451812762749739, -23.73766607897669800, -1.055555164236458898 ) ) ;
#47446 = FACE_OUTER_BOUND ( 'NONE', #44691, .T. ) ;
#47447 = CARTESIAN_POINT ( 'NONE',  ( -3.941980378682776287, 21.93750326593198352, 11.49999999999998934 ) ) ;
#47449 = CARTESIAN_POINT ( 'NONE',  ( -70.32380231474228083, -25.13313949306887096, 7.101635536975467566 ) ) ;
#47448 = VECTOR ( 'NONE', #50999, 1000.000000000000114 ) ;
#47450 = FACE_OUTER_BOUND ( 'NONE', #38130, .T. ) ;
#47451 = ORIENTED_EDGE ( 'NONE', *, *, #29663, .T. ) ;
#47452 = CARTESIAN_POINT ( 'NONE',  ( -29.68686754081408807, -25.14195210743483955, 3.478271856783234917 ) ) ;
#47453 = DIRECTION ( 'NONE',  ( -0.1311553622875919756, -6.845827386180409975E-16, -0.9913618264504692190 ) ) ;
#47454 = CC_DESIGN_SECURITY_CLASSIFICATION ( #92779, ( #91188 ) ) ;
#47455 = CARTESIAN_POINT ( 'NONE',  ( -19.40898059523135544, 7.551958013340856368, -1.500000000000002220 ) ) ;
#47456 = VERTEX_POINT ( 'NONE', #98733 ) ;
#47458 = ORIENTED_EDGE ( 'NONE', *, *, #64010, .T. ) ;
#47457 = DIRECTION ( 'NONE',  ( 3.773278334444167608E-23, -1.000000000000000000, 0.000000000000000000 ) ) ;
#47459 = VERTEX_POINT ( 'NONE', #44465 ) ;
#47460 = AXIS2_PLACEMENT_3D ( 'NONE', #28406, #13176, #14175 ) ;
#47461 = CARTESIAN_POINT ( 'NONE',  ( -50.71600500446225368, -25.25854563549779641, 7.074608752973259307 ) ) ;
#47462 = CARTESIAN_POINT ( 'NONE',  ( -18.19455084753484542, -10.52586660885228298, -1.500000000000002220 ) ) ;
#47463 = VERTEX_POINT ( 'NONE', #50085 ) ;
#47464 = CARTESIAN_POINT ( 'NONE',  ( -118.5228709571500900, -23.72773821059536914, 11.05748984161097326 ) ) ;
#47465 = DIRECTION ( 'NONE',  ( -1.286817348990133655E-16, 0.000000000000000000, 1.000000000000000000 ) ) ;
#47466 = DIRECTION ( 'NONE',  ( -0.000000000000000000, -1.000000000000000000, -0.000000000000000000 ) ) ;
#47467 = AXIS2_PLACEMENT_3D ( 'NONE', #97249, #27741, #52079 ) ;
#47468 = CARTESIAN_POINT ( 'NONE',  ( -86.62359152838003240, -24.66019654487200086, 8.947790411086115725 ) ) ;
#47469 = CARTESIAN_POINT ( 'NONE',  ( -60.62287095715004881, -23.47596703998600631, 11.44779298504227505 ) ) ;
#47470 = CARTESIAN_POINT ( 'NONE',  ( -65.62287095714999907, -24.63345952396255356, 9.038047939301506517 ) ) ;
#47472 = ORIENTED_EDGE ( 'NONE', *, *, #15243, .T. ) ;
#47471 = CARTESIAN_POINT ( 'NONE',  ( 4.265775719338400052, 21.77767432286298543, 11.49999999999999645 ) ) ;
#47473 = CARTESIAN_POINT ( 'NONE',  ( -89.06226385320383088, -25.26877915520014994, 5.947789088310639904 ) ) ;
#47474 = DIRECTION ( 'NONE',  ( 7.994117400814786717E-16, 0.000000000000000000, -1.000000000000000000 ) ) ;
#47475 = ORIENTED_EDGE ( 'NONE', *, *, #10843, .T. ) ;
#47476 = CARTESIAN_POINT ( 'NONE',  ( -19.66899025692886838, 11.29834648773183581, 11.49999999999998934 ) ) ;
#47477 = EDGE_CURVE ( 'NONE', #69684, #37312, #27975, .T. ) ;
#47479 = ORIENTED_EDGE ( 'NONE', *, *, #72374, .T. ) ;
#47478 = DIRECTION ( 'NONE',  ( 0.000000000000000000, 0.000000000000000000, -1.000000000000000000 ) ) ;
#47480 = VERTEX_POINT ( 'NONE', #97245 ) ;
#47481 = CARTESIAN_POINT ( 'NONE',  ( -68.52287095715006160, -23.47596703998600631, 11.44779298504228748 ) ) ;
#47482 = CARTESIAN_POINT ( 'NONE',  ( -11.96439459519798554, -16.23097265130270728, 11.49999999999998934 ) ) ;
#47483 = PLANE ( 'NONE',  #97589 ) ;
#47484 = VERTEX_POINT ( 'NONE', #35845 ) ;
#47485 = EDGE_CURVE ( 'NONE', #20674, #39577, #59190, .T. ) ;
#47486 = DIRECTION ( 'NONE',  ( 0.000000000000000000, 0.000000000000000000, -1.000000000000000000 ) ) ;
#47487 = CARTESIAN_POINT ( 'NONE',  ( 19.55810785529653373, 10.91776788121007868, -1.500000000000002220 ) ) ;
#47488 = ORIENTED_EDGE ( 'NONE', *, *, #63658, .F. ) ;
#47489 = ORIENTED_EDGE ( 'NONE', *, *, #36830, .T. ) ;
#47490 = CARTESIAN_POINT ( 'NONE',  ( -30.64751926837171325, -23.47596703998600631, 11.44779298504228038 ) ) ;
#47492 = FACE_OUTER_BOUND ( 'NONE', #46185, .T. ) ;
#47491 = CIRCLE ( 'NONE', #83111, 11.85241003308275864 ) ;
#47493 = EDGE_CURVE ( 'NONE', #12728, #45608, #67884, .T. ) ;
#47494 = PLANE ( 'NONE',  #99218 ) ;
#47495 = FACE_BOUND ( 'NONE', #65442, .T. ) ;
#47496 = EDGE_CURVE ( 'NONE', #3648, #58574, #12153, .T. ) ;
#47497 = FACE_BOUND ( 'NONE', #21853, .T. ) ;
#47498 = CARTESIAN_POINT ( 'NONE',  ( -10.82925958622295859, 16.30987832687952022, 11.49999999999998934 ) ) ;
#47499 = AXIS2_PLACEMENT_3D ( 'NONE', #27190, #51026, #3371 ) ;
#47500 = EDGE_CURVE ( 'NONE', #64821, #30992, #111, .T. ) ;
#47501 = CARTESIAN_POINT ( 'NONE',  ( -52.52287095715006870, -23.47596703998600631, 11.44779298504229104 ) ) ;
#47502 = EDGE_LOOP ( 'NONE', ( #92524, #69906, #33460, #54316, #81905 ) ) ;
#47503 = CARTESIAN_POINT ( 'NONE',  ( -2.374466145016132845, -21.38244973876172494, -1.500000000000002220 ) ) ;
#47504 = CARTESIAN_POINT ( 'NONE',  ( -2.794871794871795156, -5.876774720514415407, 20.36318108974359475 ) ) ;
#47505 = ADVANCED_FACE ( 'NONE', ( #21104 ), #57698, .F. ) ;
#47506 = CARTESIAN_POINT ( 'NONE',  ( -121.5228709571500616, -24.65952944569305316, 1.056160979905705899 ) ) ;
#47507 = CARTESIAN_POINT ( 'NONE',  ( 13.91401389203221406, -6.376774720514426953, 28.26920385068457264 ) ) ;
#47508 = CARTESIAN_POINT ( 'NONE',  ( -68.62287095715007013, -24.33927499327854704, 9.819080762295815390 ) ) ;
#47509 = CARTESIAN_POINT ( 'NONE',  ( 22.85676281555306844, 1.471244944367766649, -1.500000000000002220 ) ) ;
#47510 = B_SPLINE_CURVE_WITH_KNOTS ( 'NONE', 3,
 ( #65077, #95994, #94488, #73658 ),
 .UNSPECIFIED., .F., .F.,
 ( 4, 4 ),
 ( 0.000000000000000000, 0.0001002978982766898939 ),
 .UNSPECIFIED. ) ;
#47511 = PERSON_AND_ORGANIZATION_ROLE ( 'design_supplier' ) ;
#47512 = CARTESIAN_POINT ( 'NONE',  ( -124.5562042904833504, -24.64965694238575367, 8.947790433994187609 ) ) ;
#47513 = CARTESIAN_POINT ( 'NONE',  ( -71.11503856163616888, -25.29900863253169518, 5.642877111387134548 ) ) ;
#47514 = CARTESIAN_POINT ( 'NONE',  ( 19.65109224456760728, -3.968444974485820786, 11.49999999999999645 ) ) ;
#47515 = CARTESIAN_POINT ( 'NONE',  ( -79.44434589896187049, -25.26612442218368670, 4.820847248093164339 ) ) ;
#47516 = CARTESIAN_POINT ( 'NONE',  ( -57.58953762381671737, -24.66019654487199020, 8.947790411086133489 ) ) ;
#47517 = DIRECTION ( 'NONE',  ( 0.000000000000000000, 0.000000000000000000, -1.000000000000000000 ) ) ;
#47518 = DIRECTION ( 'NONE',  ( 0.000000000000000000, 0.000000000000000000, -1.000000000000000000 ) ) ;
#47519 = ORIENTED_EDGE ( 'NONE', *, *, #16038, .T. ) ;
#47520 = EDGE_CURVE ( 'NONE', #50701, #48998, #90867, .T. ) ;
#47521 = FACE_OUTER_BOUND ( 'NONE', #25288, .T. ) ;
#47522 = CARTESIAN_POINT ( 'NONE',  ( 15.29254711327534899, -15.47666941828629739, 11.49999999999998934 ) ) ;
#47523 = CARTESIAN_POINT ( 'NONE',  ( -45.52287095715007581, -24.15516710230293995, 10.28746687063727272 ) ) ;
#47524 = CARTESIAN_POINT ( 'NONE',  ( 18.70796670040472165, 5.986831462552164140, -1.500000000000002220 ) ) ;
#47525 = CARTESIAN_POINT ( 'NONE',  ( -34.52287095715006160, -23.47593901973090169, -1.443836447538997314 ) ) ;
#47526 = TOROIDAL_SURFACE ( 'NONE', #8699, 2.000000000000000000, 1.000000000000000000 ) ;
#47527 = CARTESIAN_POINT ( 'NONE',  ( -109.5056412146432052, -25.31698062991398501, 4.749485475450724969 ) ) ;
#47528 = APPROVAL_STATUS ( 'not_yet_approved' ) ;
#47529 = CC_DESIGN_SECURITY_CLASSIFICATION ( #91265, ( #100427 ) ) ;
#47530 = CARTESIAN_POINT ( 'NONE',  ( -62.52287095715003318, -24.66019654487199730, 8.947790411086124607 ) ) ;
#47531 = LINE ( 'NONE', #1853, #553 ) ;
#47532 = CARTESIAN_POINT ( 'NONE',  ( 7.805751503010069037, -19.01748540344778959, 11.49999999999999645 ) ) ;
#47533 = CARTESIAN_POINT ( 'NONE',  ( 4.215004826710222474, -5.876774720514426953, 21.34072927444733381 ) ) ;
#47534 = CARTESIAN_POINT ( 'NONE',  ( -120.5936529139786160, -23.48783264082477018, -1.443836473390085695 ) ) ;
#47535 = AXIS2_PLACEMENT_3D ( 'NONE', #34176, #65148, #33163 ) ;
#47536 = CARTESIAN_POINT ( 'NONE',  ( 22.24477432615492134, 4.004077059304647968, 11.49999999999999645 ) ) ;
#47537 = VERTEX_POINT ( 'NONE', #81529 ) ;
#47538 = CARTESIAN_POINT ( 'NONE',  ( -99.72794805030189025, -25.31296386855978753, 4.442265286386216872 ) ) ;
#47539 = DIRECTION ( 'NONE',  ( 0.000000000000000000, 1.000000000000000000, 0.000000000000000000 ) ) ;
#47540 = PLANE ( 'NONE',  #61448 ) ;
#47541 = DIRECTION ( 'NONE',  ( 0.000000000000000000, -0.9999999999976377785, -2.173523156925979128E-06 ) ) ;
#47542 = AXIS2_PLACEMENT_3D ( 'NONE', #80308, #26527, #18900 ) ;
#47543 = EDGE_CURVE ( 'NONE', #92467, #14570, #96744, .T. ) ;
#47544 = CARTESIAN_POINT ( 'NONE',  ( -25.63919700385670453, -24.93063196310097496, 6.233789962485477787 ) ) ;
#47545 = DIRECTION ( 'NONE',  ( 0.8253571461740011328, -1.227195083036775770E-06, 0.5646109999442116001 ) ) ;
#47546 = EDGE_CURVE ( 'NONE', #33967, #81135, #64314, .T. ) ;
#47547 = ORIENTED_EDGE ( 'NONE', *, *, #1322, .T. ) ;
#47548 = CARTESIAN_POINT ( 'NONE',  ( -79.98791220707269645, -25.26749890627193906, 5.033164624709036694 ) ) ;
#47549 = CARTESIAN_POINT ( 'NONE',  ( 19.70479270790718829, 11.56945388388114360, 11.49999999999998934 ) ) ;
#47550 = CARTESIAN_POINT ( 'NONE',  ( 4.653733606810938284, -5.876774720514412742, 19.95301661664751336 ) ) ;
#47551 = B_SPLINE_SURFACE_WITH_KNOTS ( 'NONE', 3, 1, ( 
 ( #27167, #34779 ),
 ( #58128, #89560 ),
 ( #50501, #10940 ),
 ( #51008, #3347 ),
 ( #74334, #25658 ),
 ( #56631, #11933 ),
 ( #64759, #42898 ),
 ( #87560, #26159 ),
 ( #73344, #88068 ),
 ( #35285, #49514 ),
 ( #96181, #57626 ),
 ( #3837, #88567 ),
 ( #91545, #67237 ),
 ( #23908, #13918 ),
 ( #20530, #83429 ),
 ( #98652, #51505 ),
 ( #82437, #5315 ),
 ( #51999, #77680 ),
 ( #67737, #74821 ) ),
 .UNSPECIFIED., .F., .F., .F.,
 ( 4, 1, 1, 1, 1, 1, 1, 1, 1, 1, 1, 1, 1, 1, 1, 1, 4 ),
 ( 2, 2 ),
 ( 0.000000000000000000, 0.06184170298390887638, 0.1212623730944471651, 0.1807459488653155588, 0.2392309018221052130, 0.2983075587884627122, 0.3581827976158459825, 0.4203592307800690930, 0.4847924155141860592, 0.5499384837666880799, 0.6137182775404268487, 0.6766807072496276998, 0.7391541704483146624, 0.8021997032403502814, 0.8667401776162937388, 0.9320496524002453986, 1.000000000000000000 ),
 ( 0.000000000000000000, 1.000000000000000000 ),
 .UNSPECIFIED. ) ;
#47552 = CARTESIAN_POINT ( 'NONE',  ( -96.59125222054736071, -24.15543982623907482, -0.2315651400026596807 ) ) ;
#47553 = DIRECTION ( 'NONE',  ( 0.000000000000000000, 0.9999999999976377785, 2.173523156925979128E-06 ) ) ;
#47554 = CARTESIAN_POINT ( 'NONE',  ( 0.2029947971921062799, -22.41465419638480228, 11.49999999999999645 ) ) ;
#47555 = ORIENTED_EDGE ( 'NONE', *, *, #29938, .T. ) ;
#47556 = B_SPLINE_CURVE_WITH_KNOTS ( 'NONE', 3,
 ( #39815, #70773, #16975, #9867 ),
 .UNSPECIFIED., .F., .F.,
 ( 4, 4 ),
 ( 0.000000000000000000, 0.0004038461538461574074 ),
 .UNSPECIFIED. ) ;
#47557 = FACE_OUTER_BOUND ( 'NONE', #42326, .T. ) ;
#47558 = CARTESIAN_POINT ( 'NONE',  ( 5.197331492371871420, 21.31670716312865466, -1.500000000000002220 ) ) ;
#47559 = ADVANCED_FACE ( 'NONE', ( #35357 ), #90458, .T. ) ;
#47560 = DIRECTION ( 'NONE',  ( -3.773278334444167020E-23, 1.000000000000000000, 0.000000000000000000 ) ) ;
#47561 = CARTESIAN_POINT ( 'NONE',  ( -34.58065475290599267, -24.51419770103156637, 9.386484678747176957 ) ) ;
#47562 = PLANE ( 'NONE',  #11394 ) ;
#47563 = VERTEX_POINT ( 'NONE', #53078 ) ;
#47564 = CARTESIAN_POINT ( 'NONE',  ( -48.64595118538275642, -23.96169478059712787, 10.65365249895718236 ) ) ;
#47565 = EDGE_CURVE ( 'NONE', #79650, #100062, #31556, .T. ) ;
#47566 = CARTESIAN_POINT ( 'NONE',  ( 282.9764569301858046, 3.316774720514426900, 20.79159422840526616 ) ) ;
#47567 = ORIENTED_EDGE ( 'NONE', *, *, #1241, .F. ) ;
#47568 = CARTESIAN_POINT ( 'NONE',  ( -7.951223608505463503, 18.87544906973805325, -1.500000000000002220 ) ) ;
#47569 = EDGE_LOOP ( 'NONE', ( #30213, #4925, #34281, #61542, #16111 ) ) ;
#47570 = ORIENTED_EDGE ( 'NONE', *, *, #63923, .F. ) ;
#47571 = ORIENTED_EDGE ( 'NONE', *, *, #40565, .F. ) ;
#47572 = ORIENTED_EDGE ( 'NONE', *, *, #63550, .F. ) ;
#47573 = CARTESIAN_POINT ( 'NONE',  ( -14.58522200957802184, -17.87834940746265389, -1.500000000000002220 ) ) ;
#47574 = CARTESIAN_POINT ( 'NONE',  ( -82.52287095715006160, -23.47593901973090169, -1.443836447538996648 ) ) ;
#47575 = CARTESIAN_POINT ( 'NONE',  ( -18.23349369547262810, -8.965252873808195133, -1.500000000000002220 ) ) ;
#47576 = CIRCLE ( 'NONE', #2230, 0.9999999999999997780 ) ;
#47577 = VERTEX_POINT ( 'NONE', #30215 ) ;
#47578 = DIRECTION ( 'NONE',  ( -0.000000000000000000, 1.000000000000000000, -0.000000000000000000 ) ) ;
#47579 = CARTESIAN_POINT ( 'NONE',  ( -37.55620429048340014, -23.48783264082478084, -1.443836473390071484 ) ) ;
#47580 = DIRECTION ( 'NONE',  ( -3.773278334453080206E-23, 0.9999999999976377785, 2.173523156925979975E-06 ) ) ;
#47581 = CARTESIAN_POINT ( 'NONE',  ( 3.825970207471427020, -6.376774720514402972, 18.52126221587801780 ) ) ;
#47583 = ORIENTED_EDGE ( 'NONE', *, *, #56837, .T. ) ;
#47582 = CARTESIAN_POINT ( 'NONE',  ( -4.253298834618286506, 21.06115358058179154, 11.49999999999999645 ) ) ;
#47584 = CARTESIAN_POINT ( 'NONE',  ( -79.58953762381672448, -24.66019654487198665, 8.947790411086133489 ) ) ;
#47586 = VECTOR ( 'NONE', #92587, 1000.000000000000000 ) ;
#47585 = CARTESIAN_POINT ( 'NONE',  ( -49.35320922236618912, -25.26385781559679344, 4.652611292282501587 ) ) ;
#47587 = VERTEX_POINT ( 'NONE', #14992 ) ;
#47588 = CARTESIAN_POINT ( 'NONE',  ( 18.78520451414993531, -8.817701518030307994, -1.500000000000002220 ) ) ;
#47589 = ORIENTED_EDGE ( 'NONE', *, *, #51547, .F. ) ;
#47590 = APPROVAL ( #60992, 'UNSPECIFIED' ) ;
#47592 = ORIENTED_EDGE ( 'NONE', *, *, #97236, .F. ) ;
#47591 = CARTESIAN_POINT ( 'NONE',  ( -125.5896781930176189, -24.52300882791529801, 0.6510814631126508045 ) ) ;
#47593 = CARTESIAN_POINT ( 'NONE',  ( -41.65561799070277260, -23.73791477778911485, 11.05961554403170943 ) ) ;
#47594 = CARTESIAN_POINT ( 'NONE',  ( -124.4728709571500360, -25.40558663563427189, 5.000950442582704270 ) ) ;
#47595 = ORIENTED_EDGE ( 'NONE', *, *, #22042, .F. ) ;
#47596 = EDGE_LOOP ( 'NONE', ( #69652, #53891, #65164, #81424 ) ) ;
#47597 = CARTESIAN_POINT ( 'NONE',  ( -109.5562042904834072, -23.47596703998600631, 11.44779298504227683 ) ) ;
#47598 = CARTESIAN_POINT ( 'NONE',  ( -42.51345785107305630, -23.73791477778911485, 11.05961554403171299 ) ) ;
#47599 = CARTESIAN_POINT ( 'NONE',  ( -43.62863212119529521, -24.51419770103157347, 9.386484678747178734 ) ) ;
#47600 = CARTESIAN_POINT ( 'NONE',  ( -21.12052157030387889, 6.262089831203976331, 11.49999999999999645 ) ) ;
#47601 = CARTESIAN_POINT ( 'NONE',  ( -89.59466469485998630, -23.96169478059713498, 10.65365249895717703 ) ) ;
#47602 = CARTESIAN_POINT ( 'NONE',  ( -19.71520456405594857, 11.01310763156902972, 11.49999999999998934 ) ) ;
#47603 = CARTESIAN_POINT ( 'NONE',  ( 8.398332666215036824, -19.25654272332048578, -1.500000000000002220 ) ) ;
#47604 = CARTESIAN_POINT ( 'NONE',  ( 25.05730599792489599, 2.682774720514426559, -18.59674224247002172 ) ) ;
#47606 = ORIENTED_EDGE ( 'NONE', *, *, #90467, .T. ) ;
#47605 = DIRECTION ( 'NONE',  ( 0.000000000000000000, 2.173523156925980399E-06, -0.9999999999976378895 ) ) ;
#47607 = VERTEX_POINT ( 'NONE', #45961 ) ;
#47608 = PLANE ( 'NONE',  #41800 ) ;
#47609 = AXIS2_PLACEMENT_3D ( 'NONE', #90804, #21769, #52743 ) ;
#47610 = CARTESIAN_POINT ( 'NONE',  ( -113.6228709571500701, -24.33927499327855415, 9.819080762295810061 ) ) ;
#47611 = ORIENTED_EDGE ( 'NONE', *, *, #33869, .T. ) ;
#47612 = CARTESIAN_POINT ( 'NONE',  ( 13.25904570721172604, 16.46799385432867169, -1.500000000000002220 ) ) ;
#47613 = FACE_OUTER_BOUND ( 'NONE', #74899, .T. ) ;
#47614 = CARTESIAN_POINT ( 'NONE',  ( -50.58702570880215177, -25.26041116158741318, 7.558808615179929191 ) ) ;
#47615 = DIRECTION ( 'NONE',  ( -0.000000000000000000, 1.000000000000000000, -0.000000000000000000 ) ) ;
#47616 = CARTESIAN_POINT ( 'NONE',  ( 8.160000000000000142, 1.527978830621527617, 4.717155776778118259 ) ) ;
#47617 = CARTESIAN_POINT ( 'NONE',  ( -77.52287095715006160, -29.50247984919015209, -1.443849546365053582 ) ) ;
#47618 = CARTESIAN_POINT ( 'NONE',  ( -22.22723998432330106, 0.1330083165726352878, -1.500000000000002220 ) ) ;
#47619 = AXIS2_PLACEMENT_3D ( 'NONE', #29651, #73835, #90553 ) ;
#47620 = B_SPLINE_CURVE_WITH_KNOTS ( 'NONE', 3,
 ( #38533, #31424, #62381, #54776, #77082, #85712 ),
 .UNSPECIFIED., .F., .F.,
 ( 4, 2, 4 ),
 ( 0.000000000000000000, 0.001380764517854766267, 0.002761529035709532533 ),
 .UNSPECIFIED. ) ;
#47621 = CARTESIAN_POINT ( 'NONE',  ( -49.21454750704995007, -25.03220799397881891, 7.069183833275417328 ) ) ;
#47622 = EDGE_CURVE ( 'NONE', #72609, #33400, #59427, .T. ) ;
#47623 = EDGE_LOOP ( 'NONE', ( #3254, #61550, #29256, #85627 ) ) ;
#47624 = CARTESIAN_POINT ( 'NONE',  ( -51.08169923747086472, -25.31633088894497519, 4.960537870539334371 ) ) ;
#47625 = CARTESIAN_POINT ( 'NONE',  ( -64.62287095715004170, -24.33927499327854704, 9.819080762295820719 ) ) ;
#47626 = CARTESIAN_POINT ( 'NONE',  ( -126.5209009042890784, -24.34968618360934300, 0.1864209137778884418 ) ) ;
#47627 = CARTESIAN_POINT ( 'NONE',  ( -100.5075858015768517, -24.73486907724917927, 1.287355809206965240 ) ) ;
#47628 = CARTESIAN_POINT ( 'NONE',  ( -61.52287095715007581, -23.47593901973090169, -1.443836447538997092 ) ) ;
#47629 = CARTESIAN_POINT ( 'NONE',  ( -14.34788840963776124, 13.16932220997287928, 11.49999999999998934 ) ) ;
#47630 = EDGE_CURVE ( 'NONE', #92987, #30745, #91229, .T. ) ;
#47631 = CARTESIAN_POINT ( 'NONE',  ( 19.34736296927903254, -9.154118057783460216, 11.49999999999998934 ) ) ;
#47632 = CARTESIAN_POINT ( 'NONE',  ( -85.52287095715004739, -24.91570333825475103, 8.075032458260896107 ) ) ;
#47633 = CARTESIAN_POINT ( 'NONE',  ( -60.53048506470604195, -24.92592662360294042, 8.075495902990192931 ) ) ;
#47634 = ADVANCED_FACE ( 'NONE', ( #15982 ), #46954, .F. ) ;
#47635 = CARTESIAN_POINT ( 'NONE',  ( -100.6228709571500559, -24.52323809116984421, 9.355190652339416602 ) ) ;
#47636 = CARTESIAN_POINT ( 'NONE',  ( -101.3738023147422780, -25.27360125068057428, 3.986250616286608928 ) ) ;
#47637 = CARTESIAN_POINT ( 'NONE',  ( 21.16149768242404861, -8.233860041645145955, -1.500000000000002220 ) ) ;
#47638 = CARTESIAN_POINT ( 'NONE',  ( -28.98875734969026396, -5.965225279485572685, -0.08597719988137648983 ) ) ;
#47639 = CARTESIAN_POINT ( 'NONE',  ( -80.52287095715007581, -24.82558206586144323, 1.605769216559446377 ) ) ;
#47640 = CARTESIAN_POINT ( 'NONE',  ( -7.754168067426306266, 18.25094163199162622, 11.49999999999999645 ) ) ;
#47641 = CARTESIAN_POINT ( 'NONE',  ( -123.5204172166400696, -24.15620529776629510, 10.23563542870659404 ) ) ;
#47642 = CARTESIAN_POINT ( 'NONE',  ( -104.5228709571500758, -24.65952944569305316, 1.056160979905702346 ) ) ;
#47643 = CARTESIAN_POINT ( 'NONE',  ( 1.175186991919855872, -6.376774720514426953, 28.89597625626659649 ) ) ;
#47644 = VERTEX_POINT ( 'NONE', #95624 ) ;
#47645 = EDGE_CURVE ( 'NONE', #6118, #70435, #66639, .T. ) ;
#47646 = DIRECTION ( 'NONE',  ( -0.000000000000000000, -1.000000000000000000, -0.000000000000000000 ) ) ;
#47647 = CARTESIAN_POINT ( 'NONE',  ( -5.960145391809922089, -6.376774720514415407, 20.04104409779160534 ) ) ;
#47648 = AXIS2_PLACEMENT_3D ( 'NONE', #36435, #82114, #90227 ) ;
#47649 = CARTESIAN_POINT ( 'NONE',  ( -51.43440959051734751, -25.27412327365844646, 3.290885351747372844 ) ) ;
#47650 = CARTESIAN_POINT ( 'NONE',  ( -2.787017431591729988, -21.48445716988565835, -1.500000000000002220 ) ) ;
#47651 = CARTESIAN_POINT ( 'NONE',  ( -29.62287095715004881, -24.57400415421967566, 8.947790463233827651 ) ) ;
#47652 = CARTESIAN_POINT ( 'NONE',  ( -4.672984603565591755, -18.88948546680484242, -1.500000000000002220 ) ) ;
#47653 = CARTESIAN_POINT ( 'NONE',  ( 19.75748517575715368, -0.3587747205144265483, 28.87153971905864580 ) ) ;
#47654 = ORIENTED_EDGE ( 'NONE', *, *, #75381, .T. ) ;
#47655 = AXIS2_PLACEMENT_3D ( 'NONE', #45941, #53058, #75869 ) ;
#47656 = CARTESIAN_POINT ( 'NONE',  ( 2.178911383790714584, -20.24183328246387958, 11.49999999999999645 ) ) ;
#47657 = CARTESIAN_POINT ( 'NONE',  ( -110.5895376238167245, -23.48783264082479505, -1.443836473390060160 ) ) ;
#47658 = CARTESIAN_POINT ( 'NONE',  ( -48.62287095715004881, -24.66019654487199020, 8.947790411086135265 ) ) ;
#47659 = VERTEX_POINT ( 'NONE', #79888 ) ;
#47660 = CARTESIAN_POINT ( 'NONE',  ( -28.52287095715005805, -29.50247984919081290, -1.443849243165460372 ) ) ;
#47661 = CARTESIAN_POINT ( 'NONE',  ( 33.50941771711500650, 4.400593307868417625, -12.46354170163595221 ) ) ;
#47662 = CARTESIAN_POINT ( 'NONE',  ( -39.31539998891226162, -25.27985467206300640, 5.139621229108158218 ) ) ;
#47663 = CARTESIAN_POINT ( 'NONE',  ( -40.52633280619024703, -24.83644354573577928, 8.397322867130096569 ) ) ;
#47664 = FACE_OUTER_BOUND ( 'NONE', #5062, .T. ) ;
#47665 = CARTESIAN_POINT ( 'NONE',  ( 15.80722972286721983, -12.41807379269815215, -1.500000000000002220 ) ) ;
#47666 = EDGE_CURVE ( 'NONE', #29733, #70312, #18494, .T. ) ;
#47667 = DIRECTION ( 'NONE',  ( -1.000000000000000000, -3.773278334444167608E-23, -8.201307833595939069E-29 ) ) ;
#47668 = ORIENTED_EDGE ( 'NONE', *, *, #53162, .T. ) ;
#47669 = CARTESIAN_POINT ( 'NONE',  ( -66.51586011922388764, -23.73791477778911840, 11.05961554403170766 ) ) ;
#47670 = ADVANCED_FACE ( 'NONE', ( #41854 ), #26111, .F. ) ;
#47671 = CARTESIAN_POINT ( 'NONE',  ( 17.43399715339889511, -14.94103553264482720, 11.49999999999999645 ) ) ;
#47672 = CARTESIAN_POINT ( 'NONE',  ( -9.076218414377828836, -20.82814578352222767, 11.49999999999998934 ) ) ;
#47673 = EDGE_LOOP ( 'NONE', ( #78667, #56316, #8128, #25876 ) ) ;
#47674 = CARTESIAN_POINT ( 'NONE',  ( -30.47287095715005734, -23.78331967171602201, 10.94926139022358669 ) ) ;
#47675 = CARTESIAN_POINT ( 'NONE',  ( 33.65278273286722310, 3.366611878523314783, -11.65467467704458393 ) ) ;
#47676 = CARTESIAN_POINT ( 'NONE',  ( 32.45853543194704116, 5.965225279485572685, 9.169203677920338080 ) ) ;
#47677 = CARTESIAN_POINT ( 'NONE',  ( -105.5228709571501042, -23.48783264082477018, -1.443836473390085917 ) ) ;
#47678 = EDGE_CURVE ( 'NONE', #55816, #91672, #48477, .T. ) ;
#47679 = CARTESIAN_POINT ( 'NONE',  ( -128.5554931858794703, -24.51419770103157703, 9.386484678747171628 ) ) ;
#47680 = EDGE_CURVE ( 'NONE', #19685, #43485, #47491, .T. ) ;
#47681 = DIRECTION ( 'NONE',  ( 0.000000000000000000, -2.173523156925980399E-06, 0.9999999999976378895 ) ) ;
#47682 = CARTESIAN_POINT ( 'NONE',  ( -98.95846461277810135, -25.31200652517857819, 5.689168854314336166 ) ) ;
#47683 = EDGE_LOOP ( 'NONE', ( #40533, #95775, #13822, #1677 ) ) ;
#47684 = CARTESIAN_POINT ( 'NONE',  ( 18.16468007720714795, -9.286844270591712913, -1.500000000000002220 ) ) ;
#47685 = ORIENTED_EDGE ( 'NONE', *, *, #90605, .F. ) ;
#47686 = CARTESIAN_POINT ( 'NONE',  ( 14.37299948674089123, 17.95305339730678185, -1.500000000000002220 ) ) ;
#47687 = CARTESIAN_POINT ( 'NONE',  ( -63.62287095715004881, -23.47593901973091235, -1.443836447539007972 ) ) ;
#47688 = ORIENTED_EDGE ( 'NONE', *, *, #65712, .F. ) ;
#47689 = DIRECTION ( 'NONE',  ( 0.000000000000000000, 0.000000000000000000, 1.000000000000000000 ) ) ;
#47690 = CARTESIAN_POINT ( 'NONE',  ( -28.47875734969025885, 5.965225279485572685, -0.08597719988137300651 ) ) ;
#47691 = CARTESIAN_POINT ( 'NONE',  ( -24.90875734969025501, 3.316774720514426456, 26.43402280011862615 ) ) ;
#47693 = VERTEX_POINT ( 'NONE', #55070 ) ;
#47692 = CARTESIAN_POINT ( 'NONE',  ( 17.95810460983813783, 11.44545274529666479, 11.49999999999999645 ) ) ;
#47694 = ORIENTED_EDGE ( 'NONE', *, *, #15668, .T. ) ;
#47695 = CARTESIAN_POINT ( 'NONE',  ( 7.688942331755139747, 20.87172568467934752, -1.500000000000002220 ) ) ;
#47696 = CARTESIAN_POINT ( 'NONE',  ( -12.00526669028610272, -16.82065764665920682, 11.49999999999998934 ) ) ;
#47697 = VECTOR ( 'NONE', #56514, 1000.000000000000114 ) ;
#47698 = ADVANCED_FACE ( 'NONE', ( #64199 ), #56073, .F. ) ;
#47699 = ORIENTED_EDGE ( 'NONE', *, *, #47372, .T. ) ;
#47700 = CARTESIAN_POINT ( 'NONE',  ( -4.620655831143558601, -5.876774720514410077, 19.21747685089457036 ) ) ;
#47701 = CARTESIAN_POINT ( 'NONE',  ( -95.58289840528635750, -25.00182538069147142, 7.747789668545044250 ) ) ;
#47702 = ORIENTED_EDGE ( 'NONE', *, *, #97827, .F. ) ;
#47703 = LINE ( 'NONE', #64955, #99614 ) ;
#47704 = ADVANCED_FACE ( 'NONE', ( #70791 ), #56580, .T. ) ;
#47705 = ORIENTED_EDGE ( 'NONE', *, *, #38530, .F. ) ;
#47706 = CARTESIAN_POINT ( 'NONE',  ( -8.160000000000000142, -10.65233964170348635, -1.203735189656879756 ) ) ;
#47707 = CARTESIAN_POINT ( 'NONE',  ( -70.56964911583740729, -25.12720894619000234, 7.077432069396976111 ) ) ;
#47708 = CARTESIAN_POINT ( 'NONE',  ( 20.89859092893058801, 0.06103081833375877813, -1.500000000000002220 ) ) ;
#47709 = CARTESIAN_POINT ( 'NONE',  ( 4.989390281198801347, -21.28523531580253803, 11.49999999999999645 ) ) ;
#47710 = B_SPLINE_CURVE_WITH_KNOTS ( 'NONE', 3,
 ( #89312, #4078, #19781, #28904, #65502, #97418 ),
 .UNSPECIFIED., .F., .F.,
 ( 4, 2, 4 ),
 ( 0.000000000000000000, 0.001380901958385385509, 0.002761803916770771018 ),
 .UNSPECIFIED. ) ;
#47711 = VECTOR ( 'NONE', #71529, 1000.000000000000114 ) ;
#47712 = CARTESIAN_POINT ( 'NONE',  ( 31.63608488009066733, -3.316774720514426456, 27.34773273846990094 ) ) ;
#47713 = DIRECTION ( 'NONE',  ( -0.000000000000000000, 2.173523156925979552E-06, -0.9999999999976378895 ) ) ;
#47714 = CARTESIAN_POINT ( 'NONE',  ( -11.50411854321151672, 19.32100693743031528, -1.500000000000002220 ) ) ;
#47715 = EDGE_CURVE ( 'NONE', #26949, #99423, #10381, .T. ) ;
#47716 = EDGE_CURVE ( 'NONE', #43349, #27461, #55574, .T. ) ;
#47717 = CARTESIAN_POINT ( 'NONE',  ( -118.5578097239443025, -23.48786465467241769, 11.44779295918253581 ) ) ;
#47718 = DIRECTION ( 'NONE',  ( 1.000000000000000000, -7.960204194457801640E-17, 0.000000000000000000 ) ) ;
#47719 = CARTESIAN_POINT ( 'NONE',  ( -31.52287095715006160, -24.64965694238574656, 8.947790433994207149 ) ) ;
#47720 = ORIENTED_EDGE ( 'NONE', *, *, #37567, .T. ) ;
#47721 = VERTEX_POINT ( 'NONE', #24100 ) ;
#47722 = VERTEX_POINT ( 'NONE', #86007 ) ;
#47723 = VERTEX_POINT ( 'NONE', #16482 ) ;
#47724 = CARTESIAN_POINT ( 'NONE',  ( -18.57871158907727249, 10.67946855401146777, -1.500000000000002220 ) ) ;
#47725 = CARTESIAN_POINT ( 'NONE',  ( -6.430504157862594994, -21.42354456762059201, 11.49999999999999645 ) ) ;
#47726 = ORIENTED_EDGE ( 'NONE', *, *, #52594, .F. ) ;
#47727 = CARTESIAN_POINT ( 'NONE',  ( 18.99863377428308198, 9.053671573812124507, 11.49999999999998934 ) ) ;
#47728 = CARTESIAN_POINT ( 'NONE',  ( -30.40154487420265994, -25.30206656716858404, 5.002391647799127483 ) ) ;
#47729 = CARTESIAN_POINT ( 'NONE',  ( -19.80664267627650688, 2.137978742899185214, -1.500000000000002220 ) ) ;
#47730 = CARTESIAN_POINT ( 'NONE',  ( -50.57411766822878718, -25.00182538069146432, 7.747789668545041586 ) ) ;
#47731 = CARTESIAN_POINT ( 'NONE',  ( 3.004381791450704942, -5.876774720514419847, 20.78526834885430219 ) ) ;
#47732 = CARTESIAN_POINT ( 'NONE',  ( -7.037580251249667462, -20.86201633182841420, -1.500000000000002220 ) ) ;
#47733 = FACE_OUTER_BOUND ( 'NONE', #41491, .T. ) ;
#47734 = VERTEX_POINT ( 'NONE', #2788 ) ;
#47735 = FACE_OUTER_BOUND ( 'NONE', #25710, .T. ) ;
#47736 = EDGE_CURVE ( 'NONE', #69136, #50260, #33726, .T. ) ;
#47737 = CARTESIAN_POINT ( 'NONE',  ( -54.52287095715006870, -23.47596703998600631, 11.44779298504229104 ) ) ;
#47738 = CARTESIAN_POINT ( 'NONE',  ( -14.03827505669662479, 15.38897104800697591, 11.49999999999999645 ) ) ;
#47739 = CARTESIAN_POINT ( 'NONE',  ( 31.62831224182126988, -4.127879075750807480, 27.04291028225966542 ) ) ;
#47740 = CARTESIAN_POINT ( 'NONE',  ( -111.5895376238167387, -23.48786465467241769, 11.44779295918254114 ) ) ;
#47741 = CIRCLE ( 'NONE', #25049, 0.3000000000000016542 ) ;
#47742 = DIRECTION ( 'NONE',  ( 0.9951627101165076983, -0.09824042138329622254, -3.430045979798646929E-16 ) ) ;
#47743 = CARTESIAN_POINT ( 'NONE',  ( -19.36244235409943926, 8.944087295975924334, 11.49999999999998934 ) ) ;
#47744 = CARTESIAN_POINT ( 'NONE',  ( -53.62287095715005592, -29.50247984919015209, -1.443849546365058689 ) ) ;
#47745 = CARTESIAN_POINT ( 'NONE',  ( -117.5228709571500048, -23.73934037231757443, 11.05740245334327732 ) ) ;
#47746 = EDGE_CURVE ( 'NONE', #90318, #96355, #20595, .T. ) ;
#47747 = CARTESIAN_POINT ( 'NONE',  ( -64.58349049003693665, -24.51419770103159124, 9.386484678747168076 ) ) ;
#47748 = CARTESIAN_POINT ( 'NONE',  ( -71.31504266748430609, -25.30188801935125653, 5.302352381037461093 ) ) ;
#47749 = CARTESIAN_POINT ( 'NONE',  ( 11.64696156460271581, 19.30390316350253244, -1.500000000000002220 ) ) ;
#47750 = EDGE_CURVE ( 'NONE', #32461, #29559, #78815, .T. ) ;
#47751 = DIRECTION ( 'NONE',  ( -1.000000000000000000, -0.000000000000000000, -0.000000000000000000 ) ) ;
#47752 = ORIENTED_EDGE ( 'NONE', *, *, #22778, .F. ) ;
#47753 = B_SPLINE_CURVE_WITH_KNOTS ( 'NONE', 3,
 ( #49744, #26389, #57360, #88292 ),
 .UNSPECIFIED., .F., .F.,
 ( 4, 4 ),
 ( 0.1288497010136043508, 0.1298504480543696271 ),
 .UNSPECIFIED. ) ;
#47754 = CARTESIAN_POINT ( 'NONE',  ( -79.00182917920848524, -25.29558293519123779, 5.503601469187146655 ) ) ;
#47755 = CARTESIAN_POINT ( 'NONE',  ( -31.64312417419304424, -24.15620529776627379, 10.23563542870661536 ) ) ;
#47756 = CARTESIAN_POINT ( 'NONE',  ( 0.7877182283408599162, 19.66719298131377514, 11.49999999999999645 ) ) ;
#47757 = DIRECTION ( 'NONE',  ( -0.000000000000000000, -0.000000000000000000, -1.000000000000000000 ) ) ;
#47758 = CARTESIAN_POINT ( 'NONE',  ( -77.52287095715006160, -29.50250243563736774, 8.947779886222141599 ) ) ;
#47759 = VERTEX_POINT ( 'NONE', #94618 ) ;
#47760 = EDGE_CURVE ( 'NONE', #11284, #37448, #87005, .T. ) ;
#47761 = CARTESIAN_POINT ( 'NONE',  ( -111.5228709571500332, -23.94994826722564696, -0.6494450866342719175 ) ) ;
#47762 = CARTESIAN_POINT ( 'NONE',  ( -124.4728709571500360, -25.21147115331109489, 5.000950864497200499 ) ) ;
#47763 = CARTESIAN_POINT ( 'NONE',  ( -48.52287095715006160, -29.50250786944525672, 11.44777988621624054 ) ) ;
#47764 = EDGE_CURVE ( 'NONE', #5650, #34190, #69116, .T. ) ;
#47765 = CARTESIAN_POINT ( 'NONE',  ( 14.76093561896379214, 3.316774720514426456, -26.55548769130089681 ) ) ;
#47766 = CARTESIAN_POINT ( 'NONE',  ( 19.48663422773152121, -3.193742178437300794, -1.500000000000002220 ) ) ;
#47767 = ADVANCED_FACE ( 'NONE', ( #3298 ), #12866, .F. ) ;
#47768 = VERTEX_POINT ( 'NONE', #36223 ) ;
#47769 = CARTESIAN_POINT ( 'NONE',  ( 19.91930514195032487, 3.327535025408205893, 11.49999999999999645 ) ) ;
#47770 = CARTESIAN_POINT ( 'NONE',  ( 7.844850387708879325, 6.376774720514429617, -25.09814097568368751 ) ) ;
#47771 = VECTOR ( 'NONE', #68503, 1000.000000000000114 ) ;
#47772 = COORDINATED_UNIVERSAL_TIME_OFFSET ( 0, 0, .AHEAD. ) ;
#47773 = EDGE_LOOP ( 'NONE', ( #90307, #45365, #69303, #169 ) ) ;
#47774 = CARTESIAN_POINT ( 'NONE',  ( -77.62287095715005592, -29.50250786944525672, 11.44777988621623521 ) ) ;
#47775 = CARTESIAN_POINT ( 'NONE',  ( -81.42380231474228935, -25.30401792888237011, 5.197789011716578145 ) ) ;
#47776 = CARTESIAN_POINT ( 'NONE',  ( -6.499999999999992895, -1.517883041479705813E-15, 3.499999999999998224 ) ) ;
#47777 = FACE_OUTER_BOUND ( 'NONE', #74384, .T. ) ;
#47778 = CARTESIAN_POINT ( 'NONE',  ( -59.22287095715007865, -23.47593901973090524, -1.443836447538997980 ) ) ;
#47779 = DIRECTION ( 'NONE',  ( 1.000000000000000000, 3.773278334444167608E-23, 8.201307833595939069E-29 ) ) ;
#47780 = CARTESIAN_POINT ( 'NONE',  ( 18.80801646011137507, -6.797914457553222434, 11.49999999999998934 ) ) ;
#47781 = VECTOR ( 'NONE', #41477, 1000.000000000000000 ) ;
#47782 = CARTESIAN_POINT ( 'NONE',  ( -34.55620429048339304, -24.64898659630528144, 1.056161002820817263 ) ) ;
#47783 = CARTESIAN_POINT ( 'NONE',  ( -67.62287095715004170, -24.66019654487199020, 8.947790411086131712 ) ) ;
#47784 = ORIENTED_EDGE ( 'NONE', *, *, #72627, .F. ) ;
#47785 = EDGE_CURVE ( 'NONE', #61548, #93369, #87282, .T. ) ;
#47786 = CARTESIAN_POINT ( 'NONE',  ( -79.55042822669543057, -24.15620529776628089, 10.23563542870660470 ) ) ;
#47787 = CARTESIAN_POINT ( 'NONE',  ( -59.62287095715004881, -29.50250243563736774, 8.947779886222145151 ) ) ;
#47788 = CARTESIAN_POINT ( 'NONE',  ( -125.6228709571500559, -24.99156045073393173, 7.747789690856161648 ) ) ;
#47789 = CARTESIAN_POINT ( 'NONE',  ( -82.58953762381673869, -24.64965694238406968, 8.947790433994654791 ) ) ;
#47790 = DIRECTION ( 'NONE',  ( 0.000000000000000000, 0.000000000000000000, -1.000000000000000000 ) ) ;
#47791 = DIRECTION ( 'NONE',  ( -0.6392559695863502256, 6.454799914155189828E-16, -0.7689940216596065081 ) ) ;
#47792 = PLANE ( 'NONE',  #96544 ) ;
#47793 = CARTESIAN_POINT ( 'NONE',  ( -73.62287095715005592, -24.65952944569304606, 1.056160979905698794 ) ) ;
#47794 = VERTEX_POINT ( 'NONE', #27111 ) ;
#47795 = CARTESIAN_POINT ( 'NONE',  ( 13.49383759531269433, -15.17088004136028090, 11.49999999999998934 ) ) ;
#47796 = CARTESIAN_POINT ( 'NONE',  ( 5.514125806255895004E-17, -29.50248528299834305, 1.056150588822498460 ) ) ;
#47797 = DIRECTION ( 'NONE',  ( 0.000000000000000000, 2.173523156925980399E-06, -0.9999999999976378895 ) ) ;
#47798 = ORIENTED_EDGE ( 'NONE', *, *, #158, .F. ) ;
#47799 = CARTESIAN_POINT ( 'NONE',  ( -50.40445135320379677, -25.26264178517331871, 7.101635255499235910 ) ) ;
#47800 = CARTESIAN_POINT ( 'NONE',  ( -13.64458216870221818, 14.86554040878868044, -1.500000000000002220 ) ) ;
#47801 = CARTESIAN_POINT ( 'NONE',  ( -11.89019930860364482, -17.45089671868802128, 11.49999999999999645 ) ) ;
#47802 = VECTOR ( 'NONE', #45276, 1000.000000000000000 ) ;
#47803 = CARTESIAN_POINT ( 'NONE',  ( 20.51613352552997327, 8.347415244503286758, 11.49999999999998934 ) ) ;
#47804 = CARTESIAN_POINT ( 'NONE',  ( 11.93631617611541351, -16.73449621718459923, 11.49999999999998934 ) ) ;
#47805 = EDGE_CURVE ( 'NONE', #83635, #27797, #89652, .T. ) ;
#47806 = CARTESIAN_POINT ( 'NONE',  ( 6.763596848542221984, -5.876774720514426065, 21.40271460634751577 ) ) ;
#47807 = ORIENTED_EDGE ( 'NONE', *, *, #4355, .F. ) ;
#47808 = CARTESIAN_POINT ( 'NONE',  ( -60.62287095715004881, -29.50249982740957577, 7.747779886224967605 ) ) ;
#47809 = VERTEX_POINT ( 'NONE', #89014 ) ;
#47810 = DIRECTION ( 'NONE',  ( -3.773278334453080206E-23, 0.9999999999976377785, 2.173523156925979975E-06 ) ) ;
#47811 = DIRECTION ( 'NONE',  ( -1.000000000000000000, -0.000000000000000000, 0.000000000000000000 ) ) ;
#47812 = ORIENTED_EDGE ( 'NONE', *, *, #19177, .T. ) ;
#47813 = ORIENTED_EDGE ( 'NONE', *, *, #70914, .F. ) ;
#47814 = ORIENTED_EDGE ( 'NONE', *, *, #56085, .F. ) ;
#47815 = CARTESIAN_POINT ( 'NONE',  ( -112.6228709571501412, -23.96127896941632685, -0.6493128931037773777 ) ) ;
#47816 = CARTESIAN_POINT ( 'NONE',  ( -127.6228709571500275, -24.66019654487199730, 8.947790411086121054 ) ) ;
#47817 = CARTESIAN_POINT ( 'NONE',  ( 5.627902640648289712, -6.376774720514413630, 20.02890049923285787 ) ) ;
#47818 = CARTESIAN_POINT ( 'NONE',  ( 18.07348078632662691, -10.09602009226539288, -1.500000000000002220 ) ) ;
#47819 = CARTESIAN_POINT ( 'NONE',  ( -12.04083774165243881, -18.01462592983040523, 11.49999999999999645 ) ) ;
#47820 = ORIENTED_EDGE ( 'NONE', *, *, #42073, .T. ) ;
#47821 = EDGE_CURVE ( 'NONE', #34695, #68647, #19488, .T. ) ;
#47822 = DIRECTION ( 'NONE',  ( 1.330598087067427724E-14, 0.000000000000000000, -1.000000000000000000 ) ) ;
#47823 = CARTESIAN_POINT ( 'NONE',  ( -111.6391784447225888, -25.23279326416602331, 3.670920698832722096 ) ) ;
#47824 = CARTESIAN_POINT ( 'NONE',  ( -15.27869365379592281, -16.34152646814254339, 11.49999999999998934 ) ) ;
#47825 = EDGE_CURVE ( 'NONE', #94137, #83680, #51451, .T. ) ;
#47826 = EDGE_CURVE ( 'NONE', #83609, #42451, #77562, .T. ) ;
#47827 = CARTESIAN_POINT ( 'NONE',  ( -84.62287095715005592, -23.48783264082479150, -1.443836473390065489 ) ) ;
#47828 = PLANE ( 'NONE',  #44879 ) ;
#47829 = ORIENTED_EDGE ( 'NONE', *, *, #49034, .T. ) ;
#47830 = CARTESIAN_POINT ( 'NONE',  ( 33.25738712673413033, -4.772289986317655774, -12.75102155484566424 ) ) ;
#47831 = CARTESIAN_POINT ( 'NONE',  ( -35.48813154574202144, -24.40133493613049609, 9.663955038902800609 ) ) ;
#47832 = EDGE_CURVE ( 'NONE', #65938, #83405, #37496, .T. ) ;
#47833 = ORIENTED_EDGE ( 'NONE', *, *, #45661, .T. ) ;
#47834 = ORIENTED_EDGE ( 'NONE', *, *, #19135, .T. ) ;
#47835 = AXIS2_PLACEMENT_3D ( 'NONE', #58137, #2345, #11443 ) ;
#47836 = CARTESIAN_POINT ( 'NONE',  ( -87.55620429048337883, -23.48786465467241058, 11.44779295918253936 ) ) ;
#47837 = ORIENTED_EDGE ( 'NONE', *, *, #42705, .F. ) ;
#47838 = DIRECTION ( 'NONE',  ( -1.000000000000000000, -3.773278334444167608E-23, -8.201307833595939069E-29 ) ) ;
#47839 = CARTESIAN_POINT ( 'NONE',  ( -12.22836702412972087, 17.35733969022439993, -1.500000000000002220 ) ) ;
#47840 = ORIENTED_EDGE ( 'NONE', *, *, #71144, .T. ) ;
#47841 = CARTESIAN_POINT ( 'NONE',  ( -50.52448634810669148, -25.00158670708910691, 2.256160236439223254 ) ) ;
#47842 = CARTESIAN_POINT ( 'NONE',  ( -8.041798833237560729, -20.28069125152608976, -1.500000000000002220 ) ) ;
#47843 = CARTESIAN_POINT ( 'NONE',  ( -88.88918693012689687, -25.22391110550272941, 6.409327647371936720 ) ) ;
#47844 = CARTESIAN_POINT ( 'NONE',  ( 32.88562546571903056, -5.965225279485572685, -5.083907541707159972 ) ) ;
#47845 = DIRECTION ( 'NONE',  ( 0.9976052577199501226, -2.125886612716675376E-15, 0.06916465693916179491 ) ) ;
#47846 = CARTESIAN_POINT ( 'NONE',  ( 1.472770742059883897, 21.73951962378590963, -1.500000000000002220 ) ) ;
#47847 = CARTESIAN_POINT ( 'NONE',  ( -30.57287095715007297, -24.38244319455381159, 0.3197473736007364065 ) ) ;
#47848 = EDGE_LOOP ( 'NONE', ( #49470, #11625, #28788, #55856 ) ) ;
#47849 = DIRECTION ( 'NONE',  ( -3.773278334444165844E-23, 1.000000000000000000, 0.000000000000000000 ) ) ;
#47850 = CARTESIAN_POINT ( 'NONE',  ( -48.87675733776060838, -25.12782531155001919, 6.266175665688602514 ) ) ;
#47851 = EDGE_CURVE ( 'NONE', #18484, #871, #87980, .T. ) ;
#47852 = B_SPLINE_CURVE_WITH_KNOTS ( 'NONE', 3,
 ( #41714, #9742, #72654, #40697, #34091, #65064, #26479, #88371, #18850, #4637, #58435, #89865, #67540, #21833, #27479, #50814, #52809, #98964, #36570 ),
 .UNSPECIFIED., .F., .F.,
 ( 4, 1, 1, 1, 1, 1, 1, 1, 1, 1, 1, 1, 1, 1, 1, 1, 4 ),
 ( 0.000000000000000000, 0.06184170298390879311, 0.1212623730944467210, 0.1807459488653150592, 0.2392309018221055461, 0.2983075587884643221, 0.3581827976158475924, 0.4203592307800689265, 0.4847924155141841718, 0.5499384837666866366, 0.6137182775404276258, 0.6766807072496321407, 0.7391541704483172159, 0.8021997032403536121, 0.8667401776163008442, 0.9320496524002468419, 1.000000000000000000 ),
 .UNSPECIFIED. ) ;
#47853 = ORIENTED_EDGE ( 'NONE', *, *, #35066, .F. ) ;
#47854 = AXIS2_PLACEMENT_3D ( 'NONE', #27124, #50460, #81411 ) ;
#47855 = DIRECTION ( 'NONE',  ( 0.000000000000000000, 0.000000000000000000, 1.000000000000000000 ) ) ;
#47856 = VECTOR ( 'NONE', #40943, 1000.000000000000000 ) ;
#47857 = ORIENTED_EDGE ( 'NONE', *, *, #36961, .T. ) ;
#47858 = EDGE_CURVE ( 'NONE', #39939, #72639, #19332, .T. ) ;
#47859 = EDGE_LOOP ( 'NONE', ( #55312, #86653, #10778, #33319 ) ) ;
#47860 = CARTESIAN_POINT ( 'NONE',  ( -27.97404546388469626, -24.80060134974466379, 2.305086465424985409 ) ) ;
#47861 = CARTESIAN_POINT ( 'NONE',  ( -119.6228709571500559, -23.47593901973091235, -1.443836447538997536 ) ) ;
#47862 = CARTESIAN_POINT ( 'NONE',  ( -21.08002519818654363, -2.465602145356518893, 11.49999999999998934 ) ) ;
#47863 = LINE ( 'NONE', #78784, #85416 ) ;
#47864 = CARTESIAN_POINT ( 'NONE',  ( -40.62287095715005592, -29.50248528299804818, 1.056150453629031594 ) ) ;
#47865 = EDGE_CURVE ( 'NONE', #9142, #93778, #11383, .T. ) ;
#47866 = DIRECTION ( 'NONE',  ( -0.9685340172660600322, 0.000000000000000000, 0.2488812114211667315 ) ) ;
#47867 = CARTESIAN_POINT ( 'NONE',  ( 31.79364159983995464, -2.682774720514426559, -11.59305536555894278 ) ) ;
#47868 = CARTESIAN_POINT ( 'NONE',  ( -1.428710472040144452, 19.32843595812722626, 11.49999999999998934 ) ) ;
#47869 = CARTESIAN_POINT ( 'NONE',  ( -117.5178510921751354, -24.35071581493544457, 9.817618358456019934 ) ) ;
#47870 = VERTEX_POINT ( 'NONE', #34724 ) ;
#47871 = CARTESIAN_POINT ( 'NONE',  ( -5.499840656826012975, 18.73951620154120334, 11.49999999999999645 ) ) ;
#47872 = CARTESIAN_POINT ( 'NONE',  ( -8.499999999999987566, 18.74999999999999645, 2.100000000000000089 ) ) ;
#47873 = DIRECTION ( 'NONE',  ( 0.000000000000000000, 0.000000000000000000, -1.000000000000000000 ) ) ;
#47874 = ORIENTED_EDGE ( 'NONE', *, *, #3654, .F. ) ;
#47875 = ADVANCED_FACE ( 'NONE', ( #38703 ), #15990, .T. ) ;
#47876 = CARTESIAN_POINT ( 'NONE',  ( 4.948291700218025113, -6.376774720514418959, 20.47145334051262111 ) ) ;
#47877 = CARTESIAN_POINT ( 'NONE',  ( -89.64224457987518235, -23.48783264082478084, -1.443836473390068154 ) ) ;
#47879 = EDGE_CURVE ( 'NONE', #15338, #15222, #23459, .T. ) ;
#47878 = CARTESIAN_POINT ( 'NONE',  ( -103.6228709571500559, -23.47593901973091235, -1.443836447539001089 ) ) ;
#47880 = FACE_OUTER_BOUND ( 'NONE', #10030, .T. ) ;
#47881 = CARTESIAN_POINT ( 'NONE',  ( -18.74838588596843181, -5.942601993926947657, 11.49999999999998934 ) ) ;
#47882 = VERTEX_POINT ( 'NONE', #69667 ) ;
#47883 = AXIS2_PLACEMENT_3D ( 'NONE', #34188, #28072, #80350 ) ;
#47884 = CARTESIAN_POINT ( 'NONE',  ( -11.65619939812097527, 18.16556634249905855, -1.500000000000002220 ) ) ;
#47885 = DIRECTION ( 'NONE',  ( 0.9951627101165076983, -0.09824042138329622254, -3.430045979798646929E-16 ) ) ;
#47886 = CARTESIAN_POINT ( 'NONE',  ( -108.5228709571500616, -24.64898659630528854, 1.056161002820831474 ) ) ;
#47887 = B_SPLINE_CURVE_WITH_KNOTS ( 'NONE', 3,
 ( #61622, #56891, #69721, #62114, #69212, #9693, #18801, #55887 ),
 .UNSPECIFIED., .F., .F.,
 ( 4, 2, 2, 4 ),
 ( 6.391158118969102054E-06, 0.002007136338672930488, 0.003007508928949909066, 0.004007881519226887644 ),
 .UNSPECIFIED. ) ;
#47888 = PERSON_AND_ORGANIZATION_ROLE ( 'creator' ) ;
#47889 = CARTESIAN_POINT ( 'NONE',  ( -125.5228709571501469, -24.92604778743018912, 8.074972756849362554 ) ) ;
#47890 = CARTESIAN_POINT ( 'NONE',  ( 4.547994309883463870, -6.376774720514422512, 20.87593061325451416 ) ) ;
#47891 = CARTESIAN_POINT ( 'NONE',  ( -97.58660980088102121, -24.51419770103157703, 9.386484678747176957 ) ) ;
#47892 = FACE_OUTER_BOUND ( 'NONE', #25103, .T. ) ;
#47893 = APPLICATION_CONTEXT ( 'configuration controlled 3d designs of mechanical parts and assemblies' ) ;
#47894 =( BOUNDED_SURFACE ( )  B_SPLINE_SURFACE ( 3, 2, ( 
 ( #1823, #73335, #97165 ),
 ( #65739, #89057, #28155 ),
 ( #81934, #82427, #50492 ),
 ( #27658, #57618, #98141 ),
 ( #59608, #42888, #81444 ),
 ( #73821, #20521, #59112 ),
 ( #3828, #34765, #43877 ),
 ( #27155, #58120, #35770 ),
 ( #4324, #82919, #3338 ),
 ( #90539, #26657, #96168 ),
 ( #28649, #74810, #11924 ),
 ( #88557, #21022, #35274 ) ),
 .UNSPECIFIED., .F., .F., .T. ) 
 B_SPLINE_SURFACE_WITH_KNOTS ( ( 4, 2, 2, 2, 2, 4 ),
 ( 3, 3 ),
 ( -3.428680950268159222E-15, 0.001642567453077259246, 0.003285134906157947173, 0.004106418632698291028, 0.004927702359238635317, 0.006570269812319323027 ),
 ( 0.000000000000000000, 1.000000000000000000 ),
 .UNSPECIFIED. ) 
 GEOMETRIC_REPRESENTATION_ITEM ( )  RATIONAL_B_SPLINE_SURFACE ( (
 ( 1.000000000000000000, 0.7071067811865476838, 1.000000000000000000),
 ( 1.000000000000000000, 0.7071067811865476838, 1.000000000000000000),
 ( 1.000000000000000000, 0.7071067811865476838, 1.000000000000000000),
 ( 1.000000000000000000, 0.7071067811865476838, 1.000000000000000000),
 ( 1.000000000000000000, 0.7071067811865476838, 1.000000000000000000),
 ( 1.000000000000000000, 0.7071067811865476838, 1.000000000000000000),
 ( 1.000000000000000000, 0.7071067811865476838, 1.000000000000000000),
 ( 1.000000000000000000, 0.7071067811865476838, 1.000000000000000000),
 ( 1.000000000000000000, 0.7071067811865476838, 1.000000000000000000),
 ( 1.000000000000000000, 0.7071067811865476838, 1.000000000000000000),
 ( 1.000000000000000000, 0.7071067811865476838, 1.000000000000000000),
 ( 1.000000000000000000, 0.7071067811865476838, 1.000000000000000000) ) ) 
 REPRESENTATION_ITEM ( '' )  SURFACE ( )  );
#47895 = FACE_OUTER_BOUND ( 'NONE', #48880, .T. ) ;
#47896 = CARTESIAN_POINT ( 'NONE',  ( -73.52287095715007581, -23.48786465467241058, 11.44779295918254647 ) ) ;
#47897 = CARTESIAN_POINT ( 'NONE',  ( -114.5916529831659858, -23.96169478059714208, 10.65365249895717170 ) ) ;
#47898 = CARTESIAN_POINT ( 'NONE',  ( 10.08953278062578462, 17.19620541797624824, -1.500000000000002220 ) ) ;
#47899 = DIRECTION ( 'NONE',  ( -3.773278334444167608E-23, 1.000000000000000000, 0.000000000000000000 ) ) ;
#47900 = CARTESIAN_POINT ( 'NONE',  ( -3.387584560642538101, 19.54024307811383210, -1.500000000000002220 ) ) ;
#47901 = ORIENTED_EDGE ( 'NONE', *, *, #89661, .F. ) ;
#47902 = DIRECTION ( 'NONE',  ( -1.000000000000000000, 0.000000000000000000, -0.000000000000000000 ) ) ;
#47903 = CARTESIAN_POINT ( 'NONE',  ( 13.60020833695035947, 0.000000000000000000, 0.000000000000000000 ) ) ;
#47904 = PLANE ( 'NONE',  #50771 ) ;
#47905 = CARTESIAN_POINT ( 'NONE',  ( 20.56943099487245519, -2.726235779781958968, 11.49999999999999645 ) ) ;
#47906 = CARTESIAN_POINT ( 'NONE',  ( -127.4728709571500360, -29.48149383318413541, 5.000941581248043555 ) ) ;
#47907 = DIRECTION ( 'NONE',  ( -3.773278334444167608E-23, 1.000000000000000000, 0.000000000000000000 ) ) ;
#47908 = CARTESIAN_POINT ( 'NONE',  ( -20.44213351528904354, 10.05872170072450977, 11.49999999999999645 ) ) ;
#47909 = AXIS2_PLACEMENT_3D ( 'NONE', #46927, #31188, #93086 ) ;
#47910 = ORIENTED_EDGE ( 'NONE', *, *, #68203, .F. ) ;
#47911 = CARTESIAN_POINT ( 'NONE',  ( -57.62287095715004881, -23.73907113216990794, -1.053371485793229922 ) ) ;
#47912 = CARTESIAN_POINT ( 'NONE',  ( -100.5895376238167245, -25.00158670708909270, 2.256160236439166411 ) ) ;
#47913 = EDGE_LOOP ( 'NONE', ( #96860, #94582, #21206, #3175 ) ) ;
#47914 = AXIS2_PLACEMENT_3D ( 'NONE', #80810, #29004, #89419 ) ;
#47915 = CARTESIAN_POINT ( 'NONE',  ( -2.107266074560359748, -20.09985696230311447, -1.500000000000002220 ) ) ;
#47916 = CARTESIAN_POINT ( 'NONE',  ( 9.010057473089011282, -0.9200333157601816580, -3.712238059855192951 ) ) ;
#47917 = AXIS2_PLACEMENT_3D ( 'NONE', #83274, #6150, #12755 ) ;
#47918 = FACE_OUTER_BOUND ( 'NONE', #89864, .T. ) ;
#47919 = VECTOR ( 'NONE', #18692, 1000.000000000000000 ) ;
#47920 = ORIENTED_EDGE ( 'NONE', *, *, #91901, .T. ) ;
#47921 = CARTESIAN_POINT ( 'NONE',  ( -6.499999999999992895, 1.999999999999999112, 3.499999999999999112 ) ) ;
#47922 = CARTESIAN_POINT ( 'NONE',  ( -13.60431050971674694, 18.46711184989817411, -1.500000000000002220 ) ) ;
#47923 = CARTESIAN_POINT ( 'NONE',  ( -84.52287095715001897, -23.95044443724990657, 10.65354141964648704 ) ) ;
#47924 = CARTESIAN_POINT ( 'NONE',  ( 10.22567584263966722, 17.17405255344276682, -1.500000000000002220 ) ) ;
#47925 = CARTESIAN_POINT ( 'NONE',  ( 31.88667425545054002, 2.682774720514426559, -9.651215965565025812 ) ) ;
#47926 = CARTESIAN_POINT ( 'NONE',  ( 4.154569570224219355, 20.57273982587956240, 11.49999999999999645 ) ) ;
#47927 = DIRECTION ( 'NONE',  ( 0.000000000000000000, 0.9999999999976377785, 2.173523156925979128E-06 ) ) ;
#47928 = CARTESIAN_POINT ( 'NONE',  ( -114.6228709571500701, -23.47596703998600631, 11.44779298504227860 ) ) ;
#47929 = CARTESIAN_POINT ( 'NONE',  ( 13.62230711432095553, -17.35066874027886286, -1.500000000000002220 ) ) ;
#47930 = DIRECTION ( 'NONE',  ( -1.000000000000000000, 0.000000000000000000, 0.000000000000000000 ) ) ;
#47931 = ORIENTED_EDGE ( 'NONE', *, *, #46246, .T. ) ;
#47932 = CARTESIAN_POINT ( 'NONE',  ( -20.77875734969026311, -6.143225279485574397, 27.31649921512899937 ) ) ;
#47933 = CARTESIAN_POINT ( 'NONE',  ( -49.50910156767503878, -25.18440247356948447, 3.963069022222974969 ) ) ;
#47934 = DIRECTION ( 'NONE',  ( -0.000000000000000000, 2.173523156925979552E-06, -0.9999999999976378895 ) ) ;
#47935 = ORIENTED_EDGE ( 'NONE', *, *, #69471, .F. ) ;
#47936 = CARTESIAN_POINT ( 'NONE',  ( 3.052815417670126319, -6.376774720514406525, 18.46676085997033923 ) ) ;
#47937 = ADVANCED_FACE ( 'NONE', ( #30593 ), #60528, .T. ) ;
#47938 = VERTEX_POINT ( 'NONE', #30092 ) ;
#47939 = EDGE_CURVE ( 'NONE', #54059, #12619, #75761, .T. ) ;
#47940 = ORIENTED_EDGE ( 'NONE', *, *, #87635, .T. ) ;
#47941 = CARTESIAN_POINT ( 'NONE',  ( 6.499999999999992895, -5.174132726397565334E-16, 0.000000000000000000 ) ) ;
#47942 = CARTESIAN_POINT ( 'NONE',  ( 31.60706529141452137, 4.540774720514427543, 26.12024523944105070 ) ) ;
#47943 = CARTESIAN_POINT ( 'NONE',  ( -4.194375271223358403, -5.876774720514417183, 20.09898898868106087 ) ) ;
#47944 = CARTESIAN_POINT ( 'NONE',  ( 14.40702264168333890, -14.58922348230443689, -1.500000000000002220 ) ) ;
#47945 = EDGE_CURVE ( 'NONE', #15171, #95755, #85375, .T. ) ;
#47946 = ORIENTED_EDGE ( 'NONE', *, *, #76788, .T. ) ;
#47947 = CARTESIAN_POINT ( 'NONE',  ( -60.52287095715006160, -29.50250786944525672, 11.44777988621623876 ) ) ;
#47948 = DIRECTION ( 'NONE',  ( -0.9951627101165078093, 0.000000000000000000, 0.09824042138329590335 ) ) ;
#47949 = DIRECTION ( 'NONE',  ( 0.000000000000000000, 0.000000000000000000, -1.000000000000000000 ) ) ;
#47950 = CARTESIAN_POINT ( 'NONE',  ( -20.55991158545366204, 8.586518200734140294, -1.500000000000002220 ) ) ;
#47951 = ADVANCED_FACE ( 'NONE', ( #36719 ), #68621, .T. ) ;
#47952 = B_SPLINE_CURVE_WITH_KNOTS ( 'NONE', 3,
 ( #80395, #10885, #99092, #7245 ),
 .UNSPECIFIED., .F., .F.,
 ( 4, 4 ),
 ( 0.000000000000000000, 0.0001000000000000028644 ),
 .UNSPECIFIED. ) ;
#47953 = LINE ( 'NONE', #46949, #93412 ) ;
#47954 = CARTESIAN_POINT ( 'NONE',  ( -1.456683411003494966, -5.876774720514416295, 19.95737465391042775 ) ) ;
#47955 = ORIENTED_EDGE ( 'NONE', *, *, #44736, .F. ) ;
#47956 = CARTESIAN_POINT ( 'NONE',  ( -96.62287095715009855, -24.34917612406837861, 0.1852690917426671191 ) ) ;
#47957 = CARTESIAN_POINT ( 'NONE',  ( -124.6228709571499991, -23.94994826722566117, -0.6494450866342683648 ) ) ;
#47958 = CARTESIAN_POINT ( 'NONE',  ( 16.93201058511109380, 12.15574511561022852, -1.500000000000002220 ) ) ;
#47959 = VERTEX_POINT ( 'NONE', #16869 ) ;
#47961 = ORIENTED_EDGE ( 'NONE', *, *, #78741, .F. ) ;
#47960 = CARTESIAN_POINT ( 'NONE',  ( 0.3910256410256418569, -6.376774720514420736, 20.67377804487180271 ) ) ;
#47962 = ORIENTED_EDGE ( 'NONE', *, *, #3873, .F. ) ;
#47963 = CARTESIAN_POINT ( 'NONE',  ( -104.2228709571500787, -23.47593901973090524, -1.443836447538996648 ) ) ;
#47964 = CARTESIAN_POINT ( 'NONE',  ( 17.27681320446407298, 11.92757687370068886, -1.500000000000002220 ) ) ;
#47965 = VERTEX_POINT ( 'NONE', #46832 ) ;
#47966 = CARTESIAN_POINT ( 'NONE',  ( -118.5228709571500758, -24.64965694238408034, 8.947790433994191162 ) ) ;
#47967 = CARTESIAN_POINT ( 'NONE',  ( -37.52287095715008292, -23.72773821059537269, 11.05748984161097326 ) ) ;
#47968 = CARTESIAN_POINT ( 'NONE',  ( -19.80875734969026425, -5.965225279485572685, 31.02402280011862246 ) ) ;
#47969 = CARTESIAN_POINT ( 'NONE',  ( -86.62887336595798615, -24.35071581493543391, 9.817618358456027039 ) ) ;
#47970 = CARTESIAN_POINT ( 'NONE',  ( -59.55363052684328551, -23.96119346886879597, -0.6495511937832131322 ) ) ;
#47971 = DIRECTION ( 'NONE',  ( -3.773278334444166432E-23, 1.000000000000000000, 0.000000000000000000 ) ) ;
#47972 = CARTESIAN_POINT ( 'NONE',  ( 2.499999999999988454, 22.00000000000000000, 0.000000000000000000 ) ) ;
#47974 = ORIENTED_EDGE ( 'NONE', *, *, #38773, .T. ) ;
#47973 = CARTESIAN_POINT ( 'NONE',  ( -21.66996937300057269, -4.939502015459471096, 11.49999999999999645 ) ) ;
#47975 = DIRECTION ( 'NONE',  ( -0.000000000000000000, -1.000000000000000000, -0.000000000000000000 ) ) ;
#47976 = CARTESIAN_POINT ( 'NONE',  ( -87.52287095715006160, -23.73907113217651599, -1.053371485781588124 ) ) ;
#47977 = VERTEX_POINT ( 'NONE', #87384 ) ;
#47978 = CARTESIAN_POINT ( 'NONE',  ( -15.33504971967173702, 16.71734053393862496, 11.49999999999998934 ) ) ;
#47979 = AXIS2_PLACEMENT_3D ( 'NONE', #48532, #57643, #40902 ) ;
#47981 = ORIENTED_EDGE ( 'NONE', *, *, #50040, .F. ) ;
#47980 = CARTESIAN_POINT ( 'NONE',  ( -87.62287095715004170, -24.66019654487199020, 8.947790411086129936 ) ) ;
#47982 = EDGE_CURVE ( 'NONE', #30802, #20834, #36240, .T. ) ;
#47983 = ORIENTED_EDGE ( 'NONE', *, *, #47496, .F. ) ;
#47984 = LINE ( 'NONE', #17525, #31944 ) ;
#47985 = AXIS2_PLACEMENT_3D ( 'NONE', #11474, #50053, #3386 ) ;
#47986 = CARTESIAN_POINT ( 'NONE',  ( 19.08902475966321788, 6.433202353099247262, 11.49999999999998934 ) ) ;
#47987 = CARTESIAN_POINT ( 'NONE',  ( 29.73860345376318293, -5.356774720514426491, 17.72811386545585322 ) ) ;
#47988 = VERTEX_POINT ( 'NONE', #79767 ) ;
#47989 = AXIS2_PLACEMENT_3D ( 'NONE', #25359, #18252, #33979 ) ;
#47990 = CARTESIAN_POINT ( 'NONE',  ( 15.52291915823243507, -3.595107466738250768, -28.22347026866546216 ) ) ;
#47991 = CARTESIAN_POINT ( 'NONE',  ( 11.21425909587273928, 19.38466839394011387, -1.500000000000002220 ) ) ;
#47992 = AXIS2_PLACEMENT_3D ( 'NONE', #90551, #91544, #67736 ) ;
#47993 = AXIS2_PLACEMENT_3D ( 'NONE', #49273, #88317, #57883 ) ;
#47994 = VERTEX_POINT ( 'NONE', #94495 ) ;
#47995 = ORIENTED_EDGE ( 'NONE', *, *, #37292, .T. ) ;
#47996 = CARTESIAN_POINT ( 'NONE',  ( 26.73860345374794178, 5.356774720496559894, 19.84760796525321780 ) ) ;
#47997 = CARTESIAN_POINT ( 'NONE',  ( -94.63646352547178253, -23.73791477778912196, 11.05961554403170588 ) ) ;
#47998 = CARTESIAN_POINT ( 'NONE',  ( -110.6228709571500701, -25.00182538069145011, 7.747789668545099317 ) ) ;
#47999 = CARTESIAN_POINT ( 'NONE',  ( 30.54636625424942764, 6.376774720514426065, 1.976438700016742045 ) ) ;
#48000 = VECTOR ( 'NONE', #8342, 1000.000000000000114 ) ;
#48002 = EDGE_CURVE ( 'NONE', #37139, #59253, #71671, .T. ) ;
#48001 = FACE_BOUND ( 'NONE', #46951, .T. ) ;
#48003 = CARTESIAN_POINT ( 'NONE',  ( -13.92019785312828972, -13.74635529968554515, -1.500000000000002220 ) ) ;
#48004 = CARTESIAN_POINT ( 'NONE',  ( -5.824076695599092801, -5.876774720514412742, 19.72913074730691108 ) ) ;
#48005 = EDGE_LOOP ( 'NONE', ( #20000, #37937, #46575, #90684 ) ) ;
#48006 = CARTESIAN_POINT ( 'NONE',  ( -0.9917595143200197416, 21.46465604038169772, 11.49999999999998934 ) ) ;
#48007 = CARTESIAN_POINT ( 'NONE',  ( -42.52287095715005449, -23.48786465467240347, 11.44779295918255180 ) ) ;
#48008 = CARTESIAN_POINT ( 'NONE',  ( -54.62287095715006302, -23.95044443724992078, 10.65354141964649592 ) ) ;
#48009 = CARTESIAN_POINT ( 'NONE',  ( -123.5228709571500758, -23.96177878511309345, 10.65340807706328441 ) ) ;
#48010 = EDGE_CURVE ( 'NONE', #39962, #20337, #67700, .T. ) ;
#48011 = DIRECTION ( 'NONE',  ( -0.000000000000000000, -1.000000000000000000, -0.000000000000000000 ) ) ;
#48012 = CARTESIAN_POINT ( 'NONE',  ( -20.38739128398232836, 10.50225141308550292, -1.500000000000002220 ) ) ;
#48013 = CALENDAR_DATE ( 2026, 9, 10 ) ;
#48014 = CARTESIAN_POINT ( 'NONE',  ( -93.62287095715004170, -23.48783264082478794, -1.443836473390063713 ) ) ;
#48015 = CARTESIAN_POINT ( 'NONE',  ( -53.59900199587650604, -23.96119346886879953, -0.6495511937832126881 ) ) ;
#48016 = CARTESIAN_POINT ( 'NONE',  ( 12.85705330080557829, 15.37097598829428513, 11.49999999999999645 ) ) ;
#48017 = CARTESIAN_POINT ( 'NONE',  ( -79.55512035851637620, -25.31594366164218712, 4.736589999760145275 ) ) ;
#48018 = CARTESIAN_POINT ( 'NONE',  ( 30.53060340732036693, 4.132774720514426292, -5.153186819891554471 ) ) ;
#48019 = CARTESIAN_POINT ( 'NONE',  ( 4.740341618695937065, -5.876774720514404748, 18.75174579344860248 ) ) ;
#48020 = CARTESIAN_POINT ( 'NONE',  ( 11.56983764158150407, -6.376774720514426953, 28.29037853177889517 ) ) ;
#48021 = B_SPLINE_CURVE_WITH_KNOTS ( 'NONE', 3,
 ( #48276, #94940, #56403, #95441 ),
 .UNSPECIFIED., .F., .F.,
 ( 4, 4 ),
 ( 0.4190663428356088405, 0.4200670898763741445 ),
 .UNSPECIFIED. ) ;
#48022 = DIRECTION ( 'NONE',  ( -0.5656310827093757876, -0.8246584009594636333, -1.161164194647626387E-16 ) ) ;
#48023 = CARTESIAN_POINT ( 'NONE',  ( -7.892909027492730267, -20.28523913882780505, -1.500000000000002220 ) ) ;
#48024 = FACE_OUTER_BOUND ( 'NONE', #52345, .T. ) ;
#48025 = CARTESIAN_POINT ( 'NONE',  ( 2.166912399371504705, 19.51343182558466793, -1.500000000000002220 ) ) ;
#48026 = CIRCLE ( 'NONE', #33449, 11.85241003308275864 ) ;
#48027 = CARTESIAN_POINT ( 'NONE',  ( -100.6228709571500559, -24.99132157543167310, 2.256160258750667502 ) ) ;
#48028 = CARTESIAN_POINT ( 'NONE',  ( -109.5669895805274336, -25.27925804186644498, 4.843009203900840554 ) ) ;
#48029 = CALENDAR_DATE ( 2026, 9, 10 ) ;
#48030 = DIRECTION ( 'NONE',  ( 1.000000000000000000, 3.773278334444166432E-23, 8.201307841325785021E-29 ) ) ;
#48031 = CARTESIAN_POINT ( 'NONE',  ( 2.590395174287518643, -5.876774720514416295, 20.05492615153064762 ) ) ;
#48032 = CARTESIAN_POINT ( 'NONE',  ( 0.1292827521129817636, -20.55975067039486603, 11.49999999999999645 ) ) ;
#48033 = CARTESIAN_POINT ( 'NONE',  ( 1.949999999999999956, -0.1925000000000001155, -0.1925000000000000600 ) ) ;
#48034 = CARTESIAN_POINT ( 'NONE',  ( -120.6241461665311192, -24.83618233451451118, 1.606449574219542598 ) ) ;
#48035 = CARTESIAN_POINT ( 'NONE',  ( -3.801653518169780366, -22.29579330195574016, 11.49999999999999645 ) ) ;
#48036 = ORIENTED_EDGE ( 'NONE', *, *, #55296, .F. ) ;
#48037 = CARTESIAN_POINT ( 'NONE',  ( -70.03562343076868046, -25.12219137083621590, 7.066379050738610168 ) ) ;
#48038 = CARTESIAN_POINT ( 'NONE',  ( 0.4325450954222598288, 2.877919977996279827E-16, -2.350000000000000089 ) ) ;
#48039 = CARTESIAN_POINT ( 'NONE',  ( -125.5888992149329653, -24.92592662359561828, 8.075495903018000021 ) ) ;
#48040 = CARTESIAN_POINT ( 'NONE',  ( -0.02075734969026423599, 3.316774720514426456, -0.08597719988137648983 ) ) ;
#48041 = CARTESIAN_POINT ( 'NONE',  ( -33.62287095715005592, -23.47593901973091235, -1.443836447539013301 ) ) ;
#48042 = CARTESIAN_POINT ( 'NONE',  ( 4.878909776184770742E-15, -5.876774720514426953, 22.50000000000000355 ) ) ;
#48043 = AXIS2_PLACEMENT_3D ( 'NONE', #55119, #8931, #54125 ) ;
#48044 = VERTEX_POINT ( 'NONE', #33102 ) ;
#48045 = CARTESIAN_POINT ( 'NONE',  ( -79.34938298551102775, -25.26750068962975604, 5.853656373955819170 ) ) ;
#48046 = CARTESIAN_POINT ( 'NONE',  ( 22.79674358141071977, 1.614764915196592598, -1.500000000000002220 ) ) ;
#48047 = CARTESIAN_POINT ( 'NONE',  ( 4.486687842132109694, -5.876774720514410077, 18.98221446873611029 ) ) ;
#48048 = CARTESIAN_POINT ( 'NONE',  ( -96.62549120092178612, -24.51314013834316086, 0.6176544820404182845 ) ) ;
#48049 = CARTESIAN_POINT ( 'NONE',  ( -63.54868262085074093, -24.15620529776628089, 10.23563542870660470 ) ) ;
#48050 = CARTESIAN_POINT ( 'NONE',  ( 5.133194422563156500, 21.89913303424002677, 11.49999999999999645 ) ) ;
#48051 = ORIENTED_EDGE ( 'NONE', *, *, #57111, .F. ) ;
#48052 = DIRECTION ( 'NONE',  ( 0.000000000000000000, 0.000000000000000000, -1.000000000000000000 ) ) ;
#48053 = CARTESIAN_POINT ( 'NONE',  ( -13.81295463269534096, 17.03802364079049525, 11.49999999999998934 ) ) ;
#48054 = CARTESIAN_POINT ( 'NONE',  ( -127.4728709571500360, -25.40558663563398767, 5.000950440326727531 ) ) ;
#48055 = AXIS2_PLACEMENT_3D ( 'NONE', #80204, #39634, #41655 ) ;
#48056 = CARTESIAN_POINT ( 'NONE',  ( -34.55278932522879387, -23.96169478059712077, 10.65365249895718769 ) ) ;
#48057 = CARTESIAN_POINT ( 'NONE',  ( -121.5228709571500474, -23.95044443724993144, 10.65354141964648704 ) ) ;
#48058 = ORIENTED_EDGE ( 'NONE', *, *, #76677, .F. ) ;
#48059 = CARTESIAN_POINT ( 'NONE',  ( -116.6228709571500417, -24.66019654487199730, 8.947790411086121054 ) ) ;
#48060 = CARTESIAN_POINT ( 'NONE',  ( 14.76093561896379214, 5.965225279485572685, -26.55548769130089681 ) ) ;
#48061 = ORIENTED_EDGE ( 'NONE', *, *, #4355, .T. ) ;
#48062 = VECTOR ( 'NONE', #71028, 1000.000000000000000 ) ;
#48063 = EDGE_CURVE ( 'NONE', #623, #39855, #91936, .T. ) ;
#48064 = CARTESIAN_POINT ( 'NONE',  ( -9.379331868514380943, 18.20734191464070406, -1.500000000000002220 ) ) ;
#48065 = ORIENTED_EDGE ( 'NONE', *, *, #12644, .F. ) ;
#48066 = AXIS2_PLACEMENT_3D ( 'NONE', #21461, #20474, #28599 ) ;
#48067 = VERTEX_POINT ( 'NONE', #23975 ) ;
#48068 = VERTEX_POINT ( 'NONE', #64080 ) ;
#48069 = VERTEX_POINT ( 'NONE', #94995 ) ;
#48070 = CARTESIAN_POINT ( 'NONE',  ( 19.40787663092975279, -12.54570180764831377, 11.49999999999998934 ) ) ;
#48071 = FACE_OUTER_BOUND ( 'NONE', #87493, .T. ) ;
#48072 = CARTESIAN_POINT ( 'NONE',  ( 6.844040470191356640, -19.11863935190610064, -1.500000000000002220 ) ) ;
#48073 = EDGE_CURVE ( 'NONE', #47456, #57568, #9636, .T. ) ;
#48074 = VERTEX_POINT ( 'NONE', #73174 ) ;
#48075 = PLANE ( 'NONE',  #73634 ) ;
#48076 = CARTESIAN_POINT ( 'NONE',  ( -92.51846584691269015, -23.73766607897670866, -1.055555164236430032 ) ) ;
#48077 = CIRCLE ( 'NONE', #86951, 22.69500000000000384 ) ;
#48078 = ADVANCED_FACE ( 'NONE', ( #96002 ), #88392, .F. ) ;
#48079 = CARTESIAN_POINT ( 'NONE',  ( -93.62287095715007013, -24.33927499327855415, 9.819080762295811837 ) ) ;
#48080 = CARTESIAN_POINT ( 'NONE',  ( 4.613443512364428400, -6.376774720514411854, 19.38647409819875733 ) ) ;
#48082 = VERTEX_POINT ( 'NONE', #12746 ) ;
#48081 = CARTESIAN_POINT ( 'NONE',  ( 5.543860000110784725, 20.76261553274053284, 11.49999999999999645 ) ) ;
#48083 = CARTESIAN_POINT ( 'NONE',  ( -75.63649189368283032, -24.40034930558991633, 0.3402023900116103450 ) ) ;
#48084 = CARTESIAN_POINT ( 'NONE',  ( -112.6228709571500559, -24.64898659630368272, 1.056161002820831474 ) ) ;
#48085 = EDGE_CURVE ( 'NONE', #14129, #82898, #44683, .T. ) ;
#48086 = VERTEX_POINT ( 'NONE', #89886 ) ;
#48087 = EDGE_CURVE ( 'NONE', #65800, #41620, #96803, .T. ) ;
#48088 = CARTESIAN_POINT ( 'NONE',  ( 10.28901978357889035, -18.02705789925236957, -1.500000000000002220 ) ) ;
#48089 = ORIENTED_EDGE ( 'NONE', *, *, #86604, .T. ) ;
#48091 = ORIENTED_EDGE ( 'NONE', *, *, #29190, .T. ) ;
#48090 = CARTESIAN_POINT ( 'NONE',  ( -125.5200017711960783, -24.63355581998386512, 0.9682620441944075340 ) ) ;
#48092 = DIRECTION ( 'NONE',  ( -0.000000000000000000, -1.000000000000000000, -0.000000000000000000 ) ) ;
#48093 = CARTESIAN_POINT ( 'NONE',  ( -53.52287095715004739, -23.73907113216989373, -1.053371485793253237 ) ) ;
#48094 = EDGE_LOOP ( 'NONE', ( #87316, #34613, #35755, #35185 ) ) ;
#48095 = ORIENTED_EDGE ( 'NONE', *, *, #83082, .T. ) ;
#48096 = CARTESIAN_POINT ( 'NONE',  ( -48.52287095715007581, -23.47593901973090524, -1.443836447538997314 ) ) ;
#48097 = CARTESIAN_POINT ( 'NONE',  ( -42.49911757110140798, -24.15620529776627734, 10.23563542870661358 ) ) ;
#48098 = EDGE_CURVE ( 'NONE', #35626, #17176, #95539, .T. ) ;
#48099 = DIRECTION ( 'NONE',  ( -1.000000000000000000, -3.773278334444166432E-23, -8.201307841325785021E-29 ) ) ;
#48101 = ORIENTED_EDGE ( 'NONE', *, *, #60245, .F. ) ;
#48100 = CARTESIAN_POINT ( 'NONE',  ( 7.103389721457689099, 20.86620700561973862, 11.49999999999999645 ) ) ;
#48102 = DIRECTION ( 'NONE',  ( 0.000000000000000000, 0.000000000000000000, 1.000000000000000000 ) ) ;
#48103 = CARTESIAN_POINT ( 'NONE',  ( -9.785633969878258398, 20.35780147342342516, 11.49999999999998934 ) ) ;
#48104 = VECTOR ( 'NONE', #47580, 1000.000000000000114 ) ;
#48105 = CARTESIAN_POINT ( 'NONE',  ( -7.324709186033012465, -19.69651249574825513, -1.500000000000002220 ) ) ;
#48107 = ORIENTED_EDGE ( 'NONE', *, *, #34498, .F. ) ;
#48106 = DIRECTION ( 'NONE',  ( -0.6451914333552788428, 0.000000000000000000, -0.7640209514960702997 ) ) ;
#48108 = ORIENTED_EDGE ( 'NONE', *, *, #7647, .T. ) ;
#48109 = CIRCLE ( 'NONE', #39982, 252.4458649670781085 ) ;
#48110 = LINE ( 'NONE', #2430, #14235 ) ;
#48111 = DIRECTION ( 'NONE',  ( 0.02119372647572909107, 0.000000000000000000, 0.9997753877537054468 ) ) ;
#48112 = ORIENTED_EDGE ( 'NONE', *, *, #63457, .T. ) ;
#48113 = CARTESIAN_POINT ( 'NONE',  ( 14.81885032312887240, -15.09863332352077592, 11.49999999999998934 ) ) ;
#48114 = CARTESIAN_POINT ( 'NONE',  ( -66.62287095715002749, -24.33927499327853639, 9.819080762295815390 ) ) ;
#48115 = CARTESIAN_POINT ( 'NONE',  ( -58.85574863676698953, -25.33009847151394922, 4.495758292450050320 ) ) ;
#48116 = DIRECTION ( 'NONE',  ( 0.000000000000000000, 0.000000000000000000, 1.000000000000000000 ) ) ;
#48117 = CARTESIAN_POINT ( 'NONE',  ( -7.064692883725313344, -6.376774720514411854, 19.55266968305501862 ) ) ;
#48118 = LINE ( 'NONE', #39497, #16226 ) ;
#48119 = CARTESIAN_POINT ( 'NONE',  ( -13.56020932195406203, -17.60290058955388659, -1.500000000000002220 ) ) ;
#48120 = CARTESIAN_POINT ( 'NONE',  ( -114.6292325214853491, -23.73766607897672287, -1.055555164236428700 ) ) ;
#48121 = ADVANCED_FACE ( 'NONE', ( #19860 ), #49345, .F. ) ;
#48122 = VERTEX_POINT ( 'NONE', #43717 ) ;
#48123 = CARTESIAN_POINT ( 'NONE',  ( -5.554587162835583847, -6.376774720514417183, 19.99258394656885329 ) ) ;
#48124 = CARTESIAN_POINT ( 'NONE',  ( -37.58686907815667411, -24.34968618360933590, 0.1864209137778856384 ) ) ;
#48125 = CARTESIAN_POINT ( 'NONE',  ( 0.000000000000000000, -2.056774720514426669, 0.000000000000000000 ) ) ;
#48126 = VECTOR ( 'NONE', #39383, 1000.000000000000114 ) ;
#48127 = CARTESIAN_POINT ( 'NONE',  ( -41.80098236575750548, -25.24187400068776554, 3.756537540763403182 ) ) ;
#48128 = CARTESIAN_POINT ( 'NONE',  ( 13.57151214508650305, -0.8999999999999998002, 0.000000000000000000 ) ) ;
#48129 = CARTESIAN_POINT ( 'NONE',  ( -12.17249226084429203, 15.20430173202493940, -1.500000000000002220 ) ) ;
#48130 = CARTESIAN_POINT ( 'NONE',  ( -20.78045986758521835, -5.208592277829342088, -1.500000000000002220 ) ) ;
#48131 = DIRECTION ( 'NONE',  ( 0.9161084732596779245, 5.365801633547218220E-16, -0.4009304992412300317 ) ) ;
#48132 = LINE ( 'NONE', #35888, #9087 ) ;
#48133 = CARTESIAN_POINT ( 'NONE',  ( -51.62368720275268430, -24.65952944569304250, 1.056160979905695463 ) ) ;
#48134 = CARTESIAN_POINT ( 'NONE',  ( -100.5840138597264826, -25.27359975741654807, 3.299225944038700398 ) ) ;
#48135 = CARTESIAN_POINT ( 'NONE',  ( -21.69093436787670726, -6.948586514802197023, -1.500000000000002220 ) ) ;
#48136 = VECTOR ( 'NONE', #67788, 999.9999999999998863 ) ;
#48137 = ADVANCED_FACE ( 'NONE', ( #20355 ), #65085, .T. ) ;
#48138 = AXIS2_PLACEMENT_3D ( 'NONE', #8525, #48099, #40480 ) ;
#48139 = CARTESIAN_POINT ( 'NONE',  ( -99.52287095715006160, -23.47596703998600631, 11.44779298504228215 ) ) ;
#48140 = CARTESIAN_POINT ( 'NONE',  ( -106.5228709571500758, -24.64965694238408034, 8.947790433994192938 ) ) ;
#48141 = CARTESIAN_POINT ( 'NONE',  ( -15.96263503330635380, 11.84234753045382682, 11.49999999999999645 ) ) ;
#48142 = CARTESIAN_POINT ( 'NONE',  ( -84.52287095715006160, -23.96127896941631974, -0.6493128931038028018 ) ) ;
#48143 = AXIS2_PLACEMENT_3D ( 'NONE', #51341, #98489, #28990 ) ;
#48144 = CARTESIAN_POINT ( 'NONE',  ( -112.6228709571500559, -23.47596703998600631, 11.44779298504227860 ) ) ;
#48145 = CARTESIAN_POINT ( 'NONE',  ( -65.22287095715006444, -23.47593901973090169, -1.443836447538997536 ) ) ;
#48146 = ORIENTED_EDGE ( 'NONE', *, *, #12471, .F. ) ;
#48147 = CARTESIAN_POINT ( 'NONE',  ( 22.02124265030973760, 7.743225279485574042, 16.20402280011862217 ) ) ;
#48148 = EDGE_CURVE ( 'NONE', #13213, #3403, #14475, .T. ) ;
#48149 = CARTESIAN_POINT ( 'NONE',  ( -6.602379858799704238, -5.876774720514410077, 19.46575348430202723 ) ) ;
#48150 = CARTESIAN_POINT ( 'NONE',  ( -28.98875734969026396, 5.965225279485572685, 2.362022800118626531 ) ) ;
#48151 = CARTESIAN_POINT ( 'NONE',  ( -21.58526226860004371, 1.989002153404973328, -1.500000000000002220 ) ) ;
#48152 = CARTESIAN_POINT ( 'NONE',  ( -84.52287095715007581, -24.66019654487199730, 8.947790411086122830 ) ) ;
#48153 = CARTESIAN_POINT ( 'NONE',  ( 13.27039818535887505, -14.28956163997708906, -1.500000000000002220 ) ) ;
#48154 = DIRECTION ( 'NONE',  ( 0.000000000000000000, 0.9999999999976377785, 2.173523156925979975E-06 ) ) ;
#48155 = ORIENTED_EDGE ( 'NONE', *, *, #74122, .F. ) ;
#48156 = CARTESIAN_POINT ( 'NONE',  ( -5.548086588741434788, -19.59138962566686004, 11.49999999999999645 ) ) ;
#48157 = CARTESIAN_POINT ( 'NONE',  ( -28.98875734969026041, -5.965225279485572685, 15.62202280011862321 ) ) ;
#48158 = DIRECTION ( 'NONE',  ( 0.000000000000000000, -1.000000000000000000, 0.000000000000000000 ) ) ;
#48159 = EDGE_LOOP ( 'NONE', ( #54681, #16222, #82183, #65211, #65532, #97602, #11525, #40872, #91863, #30873, #45993 ) ) ;
#48160 = CYLINDRICAL_SURFACE ( 'NONE', #26518, 1.249999999999997113 ) ;
#48161 = CARTESIAN_POINT ( 'NONE',  ( 33.41145047975789595, 4.538943570064395416, -12.61568413423384172 ) ) ;
#48162 = CARTESIAN_POINT ( 'NONE',  ( -39.36780865613509661, -25.31628669946116617, 5.233841552006910369 ) ) ;
#48163 = FACE_OUTER_BOUND ( 'NONE', #96322, .T. ) ;
#48164 = DIRECTION ( 'NONE',  ( -3.773278334453079030E-23, 0.9999999999976377785, 2.173523156925979128E-06 ) ) ;
#48165 = CARTESIAN_POINT ( 'NONE',  ( 19.99232773509726258, 2.034096180923423702, 11.49999999999998934 ) ) ;
#48166 = CARTESIAN_POINT ( 'NONE',  ( -24.90875734969025501, 5.965225279485572685, 30.00402280011862288 ) ) ;
#48167 = EDGE_LOOP ( 'NONE', ( #95719, #68371, #12476, #87663 ) ) ;
#48168 = PLANE ( 'NONE',  #85281 ) ;
#48169 = AXIS2_PLACEMENT_3D ( 'NONE', #67065, #29971, #98977 ) ;
#48170 = CARTESIAN_POINT ( 'NONE',  ( 19.00551534866085746, 12.86435971046890359, 11.49999999999999645 ) ) ;
#48171 = CARTESIAN_POINT ( 'NONE',  ( -2.780358639097238349, 22.57001311929844434, 11.49999999999998934 ) ) ;
#48172 = ORIENTED_EDGE ( 'NONE', *, *, #95, .F. ) ;
#48173 = CARTESIAN_POINT ( 'NONE',  ( -30.47287095715007510, -23.47596699454220470, 11.42688508591989560 ) ) ;
#48174 = B_SPLINE_CURVE_WITH_KNOTS ( 'NONE', 3,
 ( #38563, #23828, #10993, #26719, #69518, #100420, #46686, #58668 ),
 .UNSPECIFIED., .F., .F.,
 ( 4, 2, 2, 4 ),
 ( -0.001240666984355842791, -0.0002401179793395018334, 0.0007604310256768391247, 0.002761529035709520824 ),
 .UNSPECIFIED. ) ;
#48175 = CARTESIAN_POINT ( 'NONE',  ( -98.52287095715000476, -23.73907113216990084, -1.053371485793250351 ) ) ;
#48176 = CARTESIAN_POINT ( 'NONE',  ( -90.54958004235005831, -24.40034930558990922, 0.3402023900116079580 ) ) ;
#48177 = VECTOR ( 'NONE', #11427, 1000.000000000000000 ) ;
#48178 = CARTESIAN_POINT ( 'NONE',  ( -61.24303164512834030, -25.04307381209219230, 7.563174986197129357 ) ) ;
#48179 = CARTESIAN_POINT ( 'NONE',  ( -69.54471688719442568, -24.35071581493542681, 9.817618358456032368 ) ) ;
#48180 = DIRECTION ( 'NONE',  ( -0.7071067811865476838, 0.000000000000000000, 0.7071067811865474617 ) ) ;
#48181 = CARTESIAN_POINT ( 'NONE',  ( -122.5185787333176108, -24.65952944569305316, 1.056160979905708786 ) ) ;
#48182 = CARTESIAN_POINT ( 'NONE',  ( -58.55986403960651643, -23.73766607897670156, -1.055555164236457344 ) ) ;
#48183 = VERTEX_POINT ( 'NONE', #51329 ) ;
#48184 = CARTESIAN_POINT ( 'NONE',  ( -6.692510123977180925, 19.25193956699996178, -1.500000000000002220 ) ) ;
#48185 = ORIENTED_EDGE ( 'NONE', *, *, #79345, .T. ) ;
#48186 = ORIENTED_EDGE ( 'NONE', *, *, #63416, .T. ) ;
#48187 = CARTESIAN_POINT ( 'NONE',  ( -19.49525799874905729, 12.17417675796824561, -1.500000000000002220 ) ) ;
#48188 = CARTESIAN_POINT ( 'NONE',  ( -39.52287095715008292, -23.48783264082476308, -1.443836473390098574 ) ) ;
#48189 = ORIENTED_EDGE ( 'NONE', *, *, #91344, .F. ) ;
#48190 = DIRECTION ( 'NONE',  ( -0.4009304992412306978, 6.454799914155190814E-16, -0.9161084732596777025 ) ) ;
#48191 = CIRCLE ( 'NONE', #64369, 2.899999999999999467 ) ;
#48192 = CARTESIAN_POINT ( 'NONE',  ( -86.62287095715004170, -29.50248528299804818, 1.056150453629040253 ) ) ;
#48193 = CARTESIAN_POINT ( 'NONE',  ( 1.095236984349686971, 8.494825072090639750, 1.700000000000008837 ) ) ;
#48194 = CARTESIAN_POINT ( 'NONE',  ( -119.4337121810133198, -25.30063765797860498, 5.393961676144591877 ) ) ;
#48196 = ORIENTED_EDGE ( 'NONE', *, *, #32145, .T. ) ;
#48195 = CARTESIAN_POINT ( 'NONE',  ( -14.61619677566029729, 15.53698580111986693, 11.49999999999999645 ) ) ;
#48197 = EDGE_CURVE ( 'NONE', #49615, #36274, #19949, .T. ) ;
#48198 = ORIENTED_EDGE ( 'NONE', *, *, #25508, .F. ) ;
#48199 = CARTESIAN_POINT ( 'NONE',  ( -13.56020932195406203, -17.60290058955388659, 11.49999999999998934 ) ) ;
#48200 = EDGE_CURVE ( 'NONE', #26747, #39067, #73665, .T. ) ;
#48201 = CARTESIAN_POINT ( 'NONE',  ( -10.67548511050313209, -17.69376651829569269, 11.49999999999998934 ) ) ;
#48202 = AXIS2_PLACEMENT_3D ( 'NONE', #26845, #19714, #57812 ) ;
#48203 = VERTEX_POINT ( 'NONE', #5149 ) ;
#48204 = CARTESIAN_POINT ( 'NONE',  ( -6.775140224358976226, -5.876774720514408301, 19.14743589743590846 ) ) ;
#48205 = CARTESIAN_POINT ( 'NONE',  ( -95.63507531277841167, -24.15602025860896163, 10.28564288303536856 ) ) ;
#48206 = ORIENTED_EDGE ( 'NONE', *, *, #11963, .T. ) ;
#48207 = CARTESIAN_POINT ( 'NONE',  ( -95.52287095715006160, -24.99132157543166954, 2.256160258750667502 ) ) ;
#48208 = AXIS2_PLACEMENT_3D ( 'NONE', #98130, #90039, #44870 ) ;
#48209 = ORIENTED_EDGE ( 'NONE', *, *, #87257, .T. ) ;
#48210 = CARTESIAN_POINT ( 'NONE',  ( 6.646494591716556322, -3.316774720514426900, -28.33840132637671161 ) ) ;
#48211 = CARTESIAN_POINT ( 'NONE',  ( -70.38569055212785486, -25.12330845317594807, 7.099802567542052856 ) ) ;
#48212 = CARTESIAN_POINT ( 'NONE',  ( -19.85847575633505713, -6.422239212204448044, -1.500000000000002220 ) ) ;
#48213 = ADVANCED_FACE ( 'NONE', ( #42243 ), #65409, .T. ) ;
#48214 = CARTESIAN_POINT ( 'NONE',  ( -20.57666286913221754, 7.287794730890116313, 11.49999999999999645 ) ) ;
#48215 = CARTESIAN_POINT ( 'NONE',  ( -102.6228709571500701, -24.66019654487199730, 8.947790411086121054 ) ) ;
#48216 = CARTESIAN_POINT ( 'NONE',  ( 15.32643653063177958, 3.577630190450218350, -27.14485409495429380 ) ) ;
#48217 = CARTESIAN_POINT ( 'NONE',  ( 8.413247042826936806, 20.86129769029627923, -1.500000000000002220 ) ) ;
#48218 = CARTESIAN_POINT ( 'NONE',  ( -118.5566399574894945, -23.73791477778912551, 11.05961554403169878 ) ) ;
#48219 = CARTESIAN_POINT ( 'NONE',  ( -29.49875734969026198, 0.3587747205144262708, 7.870022800118625206 ) ) ;
#48220 = CARTESIAN_POINT ( 'NONE',  ( 2.899999999999999467, 33.29999999999999716, 0.000000000000000000 ) ) ;
#48221 = ORIENTED_EDGE ( 'NONE', *, *, #41708, .T. ) ;
#48222 = ORIENTED_EDGE ( 'NONE', *, *, #15520, .T. ) ;
#48223 = VERTEX_POINT ( 'NONE', #4659 ) ;
#48224 = CARTESIAN_POINT ( 'NONE',  ( -35.62287095715005592, -25.00182538069145011, 7.747789668545097541 ) ) ;
#48225 = ORIENTED_EDGE ( 'NONE', *, *, #68929, .F. ) ;
#48226 = CARTESIAN_POINT ( 'NONE',  ( -13.99230614532761052, -16.21612836239924960, -1.500000000000002220 ) ) ;
#48227 = CARTESIAN_POINT ( 'NONE',  ( -11.14805103425725719, -19.39388463112642214, 11.49999999999999645 ) ) ;
#48228 = ORIENTED_EDGE ( 'NONE', *, *, #12820, .T. ) ;
#48229 = CARTESIAN_POINT ( 'NONE',  ( 0.000000000000000000, 2.682774720514426559, 0.000000000000000000 ) ) ;
#48230 = CARTESIAN_POINT ( 'NONE',  ( 20.15827220212406701, 6.050813824765241655, -1.500000000000002220 ) ) ;
#48231 = CARTESIAN_POINT ( 'NONE',  ( -30.42284766947733488, -24.74885280525437992, 8.640462295247351321 ) ) ;
#48232 = CARTESIAN_POINT ( 'NONE',  ( -3.169371320753151977, 19.67850563098683736, -1.500000000000002220 ) ) ;
#48233 = CARTESIAN_POINT ( 'NONE',  ( -117.6228709571500559, -23.96127896941633750, -0.6493128931037767115 ) ) ;
#48234 = DIRECTION ( 'NONE',  ( 0.000000000000000000, 0.000000000000000000, -1.000000000000000000 ) ) ;
#48235 = CARTESIAN_POINT ( 'NONE',  ( -21.77411086464670831, -3.637377321037103872, -1.500000000000002220 ) ) ;
#48236 = EDGE_LOOP ( 'NONE', ( #84612, #44254, #44770, #74139 ) ) ;
#48237 = CARTESIAN_POINT ( 'NONE',  ( -116.5567473932748044, -23.73766607897671577, -1.055555164236427812 ) ) ;
#48238 = DIRECTION ( 'NONE',  ( 0.000000000000000000, 0.000000000000000000, 1.000000000000000000 ) ) ;
#48239 = CARTESIAN_POINT ( 'NONE',  ( -18.77111393065419875, 9.022841878967760465, 11.49999999999999645 ) ) ;
#48240 = AXIS2_PLACEMENT_3D ( 'NONE', #32225, #71808, #63201 ) ;
#48241 = EDGE_CURVE ( 'NONE', #93369, #10565, #58000, .T. ) ;
#48242 = DIRECTION ( 'NONE',  ( 0.000000000000000000, -1.000000000000000000, 0.000000000000000000 ) ) ;
#48243 = DIRECTION ( 'NONE',  ( 0.000000000000000000, 0.9999999999976377785, 2.173523156925979128E-06 ) ) ;
#48244 = VECTOR ( 'NONE', #3592, 1000.000000000000000 ) ;
#48245 = CARTESIAN_POINT ( 'NONE',  ( -48.52287095715007581, -23.47593901973090524, -1.443836447538997314 ) ) ;
#48246 = CARTESIAN_POINT ( 'NONE',  ( -20.14006130340733236, -7.001243683211865410, 11.49999999999998934 ) ) ;
#48247 = CARTESIAN_POINT ( 'NONE',  ( -40.52287095715005449, -29.50248789122583659, 2.256150453626215580 ) ) ;
#48248 = CARTESIAN_POINT ( 'NONE',  ( -50.45707490627877689, -25.19522716123442407, 3.295339427985402025 ) ) ;
#48249 = EDGE_CURVE ( 'NONE', #80353, #40608, #73795, .T. ) ;
#48250 = CARTESIAN_POINT ( 'NONE',  ( -128.5228709571500758, -23.47593901973090524, -1.443836447538996204 ) ) ;
#48251 = CARTESIAN_POINT ( 'NONE',  ( -69.99341794969650721, -25.22594453560301631, 6.517383687127669134 ) ) ;
#48252 = CARTESIAN_POINT ( 'NONE',  ( -22.55165446212525993, 1.111233042438415808, -1.500000000000002220 ) ) ;
#48253 = B_SPLINE_SURFACE_WITH_KNOTS ( 'NONE', 3, 3, ( 
 ( #77869, #94104, #31715, #69784 ),
 ( #47445, #7368, #84995, #84500 ),
 ( #78869, #39320, #71283, #93103 ),
 ( #38821, #32709, #63180, #93598 ),
 ( #23584, #16982, #261, #9370 ),
 ( #54554, #78373, #24591, #69280 ),
 ( #16474, #1277, #8878, #63691 ) ),
 .UNSPECIFIED., .F., .F., .F.,
 ( 4, 3, 4 ),
 ( 4, 4 ),
 ( 0.0004766839783817236630, 0.1029713700210892063, 0.2054660560637966982 ),
 ( 0.8597126934696902589, 0.8611220878828262926 ),
 .UNSPECIFIED. ) ;
#48254 = PLANE ( 'NONE',  #44153 ) ;
#48255 = ORIENTED_EDGE ( 'NONE', *, *, #66085, .T. ) ;
#48256 = CARTESIAN_POINT ( 'NONE',  ( -51.48758594601332561, -25.28167085146487381, 5.912859751850549905 ) ) ;
#48257 = CARTESIAN_POINT ( 'NONE',  ( -31.63563380732087893, -24.35071581493542325, 9.817618358456039473 ) ) ;
#48258 = CARTESIAN_POINT ( 'NONE',  ( 14.14096853472169535, -13.71769858867784464, 11.49999999999999645 ) ) ;
#48259 = CARTESIAN_POINT ( 'NONE',  ( -49.52287095715004739, -24.33832256527048798, 0.1851278514138550435 ) ) ;
#48260 = CARTESIAN_POINT ( 'NONE',  ( 14.45468597507908903, -3.471643246632547974, -28.36588305008921651 ) ) ;
#48261 = ORIENTED_EDGE ( 'NONE', *, *, #95135, .F. ) ;
#48262 = CARTESIAN_POINT ( 'NONE',  ( -111.5228709571501042, -23.72747288104470087, -1.053458166803224794 ) ) ;
#48263 = CARTESIAN_POINT ( 'NONE',  ( -99.52764846858842418, -29.50249168100820896, 3.999763059310747160 ) ) ;
#48264 = CARTESIAN_POINT ( 'NONE',  ( -124.5206801752270422, -24.15620529776629510, 10.23563542870659404 ) ) ;
#48265 = AXIS2_PLACEMENT_3D ( 'NONE', #28901, #12671, #97415 ) ;
#48266 = LINE ( 'NONE', #79197, #33353 ) ;
#48267 = CARTESIAN_POINT ( 'NONE',  ( -57.62287095715004881, -23.47593901973091235, -1.443836447539007972 ) ) ;
#48268 = CARTESIAN_POINT ( 'NONE',  ( 18.87426695099163254, 5.791883100666666451, 11.49999999999998934 ) ) ;
#48269 = VERTEX_POINT ( 'NONE', #13743 ) ;
#48270 = CARTESIAN_POINT ( 'NONE',  ( 18.20877288740043198, -8.745817889818592761, 11.49999999999999645 ) ) ;
#48271 = CARTESIAN_POINT ( 'NONE',  ( -7.421417143192116761, -5.876774720514411854, 19.43823095447975291 ) ) ;
#48272 = EDGE_CURVE ( 'NONE', #53585, #85354, #14242, .T. ) ;
#48273 = VECTOR ( 'NONE', #17366, 1000.000000000000000 ) ;
#48274 = ORIENTED_EDGE ( 'NONE', *, *, #35696, .T. ) ;
#48275 = PLANE ( 'NONE',  #41056 ) ;
#48276 = CARTESIAN_POINT ( 'NONE',  ( -72.52287095715007581, -23.47596703998600631, 11.44779298504228748 ) ) ;
#48277 = DIRECTION ( 'NONE',  ( -3.773278334453079030E-23, 0.9999999999976377785, 2.173523156925979128E-06 ) ) ;
#48278 = PLANE ( 'NONE',  #25677 ) ;
#48279 = CIRCLE ( 'NONE', #38557, 2.249999999999998668 ) ;
#48280 = CARTESIAN_POINT ( 'NONE',  ( -103.6228709571500559, -24.64965695001469115, 8.947790433994178727 ) ) ;
#48281 = B_SPLINE_CURVE_WITH_KNOTS ( 'NONE', 3,
 ( #74788, #11408, #36739, #20012 ),
 .UNSPECIFIED., .F., .F.,
 ( 4, 4 ),
 ( 0.6192157509887148414, 0.6202164980294804231 ),
 .UNSPECIFIED. ) ;
#48282 = DIRECTION ( 'NONE',  ( 3.773278334444166432E-23, -1.000000000000000000, 0.000000000000000000 ) ) ;
#48283 = CARTESIAN_POINT ( 'NONE',  ( 1.468936567494551593, -19.95401460376903913, -1.500000000000002220 ) ) ;
#48284 = DIRECTION ( 'NONE',  ( 0.000000000000000000, 0.9999999999976377785, 2.173523156925979128E-06 ) ) ;
#48285 = LINE ( 'NONE', #25434, #46802 ) ;
#48286 = ORIENTED_EDGE ( 'NONE', *, *, #10026, .T. ) ;
#48287 = EDGE_CURVE ( 'NONE', #6012, #11676, #87091, .T. ) ;
#48288 = FACE_OUTER_BOUND ( 'NONE', #97763, .T. ) ;
#48289 = DIRECTION ( 'NONE',  ( 0.000000000000000000, -2.173523156925980399E-06, 0.9999999999976378895 ) ) ;
#48290 = FACE_OUTER_BOUND ( 'NONE', #24181, .T. ) ;
#48291 = CARTESIAN_POINT ( 'NONE',  ( -117.7765869487822812, -25.31326647857923362, 3.500947721614712016 ) ) ;
#48292 = CARTESIAN_POINT ( 'NONE',  ( -83.59538777415443178, -23.96119346886880308, -0.6495511937832110227 ) ) ;
#48293 = CARTESIAN_POINT ( 'NONE',  ( -9.299999999999991829, 12.00000000000002309, 2.100000000000000089 ) ) ;
#48294 = CARTESIAN_POINT ( 'NONE',  ( -100.9392423175550988, -25.11539320716599732, 2.804431449967498491 ) ) ;
#48295 = ORIENTED_EDGE ( 'NONE', *, *, #41073, .T. ) ;
#48296 = B_SPLINE_CURVE_WITH_KNOTS ( 'NONE', 3,
 ( #46782, #40174, #10221, #87336 ),
 .UNSPECIFIED., .F., .F.,
 ( 4, 4 ),
 ( 0.000000000000000000, 9.999999999998897304E-05 ),
 .UNSPECIFIED. ) ;
#48297 = CARTESIAN_POINT ( 'NONE',  ( 16.58868386459195676, 11.68684615565071283, -1.500000000000002220 ) ) ;
#48298 = ADVANCED_FACE ( 'NONE', ( #98980 ), #22843, .F. ) ;
#48299 = EDGE_CURVE ( 'NONE', #42265, #98447, #59244, .T. ) ;
#48300 = PLANE ( 'NONE',  #32312 ) ;
#48301 = CARTESIAN_POINT ( 'NONE',  ( -34.62287095715005592, -24.64898659630367206, 1.056161002820817485 ) ) ;
#48302 = FACE_OUTER_BOUND ( 'NONE', #77148, .T. ) ;
#48303 = ORIENTED_EDGE ( 'NONE', *, *, #93676, .T. ) ;
#48304 = DIRECTION ( 'NONE',  ( 0.000000000000000000, -1.000000000000000000, 0.000000000000000000 ) ) ;
#48305 = B_SPLINE_CURVE_WITH_KNOTS ( 'NONE', 3,
 ( #24428, #8716, #47782, #25935 ),
 .UNSPECIFIED., .F., .F.,
 ( 4, 4 ),
 ( 0.000000000000000000, 9.999999999998897304E-05 ),
 .UNSPECIFIED. ) ;
#48306 = CARTESIAN_POINT ( 'NONE',  ( -20.44436638909326120, 5.324712401148210539, 11.49999999999999645 ) ) ;
#48307 = CARTESIAN_POINT ( 'NONE',  ( -9.153499762860807465, 20.15527781828815534, -1.500000000000002220 ) ) ;
#48308 = B_SPLINE_CURVE_WITH_KNOTS ( 'NONE', 3,
 ( #66947, #59322, #83138, #28361 ),
 .UNSPECIFIED., .F., .F.,
 ( 4, 4 ),
 ( 0.000000000000000000, 0.0001000000000000028644 ),
 .UNSPECIFIED. ) ;
#48309 = EDGE_CURVE ( 'NONE', #99197, #70905, #79930, .T. ) ;
#48310 = CARTESIAN_POINT ( 'NONE',  ( 15.43701773751798001, -13.56989305476470875, 11.49999999999998934 ) ) ;
#48311 = CARTESIAN_POINT ( 'NONE',  ( 7.111284305517425075, -5.876774720514421624, 21.05363841023157434 ) ) ;
#48312 = EDGE_LOOP ( 'NONE', ( #98526, #49196, #53839, #29707 ) ) ;
#48313 = DIRECTION ( 'NONE',  ( -0.8788171126619707119, 0.4771587602595986910, -0.000000000000000000 ) ) ;
#48314 = EDGE_LOOP ( 'NONE', ( #19741, #10387, #35319, #54818, #36948 ) ) ;
#48315 = ADVANCED_FACE ( 'NONE', ( #83761 ), #60945, .T. ) ;
#48316 = CARTESIAN_POINT ( 'NONE',  ( -54.64429893256247794, -23.96119346886879953, -0.6495511937832153526 ) ) ;
#48317 = CARTESIAN_POINT ( 'NONE',  ( -70.52287095715007581, -24.91570333825474748, 8.075032458260896107 ) ) ;
#48318 = ORIENTED_EDGE ( 'NONE', *, *, #43655, .F. ) ;
#48319 = ORIENTED_EDGE ( 'NONE', *, *, #71223, .T. ) ;
#48320 = ORIENTED_EDGE ( 'NONE', *, *, #99578, .F. ) ;
#48321 = FACE_OUTER_BOUND ( 'NONE', #69568, .T. ) ;
#48322 = CARTESIAN_POINT ( 'NONE',  ( -29.52287095715006515, -23.38906523657919578, -1.443836447538998424 ) ) ;
#48323 = CARTESIAN_POINT ( 'NONE',  ( 6.058092820189922456, -5.876774720514413630, 19.77091638250125882 ) ) ;
#48324 = CARTESIAN_POINT ( 'NONE',  ( 4.906390264955167169, 20.09725327650800608, -1.500000000000002220 ) ) ;
#48325 = ADVANCED_FACE ( 'NONE', ( #37596 ), #68546, .T. ) ;
#48326 = CARTESIAN_POINT ( 'NONE',  ( -19.97641003480726241, 8.421946895145676848, 11.49999999999999645 ) ) ;
#48327 = ORIENTED_EDGE ( 'NONE', *, *, #44459, .F. ) ;
#48328 = CARTESIAN_POINT ( 'NONE',  ( 22.02124265030973760, 6.143225279485574397, 16.20402280011862217 ) ) ;
#48329 = LINE ( 'NONE', #63061, #12410 ) ;
#48330 = CARTESIAN_POINT ( 'NONE',  ( 1.926536275058113867, -22.33200895297504474, -1.500000000000002220 ) ) ;
#48331 = VECTOR ( 'NONE', #49901, 1000.000000000000114 ) ;
#48332 = EDGE_CURVE ( 'NONE', #18995, #68362, #41050, .T. ) ;
#48333 = CARTESIAN_POINT ( 'NONE',  ( -47.56045540262851290, -23.73791477778911485, 11.05961554403170766 ) ) ;
#48334 = CARTESIAN_POINT ( 'NONE',  ( 29.73860345376319358, 5.356774720514427379, 1.647607965253217399 ) ) ;
#48335 = VERTEX_POINT ( 'NONE', #53332 ) ;
#48336 = CARTESIAN_POINT ( 'NONE',  ( -38.62287095715005592, -23.47593901973091235, -1.443836447539011525 ) ) ;
#48337 = CARTESIAN_POINT ( 'NONE',  ( -76.62287095715007013, -24.64965695001468404, 8.947790433994182280 ) ) ;
#48338 = ORIENTED_EDGE ( 'NONE', *, *, #68355, .F. ) ;
#48339 = EDGE_LOOP ( 'NONE', ( #43875, #67639, #73215, #63391, #55594, #19122, #885, #60026, #20840, #37077, #17117, #55657, #97363, #55136, #23600 ) ) ;
#48340 = CARTESIAN_POINT ( 'NONE',  ( -71.52287095715007581, -23.47596703998600631, 11.44779298504228748 ) ) ;
#48341 = VECTOR ( 'NONE', #1537, 1000.000000000000000 ) ;
#48342 = ORIENTED_EDGE ( 'NONE', *, *, #29700, .F. ) ;
#48343 = CARTESIAN_POINT ( 'NONE',  ( -108.5228709571500758, -23.47593901973090524, -1.443836447538996204 ) ) ;
#48344 = CARTESIAN_POINT ( 'NONE',  ( -10.85727797829764185, 18.24708236899833835, -1.500000000000002220 ) ) ;
#48345 = ORIENTED_EDGE ( 'NONE', *, *, #42162, .T. ) ;
#48346 = CARTESIAN_POINT ( 'NONE',  ( -50.48000260994784583, -24.83618233451449697, 1.606449574219540599 ) ) ;
#48347 = CARTESIAN_POINT ( 'NONE',  ( -8.041798833237560729, -20.28069125152608976, 11.49999999999998934 ) ) ;
#48348 = CARTESIAN_POINT ( 'NONE',  ( -103.6358334257766955, -23.48786465467241413, 11.44779295918254292 ) ) ;
#48349 = AXIS2_PLACEMENT_3D ( 'NONE', #37156, #83325, #21412 ) ;
#48350 = DIRECTION ( 'NONE',  ( -0.000000000000000000, 2.173523156925979552E-06, -0.9999999999976378895 ) ) ;
#48351 = CARTESIAN_POINT ( 'NONE',  ( -60.62287095715004881, -29.50249982740957577, 7.747779886224967605 ) ) ;
#48352 = CARTESIAN_POINT ( 'NONE',  ( 16.27406392464308027, 14.57352745747340172, -1.500000000000002220 ) ) ;
#48353 = CARTESIAN_POINT ( 'NONE',  ( -30.57287095715004810, -25.30498646304936727, 4.433167295270071584 ) ) ;
#48354 = ORIENTED_EDGE ( 'NONE', *, *, #42594, .T. ) ;
#48355 = CARTESIAN_POINT ( 'NONE',  ( -65.62287095715005592, -25.00158670708909270, 2.256160236439166855 ) ) ;
#48356 = DIRECTION ( 'NONE',  ( 0.000000000000000000, 0.000000000000000000, 1.000000000000000000 ) ) ;
#48357 = ORIENTED_EDGE ( 'NONE', *, *, #48818, .T. ) ;
#48358 = ORIENTED_EDGE ( 'NONE', *, *, #28124, .F. ) ;
#48359 = VECTOR ( 'NONE', #53776, 1000.000000000000000 ) ;
#48360 = VERTEX_POINT ( 'NONE', #84259 ) ;
#48361 = CARTESIAN_POINT ( 'NONE',  ( -0.02075734969026423599, 5.965225279485572685, -0.08597719988137648983 ) ) ;
#48362 = CARTESIAN_POINT ( 'NONE',  ( -113.6228709571500417, -23.48783264082479150, -1.443836473390060160 ) ) ;
#48363 = CARTESIAN_POINT ( 'NONE',  ( -1.624102159174229731, 21.17438964843747584, -1.500000000000002220 ) ) ;
#48364 = PLANE ( 'NONE',  #72544 ) ;
#48365 = CARTESIAN_POINT ( 'NONE',  ( -41.26959558397305727, -25.07899898050004950, 7.338714981574760543 ) ) ;
#48366 = CARTESIAN_POINT ( 'NONE',  ( -33.62287095715005592, -24.65952944569304250, 1.056160979905690356 ) ) ;
#48367 = FACE_OUTER_BOUND ( 'NONE', #78778, .T. ) ;
#48368 = CARTESIAN_POINT ( 'NONE',  ( 4.481524277812761525, 18.85844072219565604, 11.49999999999998934 ) ) ;
#48369 = EDGE_CURVE ( 'NONE', #53220, #56586, #42375, .T. ) ;
#48370 = EDGE_CURVE ( 'NONE', #21744, #55188, #64118, .T. ) ;
#48371 = CARTESIAN_POINT ( 'NONE',  ( -45.53831601786538386, -24.52300882791528380, 0.6510814631126234930 ) ) ;
#48372 = VERTEX_POINT ( 'NONE', #14745 ) ;
#48373 = CARTESIAN_POINT ( 'NONE',  ( 8.918240691521024388, 17.32521578647535776, 11.49999999999999645 ) ) ;
#48374 = CARTESIAN_POINT ( 'NONE',  ( -99.64934318012689118, -25.31535474791540707, 4.927356294767410105 ) ) ;
#48375 = DIRECTION ( 'NONE',  ( 1.000000000000000000, 0.000000000000000000, 0.000000000000000000 ) ) ;
#48376 = VERTEX_POINT ( 'NONE', #40099 ) ;
#48377 = CARTESIAN_POINT ( 'NONE',  ( 4.780030342074717886, -5.876774720514423400, 21.16398229115527130 ) ) ;
#48378 = CARTESIAN_POINT ( 'NONE',  ( -27.25988310792305214, -5.965225279485572685, 30.32664379231667695 ) ) ;
#48379 = CARTESIAN_POINT ( 'NONE',  ( -1.675486951385420475, 10.82748519320431591, -3.549999999999999822 ) ) ;
#48380 = FACE_OUTER_BOUND ( 'NONE', #57294, .T. ) ;
#48381 = CARTESIAN_POINT ( 'NONE',  ( -19.15281226579456231, 4.489446101945751444, -1.500000000000002220 ) ) ;
#48382 = ORIENTED_EDGE ( 'NONE', *, *, #46743, .F. ) ;
#48383 = FACE_OUTER_BOUND ( 'NONE', #51680, .T. ) ;
#48384 = CARTESIAN_POINT ( 'NONE',  ( 15.98122378838116120, 16.67787885001082770, -1.500000000000002220 ) ) ;
#48385 = EDGE_CURVE ( 'NONE', #74504, #44287, #63456, .T. ) ;
#48386 = PERSON_AND_ORGANIZATION_ROLE ( 'design_supplier' ) ;
#48387 = PLANE ( 'NONE',  #92063 ) ;
#48388 = DIRECTION ( 'NONE',  ( -3.773278334444167608E-23, 1.000000000000000000, 0.000000000000000000 ) ) ;
#48389 = CARTESIAN_POINT ( 'NONE',  ( -92.62287095715008434, -24.34917612406837861, 0.1852690917426660921 ) ) ;
#48390 = CARTESIAN_POINT ( 'NONE',  ( -97.62356141978688129, -24.66019654487199730, 8.947790411086115725 ) ) ;
#48391 = CARTESIAN_POINT ( 'NONE',  ( -78.92688763707079147, -25.20144873054373136, 6.835696071488102099 ) ) ;
#48392 = DIRECTION ( 'NONE',  ( -3.773278334453080206E-23, 0.9999999999976377785, 2.173523156925979552E-06 ) ) ;
#48393 = EDGE_CURVE ( 'NONE', #26377, #81873, #13209, .T. ) ;
#48394 = CARTESIAN_POINT ( 'NONE',  ( -129.5896973008811983, -24.34968618360934656, 0.1864209137778921610 ) ) ;
#48395 = CARTESIAN_POINT ( 'NONE',  ( -99.12380231474227799, -25.26400682238891093, 4.001575156371126596 ) ) ;
#48396 = CARTESIAN_POINT ( 'NONE',  ( -11.57717615966994273, 16.22069937712612031, 11.49999999999998934 ) ) ;
#48397 = B_SPLINE_CURVE_WITH_KNOTS ( 'NONE', 3,
 ( #95164, #9922, #26149, #25648, #87045, #17536 ),
 .UNSPECIFIED., .F., .F.,
 ( 4, 2, 4 ),
 ( 0.000000000000000000, 0.001380901958385387027, 0.002761803916770774053 ),
 .UNSPECIFIED. ) ;
#48399 = EDGE_CURVE ( 'NONE', #84073, #33754, #18081, .T. ) ;
#48398 = CARTESIAN_POINT ( 'NONE',  ( -100.4856528238762081, -25.19529134689449634, 3.295791984263175767 ) ) ;
#48400 = CARTESIAN_POINT ( 'NONE',  ( 19.67252036444665109, 2.607452956813616218, -1.500000000000002220 ) ) ;
#48401 = ORIENTED_EDGE ( 'NONE', *, *, #91063, .F. ) ;
#48402 = EDGE_CURVE ( 'NONE', #79911, #35733, #77641, .T. ) ;
#48403 = AXIS2_PLACEMENT_3D ( 'NONE', #39644, #70600, #32035 ) ;
#48404 = CARTESIAN_POINT ( 'NONE',  ( -71.52287095715006160, -23.94994826722565406, -0.6494450866342743600 ) ) ;
#48405 = EDGE_CURVE ( 'NONE', #65034, #58206, #529, .T. ) ;
#48406 = ADVANCED_FACE ( 'NONE', ( #1542 ), #23858, .F. ) ;
#48407 = CARTESIAN_POINT ( 'NONE',  ( -51.52469858490392340, -25.25107916704070732, 6.255584458614488419 ) ) ;
#48408 = CARTESIAN_POINT ( 'NONE',  ( -116.5228709571500332, -24.66019654487200086, 8.947790411086113949 ) ) ;
#48409 = CARTESIAN_POINT ( 'NONE',  ( -20.73834036848188234, 1.213307192923735345, 11.49999999999999645 ) ) ;
#48410 = CARTESIAN_POINT ( 'NONE',  ( -102.2228709571500502, -23.47596703998600276, 11.44779298504227683 ) ) ;
#48411 = CARTESIAN_POINT ( 'NONE',  ( -40.55620429048340014, -24.99132157543166244, 2.256160258750668390 ) ) ;
#48412 = CARTESIAN_POINT ( 'NONE',  ( 22.73759373355791169, -1.750760473330008171, 11.49999999999999645 ) ) ;
#48413 = ORIENTED_EDGE ( 'NONE', *, *, #9893, .F. ) ;
#48414 = CARTESIAN_POINT ( 'NONE',  ( -69.49773674714293747, -24.51314013834315375, 0.6176544820404143987 ) ) ;
#48415 = PLANE ( 'NONE',  #64659 ) ;
#48416 = ORIENTED_EDGE ( 'NONE', *, *, #44083, .T. ) ;
#48417 = AXIS2_PLACEMENT_3D ( 'NONE', #94075, #92569, #7333 ) ;
#48418 = CARTESIAN_POINT ( 'NONE',  ( -6.636546740042271963, -19.09123619949631134, -1.500000000000002220 ) ) ;
#48419 = EDGE_CURVE ( 'NONE', #23708, #26794, #56923, .T. ) ;
#48420 = EDGE_CURVE ( 'NONE', #41980, #63083, #52059, .T. ) ;
#48421 = CARTESIAN_POINT ( 'NONE',  ( -90.22287095715005023, -23.47596703998600631, 11.44779298504227860 ) ) ;
#48422 = CARTESIAN_POINT ( 'NONE',  ( -110.5228709571500048, -24.52323809116983355, 9.355190652339414825 ) ) ;
#48423 = EDGE_LOOP ( 'NONE', ( #98124, #25763, #3627, #8997 ) ) ;
#48424 = DIRECTION ( 'NONE',  ( -3.773278334453079618E-23, 0.9999999999976377785, 2.173523156925978705E-06 ) ) ;
#48425 = CARTESIAN_POINT ( 'NONE',  ( -10.11875734969026297, 3.316774720514426456, 30.51402280011862089 ) ) ;
#48426 = CARTESIAN_POINT ( 'NONE',  ( 16.79232260237064978, 10.84791536263152523, -1.500000000000002220 ) ) ;
#48427 = CARTESIAN_POINT ( 'NONE',  ( -32.62287095715004881, -24.65952944569304250, 1.056160979905691688 ) ) ;
#48428 = CARTESIAN_POINT ( 'NONE',  ( -7.180602670292889123, -19.69607742855361465, 11.49999999999999645 ) ) ;
#48429 = DIRECTION ( 'NONE',  ( -0.9975640502598243087, 0.06975647374412548285, 0.000000000000000000 ) ) ;
#48430 = CARTESIAN_POINT ( 'NONE',  ( -52.52287095715006870, -24.64965694238574656, 8.947790433994203596 ) ) ;
#48431 = CARTESIAN_POINT ( 'NONE',  ( -10.28628152547328511, -19.52461415289770130, -1.500000000000002220 ) ) ;
#48432 = EDGE_CURVE ( 'NONE', #24870, #25405, #99337, .T. ) ;
#48433 = CARTESIAN_POINT ( 'NONE',  ( 6.184520403203631389, 5.356774720514425603, -25.32021290018218451 ) ) ;
#48434 = VECTOR ( 'NONE', #40401, 1000.000000000000114 ) ;
#48435 = VERTEX_POINT ( 'NONE', #16256 ) ;
#48436 = CARTESIAN_POINT ( 'NONE',  ( -127.5895376238166961, -23.48786465467242124, 11.44779295918253403 ) ) ;
#48437 = CARTESIAN_POINT ( 'NONE',  ( -49.51045894826389571, -25.27344895790480450, 3.920634769891420568 ) ) ;
#48438 = EDGE_CURVE ( 'NONE', #6989, #16640, #70150, .T. ) ;
#48439 = DIRECTION ( 'NONE',  ( 0.000000000000000000, 0.000000000000000000, 1.000000000000000000 ) ) ;
#48440 = ORIENTED_EDGE ( 'NONE', *, *, #33554, .T. ) ;
#48441 = CARTESIAN_POINT ( 'NONE',  ( 3.797776442307698286, -6.376774720514401196, 18.16025641025640525 ) ) ;
#48442 = ORIENTED_EDGE ( 'NONE', *, *, #77473, .F. ) ;
#48443 = ORIENTED_EDGE ( 'NONE', *, *, #16020, .T. ) ;
#48444 = DIRECTION ( 'NONE',  ( -1.000000000000000000, -8.503546450866701308E-16, 0.000000000000000000 ) ) ;
#48445 = CARTESIAN_POINT ( 'NONE',  ( -101.2911250451791858, -25.10935867328099391, 3.130826437452274735 ) ) ;
#48446 = CARTESIAN_POINT ( 'NONE',  ( -94.62287095715005592, -24.64965695001469115, 8.947790433994180503 ) ) ;
#48447 = CARTESIAN_POINT ( 'NONE',  ( 19.85418835109896563, -5.301297255791479479, -1.500000000000002220 ) ) ;
#48448 = ADVANCED_FACE ( 'NONE', ( #43105 ), #66466, .F. ) ;
#48449 = VERTEX_POINT ( 'NONE', #12638 ) ;
#48450 = CARTESIAN_POINT ( 'NONE',  ( -99.30778403274287314, -25.26531023543898158, 5.994093549950689770 ) ) ;
#48451 = CARTESIAN_POINT ( 'NONE',  ( 1.542438661763949392, 2.939152317953647106E-16, -2.399999999999999911 ) ) ;
#48452 = CARTESIAN_POINT ( 'NONE',  ( 27.86270917940689174, 5.965225279485572685, 29.02104833056109001 ) ) ;
#48453 = CARTESIAN_POINT ( 'NONE',  ( 16.98343680692684643, -14.46476453587665389, -1.500000000000002220 ) ) ;
#48454 = EDGE_CURVE ( 'NONE', #90958, #40108, #70202, .T. ) ;
#48455 = B_SPLINE_CURVE_WITH_KNOTS ( 'NONE', 3,
 ( #6312, #20041, #36273, #60620 ),
 .UNSPECIFIED., .F., .F.,
 ( 4, 4 ),
 ( 0.000000000000000000, 1.000000000000000000 ),
 .UNSPECIFIED. ) ;
#48456 = CARTESIAN_POINT ( 'NONE',  ( -0.02086824871851766100, -22.77984412121519497, 2.712351064733621531 ) ) ;
#48457 = CARTESIAN_POINT ( 'NONE',  ( -1.371775545366004545, -5.876774720514414518, 20.39230070883894186 ) ) ;
#48458 = ORIENTED_EDGE ( 'NONE', *, *, #84409, .F. ) ;
#48459 = ADVANCED_FACE ( 'NONE', ( #42614 ), #58335, .F. ) ;
#48460 = CARTESIAN_POINT ( 'NONE',  ( -29.49875734969026198, 5.965225279485572685, 2.362022800118626531 ) ) ;
#48461 = CARTESIAN_POINT ( 'NONE',  ( 5.265981236333619456E-16, -1.473225279485573802, -4.300000000000000711 ) ) ;
#48462 = CARTESIAN_POINT ( 'NONE',  ( -2.238888094254589234, -20.74146561784671761, 11.49999999999998934 ) ) ;
#48463 = ORIENTED_EDGE ( 'NONE', *, *, #40504, .T. ) ;
#48465 = ORIENTED_EDGE ( 'NONE', *, *, #21599, .F. ) ;
#48464 = CARTESIAN_POINT ( 'NONE',  ( -79.52287095715004739, -23.73934037231757088, 11.05740245334329508 ) ) ;
#48466 = ORIENTED_EDGE ( 'NONE', *, *, #49680, .T. ) ;
#48468 = EDGE_CURVE ( 'NONE', #19353, #71104, #56845, .T. ) ;
#48467 = CARTESIAN_POINT ( 'NONE',  ( -68.94461706535129508, -25.25935091778287855, 6.371760082740177467 ) ) ;
#48469 = CARTESIAN_POINT ( 'NONE',  ( 2.841100885065937387, 20.89556961663114265, -1.500000000000002220 ) ) ;
#48470 = ORIENTED_EDGE ( 'NONE', *, *, #18311, .T. ) ;
#48471 = CARTESIAN_POINT ( 'NONE',  ( 9.150000000000000355, -5.876774720514426953, -15.70000000000000284 ) ) ;
#48472 = AXIS2_PLACEMENT_3D ( 'NONE', #11976, #82481, #43443 ) ;
#48473 = LINE ( 'NONE', #79401, #36865 ) ;
#48474 = CARTESIAN_POINT ( 'NONE',  ( -105.6228709571500275, -25.00182538069145721, 7.747789668545099317 ) ) ;
#48475 = AXIS2_PLACEMENT_3D ( 'NONE', #64168, #9845, #64673 ) ;
#48476 = CARTESIAN_POINT ( 'NONE',  ( -86.58557003059961232, -24.51419770103155926, 9.386484678747176957 ) ) ;
#48477 = B_SPLINE_CURVE_WITH_KNOTS ( 'NONE', 3,
 ( #31724, #25098, #64708, #80398, #41341, #8886 ),
 .UNSPECIFIED., .F., .F.,
 ( 4, 2, 4 ),
 ( 6.384118678610730862E-06, 0.001386860460828374334, 0.002767336802978137989 ),
 .UNSPECIFIED. ) ;
#48478 = CARTESIAN_POINT ( 'NONE',  ( -59.52207695799008746, -23.48783264082476308, -1.443836473390097908 ) ) ;
#48479 = CARTESIAN_POINT ( 'NONE',  ( -108.9573283046188408, -25.29252521095624928, 4.249509941946580938 ) ) ;
#48480 = CARTESIAN_POINT ( 'NONE',  ( 0.000000000000000000, -2.056774720514426669, 4.299999999999999822 ) ) ;
#48482 = ORIENTED_EDGE ( 'NONE', *, *, #10309, .F. ) ;
#48481 = CARTESIAN_POINT ( 'NONE',  ( -14.74362065938029076, 16.57599527146691898, 11.49999999999999645 ) ) ;
#48483 = CARTESIAN_POINT ( 'NONE',  ( -99.07695620119221758, -25.30872027043050210, 5.427344019169676237 ) ) ;
#48484 = PLANE ( 'NONE',  #73209 ) ;
#48485 = ORIENTED_EDGE ( 'NONE', *, *, #77638, .T. ) ;
#48486 = CARTESIAN_POINT ( 'NONE',  ( 20.48348528492645571, -9.684159049092739835, 11.49999999999998934 ) ) ;
#48487 = VECTOR ( 'NONE', #63187, 1000.000000000000114 ) ;
#48489 = VERTEX_POINT ( 'NONE', #11144 ) ;
#48488 = CARTESIAN_POINT ( 'NONE',  ( -6.377963355984652694, -6.376774720514411854, 19.53740760792478426 ) ) ;
#48490 = EDGE_LOOP ( 'NONE', ( #95627, #38833, #99442, #58105 ) ) ;
#48491 = AXIS2_PLACEMENT_3D ( 'NONE', #11579, #16819, #3985 ) ;
#48492 = DIRECTION ( 'NONE',  ( 0.000000000000000000, -1.000000000000000000, 0.000000000000000000 ) ) ;
#48493 = CARTESIAN_POINT ( 'NONE',  ( 20.11291949428234105, -1.170665973999911902, 11.49999999999998934 ) ) ;
#48494 = DIRECTION ( 'NONE',  ( 0.000000000000000000, 0.000000000000000000, -1.000000000000000000 ) ) ;
#48495 = ORIENTED_EDGE ( 'NONE', *, *, #61337, .F. ) ;
#48496 = VECTOR ( 'NONE', #88240, 1000.000000000000000 ) ;
#48497 = CARTESIAN_POINT ( 'NONE',  ( -130.5728709571500872, -25.40555871708352953, 4.425364043583297935 ) ) ;
#48498 = CARTESIAN_POINT ( 'NONE',  ( 3.152853332073482839, 22.16862046936333286, -1.500000000000002220 ) ) ;
#48499 = ORIENTED_EDGE ( 'NONE', *, *, #97413, .F. ) ;
#48500 = ORIENTED_EDGE ( 'NONE', *, *, #69956, .F. ) ;
#48501 = CARTESIAN_POINT ( 'NONE',  ( -89.40841769935769889, -25.13785473458444031, 7.104038777038262253 ) ) ;
#48502 = CARTESIAN_POINT ( 'NONE',  ( -48.52287095715006160, -24.66019654487200086, 8.947790411086119278 ) ) ;
#48503 = CARTESIAN_POINT ( 'NONE',  ( -96.52287095715006160, -23.47596703998600631, 11.44779298504228215 ) ) ;
#48504 = LINE ( 'NONE', #80941, #57897 ) ;
#48505 = CARTESIAN_POINT ( 'NONE',  ( -30.63241211973601352, -23.78062553189671746, -0.9709657327914300584 ) ) ;
#48506 = CARTESIAN_POINT ( 'NONE',  ( -13.92019785312828972, -13.74635529968554515, 11.49999999999998934 ) ) ;
#48507 = DIRECTION ( 'NONE',  ( 0.000000000000000000, -1.000000000000000000, 0.000000000000000000 ) ) ;
#48508 = VERTEX_POINT ( 'NONE', #4548 ) ;
#48509 = CARTESIAN_POINT ( 'NONE',  ( 20.90071823198991297, 5.034746273075951351, 11.49999999999998934 ) ) ;
#48510 = CARTESIAN_POINT ( 'NONE',  ( -36.52287095715006870, -23.47593901973090169, -1.443836447538997314 ) ) ;
#48512 = CARTESIAN_POINT ( 'NONE',  ( 30.09341516180546350, 1.682774720514426114, -11.39311774897855756 ) ) ;
#48511 = B_SPLINE_CURVE_WITH_KNOTS ( 'NONE', 3,
 ( #61445, #38592, #31982, #78132, #70544, #22344 ),
 .UNSPECIFIED., .F., .F.,
 ( 4, 2, 4 ),
 ( 6.384118678611516061E-06, 0.001386860460828373250, 0.002767336802978134953 ),
 .UNSPECIFIED. ) ;
#48513 = CARTESIAN_POINT ( 'NONE',  ( 27.53860345374808105, 5.356774720496559894, 19.84760796525321780 ) ) ;
#48514 = CARTESIAN_POINT ( 'NONE',  ( -80.62287095715005592, -24.99156045073393173, 7.747789690856161648 ) ) ;
#48515 = CARTESIAN_POINT ( 'NONE',  ( -22.92702450682246251, 0.3551139841105944162, -1.500000000000002220 ) ) ;
#48516 = CIRCLE ( 'NONE', #51769, 2.499999999999995115 ) ;
#48517 = EDGE_CURVE ( 'NONE', #33604, #94189, #72555, .T. ) ;
#48518 = APPROVAL_DATE_TIME ( #71852, #82954 ) ;
#48519 = LINE ( 'NONE', #29157, #54785 ) ;
#48520 = CARTESIAN_POINT ( 'NONE',  ( -2.772696838893043747, -5.876774720514414518, 19.95463486386180207 ) ) ;
#48521 = CARTESIAN_POINT ( 'NONE',  ( 1.236116150138429903, -20.07036509671028668, 11.49999999999999645 ) ) ;
#48522 = LINE ( 'NONE', #3847, #83530 ) ;
#48523 = LINE ( 'NONE', #93670, #59818 ) ;
#48524 = EDGE_CURVE ( 'NONE', #26860, #15801, #65388, .T. ) ;
#48525 = EDGE_CURVE ( 'NONE', #62936, #39701, #1198, .T. ) ;
#48526 = CARTESIAN_POINT ( 'NONE',  ( -121.6228709571500417, -24.50321055353806798, 9.387540953477529371 ) ) ;
#48527 = DIRECTION ( 'NONE',  ( -3.773278334453079618E-23, 0.9999999999976377785, 2.173523156925979975E-06 ) ) ;
#48528 = CARTESIAN_POINT ( 'NONE',  ( -49.62287095715005592, -24.66019654487199020, 8.947790411086135265 ) ) ;
#48529 = CARTESIAN_POINT ( 'NONE',  ( -19.53060160647804722, 3.385818350044136338, -1.500000000000002220 ) ) ;
#48530 = ADVANCED_FACE ( 'NONE', ( #27376 ), #58826, .F. ) ;
#48531 = CARTESIAN_POINT ( 'NONE',  ( 0.2638585030419089428, -21.76204025362994798, -1.500000000000002220 ) ) ;
#48532 = CARTESIAN_POINT ( 'NONE',  ( 2.100208336950355914, 0.000000000000000000, 0.000000000000000000 ) ) ;
#48533 = CARTESIAN_POINT ( 'NONE',  ( 5.117700956428186565, 18.95590836763280862, -1.500000000000002220 ) ) ;
#48534 = EDGE_CURVE ( 'NONE', #36610, #17395, #49728, .T. ) ;
#48535 = CARTESIAN_POINT ( 'NONE',  ( 8.160000000000000142, -7.572993419422045847, 8.500388862211309515 ) ) ;
#48536 = EDGE_CURVE ( 'NONE', #2820, #41820, #63932, .T. ) ;
#48537 = CARTESIAN_POINT ( 'NONE',  ( 29.73860345376319358, 5.356774720496559894, -0.3523920347467610070 ) ) ;
#48538 = DATE_AND_TIME ( #88094, #18185 ) ;
#48539 = ADVANCED_FACE ( 'NONE', ( #26374 ), #19249, .F. ) ;
#48540 = CARTESIAN_POINT ( 'NONE',  ( -103.5228709571500616, -24.50216790748205042, 0.6166512839542598323 ) ) ;
#48541 = CARTESIAN_POINT ( 'NONE',  ( -54.62287095715005592, -29.50247984919015209, -1.443849546365058689 ) ) ;
#48542 = CARTESIAN_POINT ( 'NONE',  ( 16.43461662053371697, -12.34185696772103391, 11.49999999999999645 ) ) ;
#48543 = CARTESIAN_POINT ( 'NONE',  ( 4.415069475862049231, -5.876774720514423400, 21.13806644168711557 ) ) ;
#48544 = CARTESIAN_POINT ( 'NONE',  ( 3.675000000000004707, 0.000000000000000000, 0.000000000000000000 ) ) ;
#48545 = CARTESIAN_POINT ( 'NONE',  ( -11.86362535333686807, -19.25999739251378173, 11.49999999999999645 ) ) ;
#48546 = VERTEX_POINT ( 'NONE', #12134 ) ;
#48547 = CARTESIAN_POINT ( 'NONE',  ( -69.86129607977629519, -25.25639579666412615, 7.001236270658951710 ) ) ;
#48548 = CARTESIAN_POINT ( 'NONE',  ( -98.62287095715005592, -23.47593901973091235, -1.443836447539001089 ) ) ;
#48549 = CARTESIAN_POINT ( 'NONE',  ( -97.55239856924187336, -24.15543982623907837, -0.2315651400026600415 ) ) ;
#48550 = CARTESIAN_POINT ( 'NONE',  ( -26.43215695177226010, -24.84863243741908434, 3.116149861069652083 ) ) ;
#48551 = CIRCLE ( 'NONE', #55053, 0.1000000000000000472 ) ;
#48552 = EDGE_CURVE ( 'NONE', #54184, #32574, #35492, .T. ) ;
#48553 = CARTESIAN_POINT ( 'NONE',  ( -110.5228709571500474, -24.63287334234179582, 0.9662140553045319713 ) ) ;
#48554 = DIRECTION ( 'NONE',  ( -1.000000000000000000, 0.000000000000000000, -0.000000000000000000 ) ) ;
#48555 = VECTOR ( 'NONE', #14860, 1000.000000000000000 ) ;
#48556 = VERTEX_POINT ( 'NONE', #10650 ) ;
#48557 = EDGE_CURVE ( 'NONE', #55957, #39695, #23990, .T. ) ;
#48558 = CARTESIAN_POINT ( 'NONE',  ( -79.46066275308743343, -25.31596331910725084, 5.472043507825191888 ) ) ;
#48559 = CARTESIAN_POINT ( 'NONE',  ( -18.62658236799572720, 13.20813282334384553, 11.49999999999998934 ) ) ;
#48560 = CARTESIAN_POINT ( 'NONE',  ( -110.6052975838258590, -25.18890164017962974, 3.322127376059897053 ) ) ;
#48561 = VECTOR ( 'NONE', #99936, 1000.000000000000000 ) ;
#48562 = CARTESIAN_POINT ( 'NONE',  ( -106.6228709571500559, -23.73934037231757799, 11.05740245334328442 ) ) ;
#48563 = LINE ( 'NONE', #71389, #69537 ) ;
#48564 = CARTESIAN_POINT ( 'NONE',  ( 22.48772827135616126, 0.8316936486096353498, 11.49999999999999645 ) ) ;
#48565 = ORIENTED_EDGE ( 'NONE', *, *, #37071, .T. ) ;
#48566 = AXIS2_PLACEMENT_3D ( 'NONE', #84219, #87738, #16213 ) ;
#48567 = DIRECTION ( 'NONE',  ( 0.000000000000000000, 0.000000000000000000, 1.000000000000000000 ) ) ;
#48568 = CARTESIAN_POINT ( 'NONE',  ( -20.77788740438921522, -7.151594987469691134, 11.49999999999998934 ) ) ;
#48569 = CARTESIAN_POINT ( 'NONE',  ( -114.5228709571500616, -23.95044443724992789, 10.65354141964649592 ) ) ;
#48571 = CARTESIAN_POINT ( 'NONE',  ( 22.81105451610979173, 8.475225279485572472, -18.46691820600746681 ) ) ;
#48570 = VECTOR ( 'NONE', #45973, 1000.000000000000114 ) ;
#48572 = CARTESIAN_POINT ( 'NONE',  ( -69.27702271707670434, -25.12257852196836438, 7.104949132215303997 ) ) ;
#48573 = ORIENTED_EDGE ( 'NONE', *, *, #16028, .T. ) ;
#48574 = PLANE ( 'NONE',  #31417 ) ;
#48575 = CARTESIAN_POINT ( 'NONE',  ( -71.52287095715007581, -29.50250243563736774, 8.947779886222143375 ) ) ;
#48576 = ORIENTED_EDGE ( 'NONE', *, *, #37112, .F. ) ;
#48577 = CARTESIAN_POINT ( 'NONE',  ( -15.16157141410761966, -13.82251119679066953, 11.49999999999998934 ) ) ;
#48578 = ORIENTED_EDGE ( 'NONE', *, *, #42349, .T. ) ;
#48579 = EDGE_LOOP ( 'NONE', ( #7659, #18767, #54598, #80505 ) ) ;
#48580 = VERTEX_POINT ( 'NONE', #64968 ) ;
#48581 = ORIENTED_EDGE ( 'NONE', *, *, #49791, .T. ) ;
#48582 = CARTESIAN_POINT ( 'NONE',  ( 2.922108196329484375, -6.376774720514417183, 20.36383711510645256 ) ) ;
#48583 = CARTESIAN_POINT ( 'NONE',  ( 22.95697726795019378, -2.620641032420567118, 11.49999999999998934 ) ) ;
#48584 = FACE_OUTER_BOUND ( 'NONE', #11890, .T. ) ;
#48585 = CARTESIAN_POINT ( 'NONE',  ( 0.8761431260907562857, 20.31601184897261092, -1.500000000000002220 ) ) ;
#48586 = ORIENTED_EDGE ( 'NONE', *, *, #97536, .F. ) ;
#48587 = DIRECTION ( 'NONE',  ( 1.000000000000000000, 0.000000000000000000, 0.000000000000000000 ) ) ;
#48588 = CARTESIAN_POINT ( 'NONE',  ( -51.52287095715006870, -23.47596703998600631, 11.44779298504229104 ) ) ;
#48589 = EDGE_CURVE ( 'NONE', #40340, #88666, #1003, .T. ) ;
#48590 = CARTESIAN_POINT ( 'NONE',  ( -114.6228709571500843, -24.35013146730204525, 9.818937971375108376 ) ) ;
#48591 = CARTESIAN_POINT ( 'NONE',  ( 3.903461913076534451, -5.876774720514405637, 18.52532880998198905 ) ) ;
#48593 = ORIENTED_EDGE ( 'NONE', *, *, #21109, .F. ) ;
#48592 = CARTESIAN_POINT ( 'NONE',  ( -19.33005188562793819, 9.364626179424670127, 11.49999999999999645 ) ) ;
#48594 = CARTESIAN_POINT ( 'NONE',  ( -75.53786830476269643, -24.83618233451450763, 1.606449574219540599 ) ) ;
#48595 = CARTESIAN_POINT ( 'NONE',  ( 27.53860345374808105, -1.682774720514426114, -1.272392034746785860 ) ) ;
#48596 = ORIENTED_EDGE ( 'NONE', *, *, #79038, .T. ) ;
#48597 = CARTESIAN_POINT ( 'NONE',  ( -15.27568272636907665, 14.01247568063241999, -1.500000000000002220 ) ) ;
#48598 = EDGE_CURVE ( 'NONE', #87115, #51471, #73060, .T. ) ;
#48599 = ORIENTED_EDGE ( 'NONE', *, *, #579, .T. ) ;
#48601 = ORIENTED_EDGE ( 'NONE', *, *, #73938, .F. ) ;
#48600 = CARTESIAN_POINT ( 'NONE',  ( -91.62287095715004170, -24.64898659630368627, 1.056161002820827921 ) ) ;
#48602 = FACE_OUTER_BOUND ( 'NONE', #44363, .T. ) ;
#48603 = CARTESIAN_POINT ( 'NONE',  ( -28.98875734969026396, 5.965225279485572685, 10.11402280011862587 ) ) ;
#48604 = ORIENTED_EDGE ( 'NONE', *, *, #78181, .T. ) ;
#48605 = ORIENTED_EDGE ( 'NONE', *, *, #16772, .T. ) ;
#48606 = CARTESIAN_POINT ( 'NONE',  ( 14.61581670307174008, 2.682774720514426559, -27.35847990810646024 ) ) ;
#48607 = DIRECTION ( 'NONE',  ( -0.000000000000000000, 0.000000000000000000, -1.000000000000000000 ) ) ;
#48608 = CARTESIAN_POINT ( 'NONE',  ( -29.68527933152038045, -25.15099025512602537, 3.470668543855588428 ) ) ;
#48610 = EDGE_LOOP ( 'NONE', ( #30117, #24228, #21305, #48198 ) ) ;
#48609 = CARTESIAN_POINT ( 'NONE',  ( 21.99661117994144988, 0.4758108284031232760, 11.49999999999999645 ) ) ;
#48611 = DIRECTION ( 'NONE',  ( 1.000000000000000000, 0.000000000000000000, 0.000000000000000000 ) ) ;
#48612 = CARTESIAN_POINT ( 'NONE',  ( 14.59886444729927923, 17.24780449347180067, -1.500000000000002220 ) ) ;
#48613 = CARTESIAN_POINT ( 'NONE',  ( 12.56776941831905070, -16.83212535568997126, 11.49999999999998934 ) ) ;
#48615 = ORIENTED_EDGE ( 'NONE', *, *, #92283, .T. ) ;
#48614 = CARTESIAN_POINT ( 'NONE',  ( -62.52287095715006160, -24.50216790748204687, 0.6166512839542488411 ) ) ;
#48616 = ORIENTED_EDGE ( 'NONE', *, *, #45545, .T. ) ;
#48617 = DIRECTION ( 'NONE',  ( -1.000000000000000000, -0.000000000000000000, -0.000000000000000000 ) ) ;
#48618 = VECTOR ( 'NONE', #58724, 1000.000000000000000 ) ;
#48619 = DIRECTION ( 'NONE',  ( 0.000000000000000000, 0.9999999999976377785, 2.173523156925979128E-06 ) ) ;
#48620 = ORIENTED_EDGE ( 'NONE', *, *, #96308, .T. ) ;
#48621 = CARTESIAN_POINT ( 'NONE',  ( 10.59196434753715010, 18.29633683537252509, -1.500000000000002220 ) ) ;
#48622 = CARTESIAN_POINT ( 'NONE',  ( 6.499999999999992895, 4.999999999999998224, 2.100000000000000089 ) ) ;
#48623 = CARTESIAN_POINT ( 'NONE',  ( -50.58702570880215177, -25.03148741087247942, 7.558809112751002424 ) ) ;
#48624 = VECTOR ( 'NONE', #99572, 1000.000000000000114 ) ;
#48625 = CARTESIAN_POINT ( 'NONE',  ( -71.20541289166536103, -25.31502801509702749, 4.885889949323629189 ) ) ;
#48626 = DIRECTION ( 'NONE',  ( -3.773278334453079030E-23, 0.9999999999976377785, 2.173523156925979128E-06 ) ) ;
#48627 = CARTESIAN_POINT ( 'NONE',  ( 14.71430157977438924, -16.63553917435140406, -1.500000000000002220 ) ) ;
#48628 = CARTESIAN_POINT ( 'NONE',  ( -114.6254336291504501, -24.34968618360934656, 0.1864209137778972403 ) ) ;
#48629 = ORIENTED_EDGE ( 'NONE', *, *, #88086, .F. ) ;
#48630 = CARTESIAN_POINT ( 'NONE',  ( -117.5228709571500758, -29.50247984919015209, -1.443849546365046699 ) ) ;
#48631 = DIRECTION ( 'NONE',  ( -3.773278334453079030E-23, 0.9999999999976377785, 2.173523156925979128E-06 ) ) ;
#48632 = CARTESIAN_POINT ( 'NONE',  ( -10.03281922573575002, -16.61734169602722488, 11.49999999999999645 ) ) ;
#48633 = VECTOR ( 'NONE', #94132, 1000.000000000000114 ) ;
#48634 = CARTESIAN_POINT ( 'NONE',  ( -36.53263999733187006, -24.51419770103156637, 9.386484678747175181 ) ) ;
#48635 = CARTESIAN_POINT ( 'NONE',  ( -82.62287095715005592, -23.47593901973091235, -1.443836447539004642 ) ) ;
#48636 = VECTOR ( 'NONE', #96478, 1000.000000000000114 ) ;
#48637 = CARTESIAN_POINT ( 'NONE',  ( 13.74000504945409418, 13.82049530813991467, -1.500000000000002220 ) ) ;
#48638 = VECTOR ( 'NONE', #23816, 1000.000000000000000 ) ;
#48639 = CARTESIAN_POINT ( 'NONE',  ( -21.42254595866439004, -0.3319015934494286557, 11.49999999999998934 ) ) ;
#48640 = CARTESIAN_POINT ( 'NONE',  ( -10.58858228176428540, 0.3587747205144061202, -27.03148018517017803 ) ) ;
#48641 = CARTESIAN_POINT ( 'NONE',  ( -60.64002619184125109, -24.40133493613623372, 9.663955038888268234 ) ) ;
#48642 = CARTESIAN_POINT ( 'NONE',  ( -51.50748557923905224, -23.96119346886880663, -0.6495511937832119109 ) ) ;
#48643 = DIRECTION ( 'NONE',  ( 0.000000000000000000, -0.9999999999976377785, -2.173523156925979128E-06 ) ) ;
#48644 = CARTESIAN_POINT ( 'NONE',  ( -22.52399778787742335, 3.408274809117095572, -1.500000000000002220 ) ) ;
#48645 = AXIS2_PLACEMENT_3D ( 'NONE', #24009, #68201, #76779 ) ;
#48646 = EDGE_CURVE ( 'NONE', #25101, #1158, #27601, .T. ) ;
#48647 = SHAPE_REPRESENTATION_RELATIONSHIP ( 'NONE' , 'NONE' ,  #32845, #59836 ) ;
#48648 = CARTESIAN_POINT ( 'NONE',  ( -106.6248927510747819, -24.51419770103158768, 9.386484678747164523 ) ) ;
#48649 = DIRECTION ( 'NONE',  ( -1.000000000000000000, -3.773278334444167608E-23, -8.201307833595939069E-29 ) ) ;
#48650 = CARTESIAN_POINT ( 'NONE',  ( 10.41257876278241845, -16.90412932818451353, 11.49999999999999645 ) ) ;
#48651 = CARTESIAN_POINT ( 'NONE',  ( 6.058092820189922456, -6.376774720514413630, 19.77091638250125882 ) ) ;
#48652 = EDGE_CURVE ( 'NONE', #89282, #47313, #66949, .T. ) ;
#48653 = DIRECTION ( 'NONE',  ( 1.000000000000000000, 3.491481338843133355E-15, 2.352173255807796056E-16 ) ) ;
#48654 = CARTESIAN_POINT ( 'NONE',  ( -92.52287095715006160, -23.48786465467241769, 11.44779295918254292 ) ) ;
#48655 = VERTEX_POINT ( 'NONE', #21735 ) ;
#48656 = DIRECTION ( 'NONE',  ( 3.773278334444167608E-23, -1.000000000000000000, 0.000000000000000000 ) ) ;
#48657 = CARTESIAN_POINT ( 'NONE',  ( -1.164890887384984586, 4.028272616778473036, -3.549999999999999378 ) ) ;
#48658 = EDGE_CURVE ( 'NONE', #1547, #5151, #37977, .T. ) ;
#48659 = CARTESIAN_POINT ( 'NONE',  ( -51.32120688873476411, -25.10935831503348581, 3.174475921786763077 ) ) ;
#48660 = CARTESIAN_POINT ( 'NONE',  ( 4.495418090846292181, 21.21921847905042569, 11.49999999999998934 ) ) ;
#48661 = PLANE ( 'NONE',  #86844 ) ;
#48662 = CARTESIAN_POINT ( 'NONE',  ( -17.65537929698502495, 8.214918384300796461, -1.500000000000002220 ) ) ;
#48663 = EDGE_CURVE ( 'NONE', #64945, #6225, #18368, .T. ) ;
#48664 = CARTESIAN_POINT ( 'NONE',  ( 28.20688450243577705, 4.772774720514425972, -7.073367244511738150 ) ) ;
#48665 = ORIENTED_EDGE ( 'NONE', *, *, #59641, .F. ) ;
#48666 = EDGE_CURVE ( 'NONE', #88122, #59933, #24881, .T. ) ;
#48667 = CARTESIAN_POINT ( 'NONE',  ( 18.38310620586021571, 8.829655622120887060, 11.49999999999999645 ) ) ;
#48668 = CARTESIAN_POINT ( 'NONE',  ( -16.22218391600152643, 6.376774720514426953, -54.85883559227303863 ) ) ;
#48669 = EDGE_CURVE ( 'NONE', #22711, #99954, #83182, .T. ) ;
#48670 = CARTESIAN_POINT ( 'NONE',  ( 5.949073730962466833, 6.475225279485573360, -27.94053387008862188 ) ) ;
#48671 = ORIENTED_EDGE ( 'NONE', *, *, #46709, .T. ) ;
#48672 = DIRECTION ( 'NONE',  ( 0.000000000000000000, 0.000000000000000000, 1.000000000000000000 ) ) ;
#48673 = CARTESIAN_POINT ( 'NONE',  ( -29.62287095715003815, -23.88347863494311341, -0.6494985534383576065 ) ) ;
#48674 = CARTESIAN_POINT ( 'NONE',  ( -48.92287095715006018, -23.47596703998600276, 11.44779298504227683 ) ) ;
#48675 = DIRECTION ( 'NONE',  ( -0.000000000000000000, -0.000000000000000000, -1.000000000000000000 ) ) ;
#48676 = CARTESIAN_POINT ( 'NONE',  ( -38.62287095715005592, -23.47596703998600276, 11.44779298504227505 ) ) ;
#48677 = CARTESIAN_POINT ( 'NONE',  ( -106.5228709571500758, -29.50250243563736774, 8.947779886222136270 ) ) ;
#48678 = ORIENTED_EDGE ( 'NONE', *, *, #3128, .F. ) ;
#48679 = CARTESIAN_POINT ( 'NONE',  ( -66.49650470888528275, -24.51419770103157347, 9.386484678747176957 ) ) ;
#48680 = CARTESIAN_POINT ( 'NONE',  ( 20.74614131242519477, 9.816050768296040729, 11.49999999999999645 ) ) ;
#48681 = CARTESIAN_POINT ( 'NONE',  ( 5.860688371469950475, 21.97560254587667217, 11.49999999999998934 ) ) ;
#48682 = VERTEX_POINT ( 'NONE', #14632 ) ;
#48683 = CARTESIAN_POINT ( 'NONE',  ( -110.5501817371814468, -24.73531770709095312, 8.716586749053508498 ) ) ;
#48684 = CARTESIAN_POINT ( 'NONE',  ( -3.749999999999999112, 25.69999999999999574, 0.000000000000000000 ) ) ;
#48685 = CARTESIAN_POINT ( 'NONE',  ( 10.28391390014267692, 1.335655600570678558, 18.31352460785937453 ) ) ;
#48686 = CARTESIAN_POINT ( 'NONE',  ( -110.5570708675502516, -23.85016227208580020, -0.8807180028928306426 ) ) ;
#48687 = VECTOR ( 'NONE', #89871, 1000.000000000000000 ) ;
#48688 = CARTESIAN_POINT ( 'NONE',  ( -8.129759772327192380, 20.32010563749377141, -1.500000000000002220 ) ) ;
#48689 = CARTESIAN_POINT ( 'NONE',  ( -69.60832130884770663, -23.48786465467240703, 11.44779295918255002 ) ) ;
#48690 = CARTESIAN_POINT ( 'NONE',  ( -28.84663072490566194, -5.965225279485572685, 28.73989617533406715 ) ) ;
#48691 = DIRECTION ( 'NONE',  ( 0.000000000000000000, 0.000000000000000000, 1.000000000000000000 ) ) ;
#48692 = DIRECTION ( 'NONE',  ( -0.7071067811865515695, 0.7071067811865435759, 0.000000000000000000 ) ) ;
#48693 = EDGE_LOOP ( 'NONE', ( #62171, #90212, #80436, #41005 ) ) ;
#48694 = CARTESIAN_POINT ( 'NONE',  ( 18.82465703714932204, -7.861812626244089053, 11.49999999999998934 ) ) ;
#48695 = ORIENTED_EDGE ( 'NONE', *, *, #49672, .T. ) ;
#48696 = VERTEX_POINT ( 'NONE', #13625 ) ;
#48697 = CARTESIAN_POINT ( 'NONE',  ( 18.48385363477634513, -13.70420857335572506, -1.500000000000002220 ) ) ;
#48698 = CARTESIAN_POINT ( 'NONE',  ( -1.653359744423585465, -5.876774720514412742, 19.34586827028017098 ) ) ;
#48699 = ORIENTED_EDGE ( 'NONE', *, *, #83832, .F. ) ;
#48700 = FACE_OUTER_BOUND ( 'NONE', #66432, .T. ) ;
#48701 = CARTESIAN_POINT ( 'NONE',  ( -125.6228709571500559, -23.47593901973091235, -1.443836447538995760 ) ) ;
#48703 = CARTESIAN_POINT ( 'NONE',  ( -95.51303906205738770, -24.15503026093913874, -0.2815557561904519224 ) ) ;
#48702 = AXIS2_PLACEMENT_3D ( 'NONE', #25745, #80528, #33856 ) ;
#48704 = FACE_OUTER_BOUND ( 'NONE', #8041, .T. ) ;
#48706 = EDGE_LOOP ( 'NONE', ( #65573, #15844, #96982, #84193 ) ) ;
#48705 = CARTESIAN_POINT ( 'NONE',  ( 6.557060941508195739, 20.25493142521265355, 11.49999999999999645 ) ) ;
#48707 = VECTOR ( 'NONE', #35949, 1000.000000000000114 ) ;
#48708 = EDGE_LOOP ( 'NONE', ( #82732, #91239, #43381, #98982 ) ) ;
#48709 = CARTESIAN_POINT ( 'NONE',  ( -7.359855604737914447, 20.98419016808480109, 11.49999999999998934 ) ) ;
#48710 = CARTESIAN_POINT ( 'NONE',  ( 6.115004186001010922, -19.73231167505474559, -1.500000000000002220 ) ) ;
#48711 = ADVANCED_FACE ( 'NONE', ( #60338 ), #28869, .T. ) ;
#48712 = AXIS2_PLACEMENT_3D ( 'NONE', #76548, #69457, #949 ) ;
#48713 = ORIENTED_EDGE ( 'NONE', *, *, #80476, .F. ) ;
#48714 = CARTESIAN_POINT ( 'NONE',  ( -6.072964844751159497, -6.376774720514410077, 19.44316438561912008 ) ) ;
#48715 = EDGE_CURVE ( 'NONE', #99009, #46879, #56742, .T. ) ;
#48716 = CARTESIAN_POINT ( 'NONE',  ( -95.62584158020946745, -24.83644354573579349, 8.397322867130096569 ) ) ;
#48717 = ORIENTED_EDGE ( 'NONE', *, *, #79791, .T. ) ;
#48718 = CARTESIAN_POINT ( 'NONE',  ( -95.52287095715003318, -24.14321612903117753, -0.2833117244520895750 ) ) ;
#48719 = EDGE_LOOP ( 'NONE', ( #67992, #36183, #38556, #61713 ) ) ;
#48720 = CARTESIAN_POINT ( 'NONE',  ( 5.959527149828093506, -3.316774720514425567, -28.45540529974545407 ) ) ;
#48721 = DIRECTION ( 'NONE',  ( 0.000000000000000000, -1.000000000000000000, 0.000000000000000000 ) ) ;
#48722 = CARTESIAN_POINT ( 'NONE',  ( 20.33208665566141704, 4.825383418962623239, -1.500000000000002220 ) ) ;
#48723 = CARTESIAN_POINT ( 'NONE',  ( -19.96805355746080934, -8.928269573510897672, 11.49999999999999645 ) ) ;
#48724 = CARTESIAN_POINT ( 'NONE',  ( -73.63478229892059801, -24.15620529776628089, 10.23563542870660470 ) ) ;
#48725 = PLANE ( 'NONE',  #92069 ) ;
#48726 = CARTESIAN_POINT ( 'NONE',  ( -18.88510386880526326, 12.19974334031638641, -1.500000000000002220 ) ) ;
#48727 = CARTESIAN_POINT ( 'NONE',  ( 5.579783289733251550, -20.15082174716252794, 11.49999999999998934 ) ) ;
#48728 = CARTESIAN_POINT ( 'NONE',  ( -38.64173560969166488, -24.15543982623906771, -0.2315651400026570161 ) ) ;
#48729 = CARTESIAN_POINT ( 'NONE',  ( -57.62287095715004881, -23.47593901973091235, -1.443836447539007972 ) ) ;
#48730 = CARTESIAN_POINT ( 'NONE',  ( 4.780030342074717886, -5.876774720514424288, 21.16398229115527130 ) ) ;
#48731 = ORIENTED_EDGE ( 'NONE', *, *, #18778, .F. ) ;
#48732 = ORIENTED_EDGE ( 'NONE', *, *, #77808, .T. ) ;
#48733 = ORIENTED_EDGE ( 'NONE', *, *, #13227, .F. ) ;
#48734 = CARTESIAN_POINT ( 'NONE',  ( -52.56777431719391558, -23.48783264082478794, -1.443836473390069708 ) ) ;
#48735 = ORIENTED_EDGE ( 'NONE', *, *, #57358, .T. ) ;
#48736 = CARTESIAN_POINT ( 'NONE',  ( -21.12015818079280649, -3.594773940630530795, -1.500000000000002220 ) ) ;
#48737 = CARTESIAN_POINT ( 'NONE',  ( -8.633843874998758494, 20.65557450359631630, 11.49999999999999645 ) ) ;
#48738 = EDGE_LOOP ( 'NONE', ( #51501, #32997, #33833, #64505 ) ) ;
#48739 = FACE_OUTER_BOUND ( 'NONE', #68302, .T. ) ;
#48740 = CARTESIAN_POINT ( 'NONE',  ( 16.02493003730957000, -13.65669227992738577, 11.49999999999998934 ) ) ;
#48741 = CARTESIAN_POINT ( 'NONE',  ( -30.48805280194831369, -24.57390550863043899, 9.174392229302920754 ) ) ;
#48742 = CARTESIAN_POINT ( 'NONE',  ( -12.53609265798794681, -15.47265773855268378, -1.500000000000002220 ) ) ;
#48743 = DIRECTION ( 'NONE',  ( 1.000000000000000000, -0.000000000000000000, 0.000000000000000000 ) ) ;
#48744 = CARTESIAN_POINT ( 'NONE',  ( -80.84160375922890296, -25.29534361467446502, 4.579768035494214296 ) ) ;
#48745 = CARTESIAN_POINT ( 'NONE',  ( 21.84380375219137349, -3.031640915038902762, -1.500000000000002220 ) ) ;
#48746 = ORIENTED_EDGE ( 'NONE', *, *, #84471, .T. ) ;
#48747 = CARTESIAN_POINT ( 'NONE',  ( -65.53456971742291159, -24.83644354573578994, 8.397322867130098345 ) ) ;
#48748 = CARTESIAN_POINT ( 'NONE',  ( -2.243088942307695177, -6.376774720514408301, 19.14743589743590491 ) ) ;
#48749 = CARTESIAN_POINT ( 'NONE',  ( 20.57277012135545036, 3.371850554975475145, 11.49999999999999645 ) ) ;
#48750 = CARTESIAN_POINT ( 'NONE',  ( -28.41196290477738273, -24.69444547851099614, 8.290116722409051064 ) ) ;
#48751 = CARTESIAN_POINT ( 'NONE',  ( -27.51841088719901052, -24.59198966350803772, 1.634211142568063213 ) ) ;
#48752 = CARTESIAN_POINT ( 'NONE',  ( 2.230654205607476293, 0.1647943925233646134, -7.514475724998474108E-17 ) ) ;
#48753 = CARTESIAN_POINT ( 'NONE',  ( 0.2649960030224881025, 21.33594185153759426, -1.500000000000002220 ) ) ;
#48754 = CARTESIAN_POINT ( 'NONE',  ( -9.940598223437573822, -5.876774720514426953, 21.78128695274315874 ) ) ;
#48755 = CARTESIAN_POINT ( 'NONE',  ( 27.53860345374808105, 5.356774720514425603, -6.982392034746242260 ) ) ;
#48756 = VECTOR ( 'NONE', #23097, 1000.000000000000114 ) ;
#48757 = CARTESIAN_POINT ( 'NONE',  ( 22.02124265030973760, -6.376774720514428729, 16.20402280011862217 ) ) ;
#48758 = PLANE ( 'NONE',  #29711 ) ;
#48759 = CARTESIAN_POINT ( 'NONE',  ( -14.53490578827140212, -17.26895500059623956, -1.500000000000002220 ) ) ;
#48760 = CARTESIAN_POINT ( 'NONE',  ( -68.62287095715005592, -29.50250243563736774, 8.947779886222143375 ) ) ;
#48761 = EDGE_LOOP ( 'NONE', ( #98832, #79484, #33950, #73044 ) ) ;
#48762 = CARTESIAN_POINT ( 'NONE',  ( 12.90232279286373185, 3.316774720514426456, -28.14923833570356493 ) ) ;
#48763 = CARTESIAN_POINT ( 'NONE',  ( 7.545203588713008003, -10.70224338845203071, 1.194977652177498628 ) ) ;
#48764 = CARTESIAN_POINT ( 'NONE',  ( 2.169241753049089727, -19.58708112974024829, 11.49999999999999645 ) ) ;
#48765 = CARTESIAN_POINT ( 'NONE',  ( -32.07722060962683486, -25.28405270565852447, 3.734159825085341833 ) ) ;
#48766 = CARTESIAN_POINT ( 'NONE',  ( -28.98875734969026041, 5.965225279485572685, 23.37402280011862743 ) ) ;
#48767 = ORIENTED_EDGE ( 'NONE', *, *, #56912, .F. ) ;
#48768 = CARTESIAN_POINT ( 'NONE',  ( -111.5228709571500474, -24.50216790748206108, 0.6166512839542542812 ) ) ;
#48769 = CARTESIAN_POINT ( 'NONE',  ( -99.52287095715009002, -24.66019654487200441, 8.947790411086119278 ) ) ;
#48770 = EDGE_CURVE ( 'NONE', #86899, #100313, #55694, .T. ) ;
#48771 = CARTESIAN_POINT ( 'NONE',  ( -61.52287095715005449, -24.35013146730203815, 9.818937971375103047 ) ) ;
#48772 = CARTESIAN_POINT ( 'NONE',  ( -97.62287095715005592, -29.50248528299804818, 1.056150453629042030 ) ) ;
#48773 = CARTESIAN_POINT ( 'NONE',  ( -32.99388727629348494, -25.12026506542017046, 2.831122744435439209 ) ) ;
#48774 = EDGE_CURVE ( 'NONE', #48827, #91131, #83298, .T. ) ;
#48775 = DIRECTION ( 'NONE',  ( 0.000000000000000000, -2.173523156925979552E-06, 0.9999999999976378895 ) ) ;
#48776 = CARTESIAN_POINT ( 'NONE',  ( 9.697495225759652726, 17.24774500829319734, 11.49999999999998934 ) ) ;
#48777 = AXIS2_PLACEMENT_3D ( 'NONE', #98637, #14401, #66234 ) ;
#48778 = ORIENTED_EDGE ( 'NONE', *, *, #60912, .F. ) ;
#48779 = ADVANCED_FACE ( 'NONE', ( #97866 ), #6025, .T. ) ;
#48780 = VECTOR ( 'NONE', #34598, 1000.000000000000114 ) ;
#48781 = CARTESIAN_POINT ( 'NONE',  ( 15.40757771627215256, 13.04930689719894765, 11.49999999999999645 ) ) ;
#48782 = CARTESIAN_POINT ( 'NONE',  ( 5.817949855437939632, -5.876774720514417183, 20.34349022145623209 ) ) ;
#48783 = EDGE_CURVE ( 'NONE', #43385, #76243, #60327, .T. ) ;
#48784 = B_SPLINE_CURVE_WITH_KNOTS ( 'NONE', 3,
 ( #11026, #73431, #41995, #88656, #34864, #58209, #19625, #50587 ),
 .UNSPECIFIED., .F., .F.,
 ( 4, 2, 2, 4 ),
 ( 0.06220205793350375156, 0.06492579111525004221, 0.06628765770612317365, 0.06764952429699631897 ),
 .UNSPECIFIED. ) ;
#48785 = ORIENTED_EDGE ( 'NONE', *, *, #29255, .T. ) ;
#48786 = CARTESIAN_POINT ( 'NONE',  ( -10.40290173325841216, 6.376774720514426953, 27.45402280011861862 ) ) ;
#48787 = CARTESIAN_POINT ( 'NONE',  ( -70.10882455230809285, -25.30100131183307610, 5.336495488474668036 ) ) ;
#48788 = CARTESIAN_POINT ( 'NONE',  ( 8.499999999999989342, 18.74999999999999645, 2.100000000000000089 ) ) ;
#48789 = CARTESIAN_POINT ( 'NONE',  ( -122.5895376238167245, -23.47596703998600631, 11.44779298504227683 ) ) ;
#48790 = B_SPLINE_CURVE_WITH_KNOTS ( 'NONE', 3,
 ( #65894, #35427, #2985, #66389, #58268, #49165 ),
 .UNSPECIFIED., .F., .F.,
 ( 4, 2, 4 ),
 ( 0.000000000000000000, 0.001380901958385383991, 0.002761803916770767982 ),
 .UNSPECIFIED. ) ;
#48791 = CARTESIAN_POINT ( 'NONE',  ( -52.62287095715005592, -24.64898659630367561, 1.056161002820821038 ) ) ;
#48792 = FACE_OUTER_BOUND ( 'NONE', #12216, .T. ) ;
#48793 = CARTESIAN_POINT ( 'NONE',  ( 5.980626343040887249, -19.09133569553460319, 11.49999999999998934 ) ) ;
#48794 = EDGE_CURVE ( 'NONE', #58098, #65974, #78521, .T. ) ;
#48795 = CARTESIAN_POINT ( 'NONE',  ( -57.62287095715004881, -24.66019654487199020, 8.947790411086131712 ) ) ;
#48796 = VERTEX_POINT ( 'NONE', #47604 ) ;
#48797 = CARTESIAN_POINT ( 'NONE',  ( -79.55873576538276382, -23.73791477778911840, 11.05961554403170943 ) ) ;
#48798 = CARTESIAN_POINT ( 'NONE',  ( -35.48363359496615743, -24.52300882791529446, 0.6510814631126419227 ) ) ;
#48799 = CARTESIAN_POINT ( 'NONE',  ( -79.48084051826894836, -25.29803721465439637, 5.434463432368143998 ) ) ;
#48800 = DIRECTION ( 'NONE',  ( -1.000000000000000000, 0.000000000000000000, 0.000000000000000000 ) ) ;
#48801 = B_SPLINE_CURVE_WITH_KNOTS ( 'NONE', 3,
 ( #84776, #77656, #85788, #92884 ),
 .UNSPECIFIED., .F., .F.,
 ( 4, 4 ),
 ( 0.000000000000000000, 9.999999999998897304E-05 ),
 .UNSPECIFIED. ) ;
#48802 = CARTESIAN_POINT ( 'NONE',  ( -73.58797577400544299, -24.34968618360933590, 0.1864209137778805869 ) ) ;
#48803 = CARTESIAN_POINT ( 'NONE',  ( 14.47435193431689449, 3.621805754985667036, -28.36943713370744646 ) ) ;
#48804 = CARTESIAN_POINT ( 'NONE',  ( -101.9682441342847596, -25.32724633150699844, 4.398074151685130495 ) ) ;
#48805 = ORIENTED_EDGE ( 'NONE', *, *, #49340, .T. ) ;
#48806 = CARTESIAN_POINT ( 'NONE',  ( 14.61151973098085222, 14.07909450314327771, 11.49999999999998934 ) ) ;
#48807 = ORIENTED_EDGE ( 'NONE', *, *, #59759, .T. ) ;
#48808 = DIRECTION ( 'NONE',  ( 2.246662546894773332E-15, 0.000000000000000000, 1.000000000000000000 ) ) ;
#48809 = CARTESIAN_POINT ( 'NONE',  ( -127.5554365995002541, -24.35071581493544102, 9.817618358456009275 ) ) ;
#48810 = CARTESIAN_POINT ( 'NONE',  ( -59.57899832961151532, -24.66019654487199730, 8.947790411086124607 ) ) ;
#48812 = EDGE_CURVE ( 'NONE', #57023, #76713, #39453, .T. ) ;
#48811 = DIRECTION ( 'NONE',  ( -0.2164396139380965478, 0.9762960071199346945, 0.000000000000000000 ) ) ;
#48813 = CARTESIAN_POINT ( 'NONE',  ( -30.47287095715007510, -24.98308899733239130, 7.804029986632581739 ) ) ;
#48814 = CARTESIAN_POINT ( 'NONE',  ( -17.67215177357914513, -11.65580189297658897, 11.49999999999999645 ) ) ;
#48815 = B_SPLINE_CURVE_WITH_KNOTS ( 'NONE', 3,
 ( #56060, #17480, #40817, #33204 ),
 .UNSPECIFIED., .F., .F.,
 ( 4, 4 ),
 ( 0.4801287726817814461, 0.4891352039538970353 ),
 .UNSPECIFIED. ) ;
#48816 = CARTESIAN_POINT ( 'NONE',  ( 21.13975321936677787, -6.629177502137091338, -1.500000000000002220 ) ) ;
#48817 = CIRCLE ( 'NONE', #84434, 1.500000000000000666 ) ;
#48818 = EDGE_CURVE ( 'NONE', #43756, #63195, #42184, .T. ) ;
#48819 = CARTESIAN_POINT ( 'NONE',  ( 7.805751503010069037, -19.01748540344778959, 11.49999999999998934 ) ) ;
#48820 = ORIENTED_EDGE ( 'NONE', *, *, #52069, .T. ) ;
#48821 = DIRECTION ( 'NONE',  ( 0.000000000000000000, -2.173523156925979552E-06, 0.9999999999976378895 ) ) ;
#48822 = ORIENTED_EDGE ( 'NONE', *, *, #22368, .T. ) ;
#48823 = CARTESIAN_POINT ( 'NONE',  ( -54.58256300931693517, -24.51314013834315020, 0.6176544820404069602 ) ) ;
#48824 = CARTESIAN_POINT ( 'NONE',  ( -70.52287095715007581, -24.51254535375844412, 9.355368624242185405 ) ) ;
#48825 = ORIENTED_EDGE ( 'NONE', *, *, #39586, .F. ) ;
#48826 = ORIENTED_EDGE ( 'NONE', *, *, #64247, .T. ) ;
#48827 = VERTEX_POINT ( 'NONE', #72314 ) ;
#48828 = CARTESIAN_POINT ( 'NONE',  ( -110.5097208737972778, -25.12185449762653278, 2.839826584255876973 ) ) ;
#48829 = CARTESIAN_POINT ( 'NONE',  ( 6.658651924251966392, -5.876774720514415407, 20.11748569626183425 ) ) ;
#48830 = CARTESIAN_POINT ( 'NONE',  ( 8.676776695296462449, 18.57322330470351091, 2.100000000000000089 ) ) ;
#48831 = CARTESIAN_POINT ( 'NONE',  ( 20.27745880512110688, -4.159726151199424571, -1.500000000000002220 ) ) ;
#48832 = CARTESIAN_POINT ( 'NONE',  ( 3.837509532605410278, -21.31939230324424628, 11.49999999999999645 ) ) ;
#48833 = ORIENTED_EDGE ( 'NONE', *, *, #84216, .F. ) ;
#48834 = CARTESIAN_POINT ( 'NONE',  ( -127.5895376238167245, -24.65952944569305316, 1.056160979905710118 ) ) ;
#48835 = CARTESIAN_POINT ( 'NONE',  ( -24.90875734969025501, -6.376774720514426953, 29.49402280011861777 ) ) ;
#48836 = CARTESIAN_POINT ( 'NONE',  ( -4.914914792326205983, -21.87198836336805385, -1.500000000000002220 ) ) ;
#48837 = CARTESIAN_POINT ( 'NONE',  ( -33.62287095715005592, -24.64965695001467694, 8.947790433994189385 ) ) ;
#48838 = CARTESIAN_POINT ( 'NONE',  ( -71.62287095715007013, -24.51283580621364777, 0.6167428607019787012 ) ) ;
#48839 = ORIENTED_EDGE ( 'NONE', *, *, #42707, .F. ) ;
#48840 = CARTESIAN_POINT ( 'NONE',  ( -87.52287095715006160, -23.47596703998600631, 11.44779298504228393 ) ) ;
#48841 = VECTOR ( 'NONE', #89807, 1000.000000000000114 ) ;
#48842 = CARTESIAN_POINT ( 'NONE',  ( -120.6228709571500275, -24.52323809116984776, 9.355190652339421931 ) ) ;
#48843 =( GEOMETRIC_REPRESENTATION_CONTEXT ( 3 ) GLOBAL_UNCERTAINTY_ASSIGNED_CONTEXT ( ( #60147 ) ) GLOBAL_UNIT_ASSIGNED_CONTEXT ( ( #1366, #84081, #14571 ) ) REPRESENTATION_CONTEXT ( 'NONE', 'WORKASPACE' ) );
#48844 = ORIENTED_EDGE ( 'NONE', *, *, #22287, .F. ) ;
#48845 = ORIENTED_EDGE ( 'NONE', *, *, #42463, .F. ) ;
#48846 = CARTESIAN_POINT ( 'NONE',  ( -8.160000000000000142, 0.000000000000000000, 0.000000000000000000 ) ) ;
#48847 = APPROVAL ( #72351, 'UNSPECIFIED' ) ;
#48848 = ORIENTED_EDGE ( 'NONE', *, *, #60145, .T. ) ;
#48849 = CARTESIAN_POINT ( 'NONE',  ( -94.62287095715005592, -24.64898659630528854, 1.056161002820827921 ) ) ;
#48850 = CARTESIAN_POINT ( 'NONE',  ( 9.380127297304197143, -19.07726845333505494, -1.500000000000002220 ) ) ;
#48851 = EDGE_LOOP ( 'NONE', ( #14747, #19824, #63101, #64307 ) ) ;
#48852 = DIRECTION ( 'NONE',  ( 0.000000000000000000, 2.173523156925980399E-06, -0.9999999999976378895 ) ) ;
#48853 = CARTESIAN_POINT ( 'NONE',  ( -15.20188179817220231, 15.67080601223297442, -1.500000000000002220 ) ) ;
#48854 = CARTESIAN_POINT ( 'NONE',  ( -52.50765823405691890, -23.96169478059712787, 10.65365249895718769 ) ) ;
#48855 = PLANE ( 'NONE',  #32321 ) ;
#48856 = DIRECTION ( 'NONE',  ( -1.000000000000000000, -3.773278334444166432E-23, -8.201307841325785021E-29 ) ) ;
#48857 = CARTESIAN_POINT ( 'NONE',  ( -12.54888962926113827, 17.92887824059606672, -1.500000000000002220 ) ) ;
#48858 = DIRECTION ( 'NONE',  ( -1.000000000000000000, 0.000000000000000000, -4.956352788505167212E-16 ) ) ;
#48859 = ORIENTED_EDGE ( 'NONE', *, *, #73490, .F. ) ;
#48860 = DIRECTION ( 'NONE',  ( 0.000000000000000000, -1.000000000000000000, 0.000000000000000000 ) ) ;
#48861 = DIRECTION ( 'NONE',  ( 0.000000000000000000, 1.000000000000000000, 0.000000000000000000 ) ) ;
#48862 = ORIENTED_EDGE ( 'NONE', *, *, #40204, .T. ) ;
#48863 = EDGE_LOOP ( 'NONE', ( #96520, #64217 ) ) ;
#48864 = ORIENTED_EDGE ( 'NONE', *, *, #40405, .T. ) ;
#48865 = PLANE ( 'NONE',  #54040 ) ;
#48866 = PLANE ( 'NONE',  #23819 ) ;
#48867 = CARTESIAN_POINT ( 'NONE',  ( 7.950249384483326409, 19.69624408967213469, -1.500000000000002220 ) ) ;
#48868 = PLANE ( 'NONE',  #92006 ) ;
#48869 = CARTESIAN_POINT ( 'NONE',  ( -30.59326697242301663, -24.88273649812090227, 8.549170486301877148 ) ) ;
#48870 = DIRECTION ( 'NONE',  ( 3.773278334444166432E-23, -1.000000000000000000, 0.000000000000000000 ) ) ;
#48871 = DIRECTION ( 'NONE',  ( 0.06916465693916194757, 0.000000000000000000, -0.9976052577199501226 ) ) ;
#48872 = ADVANCED_BREP_SHAPE_REPRESENTATION ( '', ( #8332, #37391 ), #48843 ) ;
#48873 = CARTESIAN_POINT ( 'NONE',  ( -10.03281922573575002, -16.61734169602722488, -1.500000000000002220 ) ) ;
#48874 = CARTESIAN_POINT ( 'NONE',  ( -117.5520235238924158, -24.66019654487200441, 8.947790411086112172 ) ) ;
#48875 = ORIENTED_EDGE ( 'NONE', *, *, #80119, .T. ) ;
#48876 = CARTESIAN_POINT ( 'NONE',  ( -8.384790838521158918, 17.58144419890746235, 11.49999999999999645 ) ) ;
#48877 = CARTESIAN_POINT ( 'NONE',  ( 31.61049571213237641, -4.540774720514426654, 26.28206907949443050 ) ) ;
#48878 = EDGE_CURVE ( 'NONE', #26341, #50456, #78018, .T. ) ;
#48879 = FACE_OUTER_BOUND ( 'NONE', #12727, .T. ) ;
#48880 = EDGE_LOOP ( 'NONE', ( #34452, #77383, #16715, #6894 ) ) ;
#48881 = CARTESIAN_POINT ( 'NONE',  ( 4.465438306463536122, -6.376774720514426065, 21.59631214011467293 ) ) ;
#48882 = CARTESIAN_POINT ( 'NONE',  ( -75.62287095715011276, -23.85196035786901803, -0.8779234886475031363 ) ) ;
#48883 = LINE ( 'NONE', #26029, #201 ) ;
#48884 = CARTESIAN_POINT ( 'NONE',  ( -81.73829046040381741, -25.03155895851643464, 6.803918155767815001 ) ) ;
#48885 = CARTESIAN_POINT ( 'NONE',  ( 6.681059570357060551, -18.48443787736713873, 11.49999999999998934 ) ) ;
#48886 = ORIENTED_EDGE ( 'NONE', *, *, #31089, .F. ) ;
#48887 = EDGE_CURVE ( 'NONE', #60374, #79287, #22721, .T. ) ;
#48888 = AXIS2_PLACEMENT_3D ( 'NONE', #13932, #90564, #43900 ) ;
#48889 = FACE_OUTER_BOUND ( 'NONE', #44835, .T. ) ;
#48890 = CARTESIAN_POINT ( 'NONE',  ( 19.40787663092975279, -12.54570180764831377, -1.500000000000002220 ) ) ;
#48891 = ADVANCED_FACE ( 'NONE', ( #92751 ), #23236, .T. ) ;
#48892 = B_SPLINE_CURVE_WITH_KNOTS ( 'NONE', 3,
 ( #24254, #16637, #30363, #30869 ),
 .UNSPECIFIED., .F., .F.,
 ( 4, 4 ),
 ( 0.000000000000000000, 0.001418231214350569244 ),
 .UNSPECIFIED. ) ;
#48893 = DATE_AND_TIME ( #96057, #362 ) ;
#48894 = LINE ( 'NONE', #26038, #48331 ) ;
#48895 = PLANE ( 'NONE',  #78189 ) ;
#48896 = CARTESIAN_POINT ( 'NONE',  ( -109.4136617073600917, -25.16309701932601328, 3.145511876789759853 ) ) ;
#48897 = CARTESIAN_POINT ( 'NONE',  ( -63.52287095715006160, -29.50250786944525672, 11.44777988621623876 ) ) ;
#48898 = DIRECTION ( 'NONE',  ( -0.000000000000000000, -1.000000000000000000, -0.000000000000000000 ) ) ;
#48899 = CARTESIAN_POINT ( 'NONE',  ( 6.326958800731953048, -5.876774720514425177, 21.47849181751607972 ) ) ;
#48900 = LINE ( 'NONE', #10323, #89438 ) ;
#48901 = CARTESIAN_POINT ( 'NONE',  ( 27.53860345374771867, -1.682774720514426114, -9.482392034746242260 ) ) ;
#48902 = CARTESIAN_POINT ( 'NONE',  ( -18.69216024341242743, -6.879743215651725308, -1.500000000000002220 ) ) ;
#48903 = ADVANCED_FACE ( 'NONE', ( #34252 ), #41128, .F. ) ;
#48904 = DIRECTION ( 'NONE',  ( 1.000000000000000000, 3.773278334444167608E-23, 8.201307833595939069E-29 ) ) ;
#48905 = CARTESIAN_POINT ( 'NONE',  ( -10.37884456512175291, 16.95428827495986823, -1.500000000000002220 ) ) ;
#48906 = ORIENTED_EDGE ( 'NONE', *, *, #88785, .T. ) ;
#48907 = DIRECTION ( 'NONE',  ( -3.773278334453079030E-23, 0.9999999999976377785, 2.173523156925979128E-06 ) ) ;
#48908 = AXIS2_PLACEMENT_3D ( 'NONE', #54003, #77310, #38755 ) ;
#48909 = SECURITY_CLASSIFICATION ( '', '', #49521 ) ;
#48910 = CARTESIAN_POINT ( 'NONE',  ( -125.5228709571500900, -24.62226745350437795, 0.9660975649728180681 ) ) ;
#48911 = CARTESIAN_POINT ( 'NONE',  ( 7.844850387708879325, -6.376774720514429617, -25.09814097568368751 ) ) ;
#48912 = CARTESIAN_POINT ( 'NONE',  ( -8.830788454959730416, 18.81286502489961876, 11.49999999999999645 ) ) ;
#48913 = CARTESIAN_POINT ( 'NONE',  ( -7.338700834008208496, -6.376774720514410077, 19.35116211686183263 ) ) ;
#48914 = CARTESIAN_POINT ( 'NONE',  ( -29.49875734969026198, 0.3587747205144265483, 10.11402280011862587 ) ) ;
#48915 = CARTESIAN_POINT ( 'NONE',  ( 21.04450177026006230, 8.645109164175620364, 11.49999999999999645 ) ) ;
#48916 = ORIENTED_EDGE ( 'NONE', *, *, #89645, .F. ) ;
#48917 = DIRECTION ( 'NONE',  ( 3.773278334444167608E-23, -1.000000000000000000, 0.000000000000000000 ) ) ;
#48918 = CARTESIAN_POINT ( 'NONE',  ( 23.60872659128563456, -0.9000000000000000222, 2.097483029078133665 ) ) ;
#48919 = VERTEX_POINT ( 'NONE', #57102 ) ;
#48920 = CARTESIAN_POINT ( 'NONE',  ( -6.636546740042271963, -19.09123619949631134, 11.49999999999998934 ) ) ;
#48921 = EDGE_CURVE ( 'NONE', #14248, #37175, #54221, .T. ) ;
#48922 = CARTESIAN_POINT ( 'NONE',  ( 7.480769230769231726, -6.376774720514420736, 20.77403846153845635 ) ) ;
#48923 = B_SPLINE_CURVE_WITH_KNOTS ( 'NONE', 3,
 ( #49416, #72747, #21801, #27063 ),
 .UNSPECIFIED., .F., .F.,
 ( 4, 4 ),
 ( 0.000000000000000000, 9.999999999998897304E-05 ),
 .UNSPECIFIED. ) ;
#48924 = DIRECTION ( 'NONE',  ( 0.000000000000000000, 0.000000000000000000, -1.000000000000000000 ) ) ;
#48925 = CARTESIAN_POINT ( 'NONE',  ( -51.62287095715005592, -23.48786465467241413, 11.44779295918254824 ) ) ;
#48926 = ORIENTED_EDGE ( 'NONE', *, *, #34997, .T. ) ;
#48927 = DIRECTION ( 'NONE',  ( -1.000000000000000000, 0.000000000000000000, 0.000000000000000000 ) ) ;
#48928 = CARTESIAN_POINT ( 'NONE',  ( -104.5895376238167245, -23.47596703998600631, 11.44779298504227683 ) ) ;
#48929 = CARTESIAN_POINT ( 'NONE',  ( -13.81204400269958654, 14.50282280199826701, -1.500000000000002220 ) ) ;
#48930 = CARTESIAN_POINT ( 'NONE',  ( 17.15856466979341377, 12.00972951212132855, 11.49999999999999645 ) ) ;
#48931 = CARTESIAN_POINT ( 'NONE',  ( -54.62287095715005592, -24.66019654487199020, 8.947790411086135265 ) ) ;
#48932 = CARTESIAN_POINT ( 'NONE',  ( -124.6228709571500701, -23.47596703998600631, 11.44779298504227860 ) ) ;
#48933 = CARTESIAN_POINT ( 'NONE',  ( 21.84380375219137349, -3.031640915038902762, -1.500000000000002220 ) ) ;
#48934 = LINE ( 'NONE', #4255, #59277 ) ;
#48936 = ORIENTED_EDGE ( 'NONE', *, *, #33179, .T. ) ;
#48935 = EDGE_CURVE ( 'NONE', #9106, #18610, #62328, .T. ) ;
#48937 = VECTOR ( 'NONE', #19013, 1000.000000000000000 ) ;
#48938 = CARTESIAN_POINT ( 'NONE',  ( -60.52287095715006870, -23.84047902841601996, -0.8780736468305723186 ) ) ;
#48939 = CARTESIAN_POINT ( 'NONE',  ( -9.149999999999996803, -5.876774720514426953, 11.88602120139452012 ) ) ;
#48940 = CARTESIAN_POINT ( 'NONE',  ( -72.58794503245407270, -24.34968618360933590, 0.1864209137778795600 ) ) ;
#48941 = ORIENTED_EDGE ( 'NONE', *, *, #98674, .F. ) ;
#48942 = DIRECTION ( 'NONE',  ( -8.334928612639484546E-17, 1.000000000000000000, -7.321843366904296032E-17 ) ) ;
#48943 = ORIENTED_EDGE ( 'NONE', *, *, #21230, .T. ) ;
#48944 = ORIENTED_EDGE ( 'NONE', *, *, #3781, .F. ) ;
#48945 = CARTESIAN_POINT ( 'NONE',  ( 13.10664265030973930, 5.965225279485574461, -28.18129937516157568 ) ) ;
#48946 = LINE ( 'NONE', #86493, #98850 ) ;
#48947 = CARTESIAN_POINT ( 'NONE',  ( -58.62287095715006302, -24.34917612406837861, 0.1852690917426618733 ) ) ;
#48948 = CARTESIAN_POINT ( 'NONE',  ( 17.96566822227200433, 9.963707542159163211, -1.500000000000002220 ) ) ;
#48949 = ORIENTED_EDGE ( 'NONE', *, *, #95999, .T. ) ;
#48950 = CARTESIAN_POINT ( 'NONE',  ( -7.749999999999996447, 24.84999999999999787, 2.100000000000000089 ) ) ;
#48951 = DIRECTION ( 'NONE',  ( 0.000000000000000000, 1.000000000000000000, 1.478457507934778393E-16 ) ) ;
#48952 = CARTESIAN_POINT ( 'NONE',  ( -83.52287095715009002, -23.73907113216989373, -1.053371485793249684 ) ) ;
#48953 = CARTESIAN_POINT ( 'NONE',  ( -21.40455707349245529, -6.346402434563959361, -1.500000000000002220 ) ) ;
#48954 = CARTESIAN_POINT ( 'NONE',  ( -71.25156906290497716, -25.22179730619566840, 6.511357954259892722 ) ) ;
#48955 = CARTESIAN_POINT ( 'NONE',  ( -41.32836283488544638, -2.803225279485573207, 39.26872235229541985 ) ) ;
#48956 = VERTEX_POINT ( 'NONE', #85653 ) ;
#48957 = CARTESIAN_POINT ( 'NONE',  ( -32.08503310962682065, -24.86181185134534388, 1.747789972853592833 ) ) ;
#48958 = DIRECTION ( 'NONE',  ( 0.000000000000000000, 0.000000000000000000, -1.000000000000000000 ) ) ;
#48959 = CARTESIAN_POINT ( 'NONE',  ( -13.77211689728001964, -15.67653869864640903, 11.49999999999998934 ) ) ;
#48960 = CIRCLE ( 'NONE', #3620, 0.3000000000000016542 ) ;
#48961 = ORIENTED_EDGE ( 'NONE', *, *, #37976, .F. ) ;
#48963 = ORIENTED_EDGE ( 'NONE', *, *, #95900, .T. ) ;
#48962 = DIRECTION ( 'NONE',  ( 1.000000000000000000, 0.000000000000000000, -5.238131417152343399E-15 ) ) ;
#48964 = ADVANCED_FACE ( 'NONE', ( #96151 ), #16134, .F. ) ;
#48965 = ORIENTED_EDGE ( 'NONE', *, *, #27804, .T. ) ;
#48966 = CARTESIAN_POINT ( 'NONE',  ( -62.62287095715004881, -29.50250243563736774, 8.947779886222145151 ) ) ;
#48967 = CARTESIAN_POINT ( 'NONE',  ( -13.78326148797977169, 15.88460234914768421, -1.500000000000002220 ) ) ;
#48968 = ORIENTED_EDGE ( 'NONE', *, *, #94579, .T. ) ;
#48969 = CARTESIAN_POINT ( 'NONE',  ( 8.160000000000000142, 9.789768006247301813, -0.8564937190954607926 ) ) ;
#48970 = CARTESIAN_POINT ( 'NONE',  ( -53.52287095715006160, -24.50321055353805377, 9.387540953477522265 ) ) ;
#48971 = CARTESIAN_POINT ( 'NONE',  ( -120.6245363983109655, -24.73531770709095312, 8.716586749053508498 ) ) ;
#48972 = EDGE_CURVE ( 'NONE', #15899, #45653, #8530, .T. ) ;
#48973 = CARTESIAN_POINT ( 'NONE',  ( -100.9913061220214843, -25.03152431204875583, 7.480517603216952693 ) ) ;
#48974 = CARTESIAN_POINT ( 'NONE',  ( -49.55620429048340014, -24.64898659630528499, 1.056161002820822592 ) ) ;
#48975 = CARTESIAN_POINT ( 'NONE',  ( 12.10466045530642631, 18.00204671274030233, -1.500000000000002220 ) ) ;
#48976 = CARTESIAN_POINT ( 'NONE',  ( 0.2311345937353457003, -6.376774720514410077, 19.43951662020192828 ) ) ;
#48978 = ORIENTED_EDGE ( 'NONE', *, *, #54588, .F. ) ;
#48977 = CARTESIAN_POINT ( 'NONE',  ( -13.27262489239681997, 17.90159134968837051, 11.49999999999999645 ) ) ;
#48979 = CARTESIAN_POINT ( 'NONE',  ( -51.52764846858840997, -25.31441937397667274, 6.187572642957288593 ) ) ;
#48980 = CARTESIAN_POINT ( 'NONE',  ( -87.52287095715006160, -23.48783264083352762, -1.443836473376473695 ) ) ;
#48981 = VERTEX_POINT ( 'NONE', #8023 ) ;
#48982 = B_SPLINE_CURVE_WITH_KNOTS ( 'NONE', 3,
 ( #97160, #90047, #20517, #29137 ),
 .UNSPECIFIED., .F., .F.,
 ( 4, 4 ),
 ( 0.5091335765045065243, 0.5101343235452722169 ),
 .UNSPECIFIED. ) ;
#48983 = ADVANCED_FACE ( 'NONE', ( #10911 ), #46098, .T. ) ;
#48984 = EDGE_CURVE ( 'NONE', #92467, #55695, #91745, .T. ) ;
#48986 = ORIENTED_EDGE ( 'NONE', *, *, #34804, .T. ) ;
#48985 = CARTESIAN_POINT ( 'NONE',  ( -118.6228709571500701, -24.50321055353805377, 9.387540953477516936 ) ) ;
#48987 = AXIS2_PLACEMENT_3D ( 'NONE', #39614, #70567, #48243 ) ;
#48988 = ORIENTED_EDGE ( 'NONE', *, *, #46477, .T. ) ;
#48990 = ADVANCED_FACE ( 'NONE', ( #20999 ), #20621, .F. ) ;
#48989 = LOCAL_TIME ( 0, 54, 15.00000000000000000, #98157 ) ;
#48991 = CARTESIAN_POINT ( 'NONE',  ( -57.62287095715004881, -23.47596703998600276, 11.44779298504227683 ) ) ;
#48992 = CARTESIAN_POINT ( 'NONE',  ( 5.670567493371958534, -19.34269084982597775, 11.49999999999998934 ) ) ;
#48993 = CARTESIAN_POINT ( 'NONE',  ( -66.52287095715006160, -24.64965694238407323, 8.947790433994200043 ) ) ;
#48994 = EDGE_LOOP ( 'NONE', ( #80621, #89239, #46813, #56056, #84964, #42465, #64756, #35455, #25376, #5526, #75694, #51564, #84132, #56401, #59069, #60799, #40576, #87270, #34461, #66226, #63289, #33600, #74087, #89892, #16189, #59188, #27507, #81726, #86618, #29100, #42223, #93966, #96498, #67795, #70682, #14404, #38665, #70365, #75421, #82801, #23577, #25970, #89037, #1594, #46205, #12076, #84244, #53063, #3769, #21893 ) ) ;
#48995 = CARTESIAN_POINT ( 'NONE',  ( -130.5728709571501156, -25.24108479417091289, 2.995995577098621077 ) ) ;
#48996 = CARTESIAN_POINT ( 'NONE',  ( 15.70178742502441693, -15.98865493379879332, -1.500000000000002220 ) ) ;
#48997 = EDGE_CURVE ( 'NONE', #47215, #57615, #50979, .T. ) ;
#48998 = VERTEX_POINT ( 'NONE', #66721 ) ;
#48999 = VERTEX_POINT ( 'NONE', #27640 ) ;
#49000 = CARTESIAN_POINT ( 'NONE',  ( -112.5952105876609153, -23.48786465467241769, 11.44779295918253936 ) ) ;
#49001 = CARTESIAN_POINT ( 'NONE',  ( -101.5193634269438405, -23.73791477778911840, 11.05961554403170588 ) ) ;
#49002 = DIRECTION ( 'NONE',  ( -1.000000000000000000, 0.000000000000000000, -0.000000000000000000 ) ) ;
#49003 = CARTESIAN_POINT ( 'NONE',  ( -129.5228709571500758, -23.47596703998600631, 11.44779298504227683 ) ) ;
#49004 = CARTESIAN_POINT ( 'NONE',  ( -97.24578422077173911, -24.82959736273287277, 8.370978854367631783 ) ) ;
#49005 = CARTESIAN_POINT ( 'NONE',  ( -12.82114019720147802, -14.77593736753402709, 11.49999999999998934 ) ) ;
#49006 = B_SPLINE_SURFACE_WITH_KNOTS ( 'NONE', 3, 1, ( 
 ( #43476, #74413 ),
 ( #45967, #63197 ),
 ( #30730, #275 ),
 ( #24107, #55080 ),
 ( #1290, #15492 ),
 ( #86013, #93613 ),
 ( #94120, #22594 ),
 ( #84513, #16489 ),
 ( #100210, #54570 ),
 ( #46456, #32220 ),
 ( #85508, #77386 ),
 ( #47461, #92616 ),
 ( #69293, #84012 ),
 ( #78388, #53588 ),
 ( #24604, #14499 ) ),
 .UNSPECIFIED., .F., .F., .F.,
 ( 4, 1, 1, 1, 1, 1, 1, 1, 1, 1, 1, 1, 4 ),
 ( 2, 2 ),
 ( 0.000000000000000000, 0.07489820792759518953, 0.1485962943439394779, 0.2244712347857275581, 0.3023227423595722940, 0.3819186179896829625, 0.4611486955215912120, 0.5424171227241534332, 0.6267160830665706728, 0.7145968311855385169, 0.8049029203553225154, 0.9001272540718607829, 1.000000000000000000 ),
 ( 0.000000000000000000, 1.000000000000000000 ),
 .UNSPECIFIED. ) ;
#49007 = CARTESIAN_POINT ( 'NONE',  ( -46.59349553319857762, -24.15543982623906416, -0.2315651400026683127 ) ) ;
#49008 = ORIENTED_EDGE ( 'NONE', *, *, #50805, .T. ) ;
#49009 = CARTESIAN_POINT ( 'NONE',  ( -21.26083644630951142, -3.357327265692296780, 11.49999999999998934 ) ) ;
#49010 = CARTESIAN_POINT ( 'NONE',  ( 6.660000000000001030, -10.15233964170348457, 0.003711184059992174607 ) ) ;
#49011 = CARTESIAN_POINT ( 'NONE',  ( -114.5228709571500474, -24.50216790748205042, 0.6166512839542590552 ) ) ;
#49012 = DIRECTION ( 'NONE',  ( 3.773278334444166432E-23, -1.000000000000000000, 0.000000000000000000 ) ) ;
#49013 = PLANE ( 'NONE',  #53693 ) ;
#49014 = CARTESIAN_POINT ( 'NONE',  ( 7.457602374657920308, -21.66695214233757838, -1.500000000000002220 ) ) ;
#49015 = ADVANCED_FACE ( 'NONE', ( #51972 ), #89528, .T. ) ;
#49016 = VECTOR ( 'NONE', #39490, 1000.000000000000000 ) ;
#49017 = EDGE_CURVE ( 'NONE', #33587, #15382, #48281, .T. ) ;
#49018 = COORDINATED_UNIVERSAL_TIME_OFFSET ( 0, 0, .AHEAD. ) ;
#49019 = CARTESIAN_POINT ( 'NONE',  ( -20.27875734969026311, 7.743225279485574042, 21.75402280011862644 ) ) ;
#49020 = CARTESIAN_POINT ( 'NONE',  ( -53.59318146942742089, -24.15543982623906771, -0.2315651400026670359 ) ) ;
#49021 = CARTESIAN_POINT ( 'NONE',  ( 7.746586651691365510, 18.53313339873204058, 11.49999999999999645 ) ) ;
#49022 = CARTESIAN_POINT ( 'NONE',  ( -109.8914236385200525, -25.28814080510020901, 2.885852232195856182 ) ) ;
#49023 = CARTESIAN_POINT ( 'NONE',  ( -90.52287095715006160, -23.48786465467241769, 11.44779295918254292 ) ) ;
#49024 = PRODUCT_DEFINITION_SHAPE ( 'NONE', 'NONE',  #100425 ) ;
#49025 = FACE_OUTER_BOUND ( 'NONE', #47848, .T. ) ;
#49026 = CARTESIAN_POINT ( 'NONE',  ( -126.5562042904833930, -23.47596703998600631, 11.44779298504227683 ) ) ;
#49027 = CARTESIAN_POINT ( 'NONE',  ( -100.6228709571500701, -23.47596703998600631, 11.44779298504227860 ) ) ;
#49028 = CARTESIAN_POINT ( 'NONE',  ( 18.78741845327603599, -6.401996767227196905, 11.49999999999998934 ) ) ;
#49029 = EDGE_CURVE ( 'NONE', #5079, #1528, #58934, .T. ) ;
#49030 = CARTESIAN_POINT ( 'NONE',  ( -94.52287095715006160, -23.95044443724991723, 10.65354141964649948 ) ) ;
#49031 = CARTESIAN_POINT ( 'NONE',  ( -11.90832679833862073, -15.64659449181510986, -1.500000000000002220 ) ) ;
#49032 = CARTESIAN_POINT ( 'NONE',  ( -85.52287095715004739, -24.99132157543166954, 2.256160258750667502 ) ) ;
#49033 = ADVANCED_FACE ( 'NONE', ( #60093 ), #82901, .T. ) ;
#49034 = EDGE_CURVE ( 'NONE', #1657, #24459, #51473, .T. ) ;
#49035 = DIRECTION ( 'NONE',  ( -0.000000000000000000, -1.000000000000000000, -0.000000000000000000 ) ) ;
#49036 = DATE_TIME_ROLE ( 'classification_date' ) ;
#49037 = CIRCLE ( 'NONE', #45755, 1.000000000000000000 ) ;
#49038 = PLANE ( 'NONE',  #40283 ) ;
#49039 = CARTESIAN_POINT ( 'NONE',  ( -2.704906987277324593, -5.965225279485572685, -28.92935364444904067 ) ) ;
#49040 = CARTESIAN_POINT ( 'NONE',  ( 9.220172233967117492, 18.46515239161685784, 11.49999999999999645 ) ) ;
#49041 = CARTESIAN_POINT ( 'NONE',  ( 4.453188626415028217, -6.376774720514422512, 21.07953283331298167 ) ) ;
#49042 = DIRECTION ( 'NONE',  ( 0.8246584009594636333, 0.5656310827093757876, 0.000000000000000000 ) ) ;
#49043 = CARTESIAN_POINT ( 'NONE',  ( -17.80605238980536953, 13.89162706601689479, 11.49999999999999645 ) ) ;
#49044 = VERTEX_POINT ( 'NONE', #28135 ) ;
#49045 = CARTESIAN_POINT ( 'NONE',  ( -69.35973275182155362, -25.12218989444304995, 6.387116372111183438 ) ) ;
#49046 = LINE ( 'NONE', #78463, #7252 ) ;
#49047 = CARTESIAN_POINT ( 'NONE',  ( -97.58871357123791768, -24.34968618360934300, 0.1864209137778856384 ) ) ;
#49048 = CARTESIAN_POINT ( 'NONE',  ( -39.62287095715005592, -24.64898659630366851, 1.056161002820819261 ) ) ;
#49049 = CARTESIAN_POINT ( 'NONE',  ( -127.5228709571500616, -23.47596703998600631, 11.44779298504227683 ) ) ;
#49050 = CARTESIAN_POINT ( 'NONE',  ( -2.791950601096355733, -6.376774720514417183, 20.17732409774492552 ) ) ;
#49051 = VERTEX_POINT ( 'NONE', #98624 ) ;
#49052 = VECTOR ( 'NONE', #4587, 1000.000000000000114 ) ;
#49053 = CARTESIAN_POINT ( 'NONE',  ( 1.767912858038628965, -23.04938964843747584, 11.49999999999999645 ) ) ;
#49054 = CARTESIAN_POINT ( 'NONE',  ( -10.82450569625279613, 20.10975305113172951, 11.49999999999998934 ) ) ;
#49055 = CARTESIAN_POINT ( 'NONE',  ( -65.05438548721848235, -6.143225279485573509, 29.49402280011861777 ) ) ;
#49056 = CARTESIAN_POINT ( 'NONE',  ( -96.54755524882318696, -24.51314013834316086, 0.6176544820404197278 ) ) ;
#49057 = CARTESIAN_POINT ( 'NONE',  ( -63.55959558400564902, -23.73791477778911840, 11.05961554403170766 ) ) ;
#49058 = LOCAL_TIME ( 0, 54, 15.00000000000000000, #58752 ) ;
#49059 = CARTESIAN_POINT ( 'NONE',  ( 16.80569330386292748, 14.95695114220347932, 11.49999999999999645 ) ) ;
#49060 = EDGE_LOOP ( 'NONE', ( #86245, #11111, #31092, #32097 ) ) ;
#49061 = CARTESIAN_POINT ( 'NONE',  ( -43.55309799638700952, -23.96119346886880308, -0.6495511937831988103 ) ) ;
#49062 = CARTESIAN_POINT ( 'NONE',  ( -3.625624329714521643, -21.66436044012089468, -1.500000000000002220 ) ) ;
#49063 = CARTESIAN_POINT ( 'NONE',  ( -54.62287095715006302, -24.51283580621364777, 0.6167428607019743714 ) ) ;
#49064 = CARTESIAN_POINT ( 'NONE',  ( -44.62370648846312093, -24.66019654487199375, 8.947790411086115725 ) ) ;
#49065 = CARTESIAN_POINT ( 'NONE',  ( -83.62287095715005592, -29.50247984919015209, -1.443849546365053582 ) ) ;
#49066 = VERTEX_POINT ( 'NONE', #4300 ) ;
#49067 = FACE_OUTER_BOUND ( 'NONE', #30412, .T. ) ;
#49068 = CARTESIAN_POINT ( 'NONE',  ( -4.531374827497722357, 4.263680106169587702, -1.700000000000009059 ) ) ;
#49069 = ORIENTED_EDGE ( 'NONE', *, *, #9825, .T. ) ;
#49070 = DIRECTION ( 'NONE',  ( 0.000000000000000000, -1.000000000000000000, 0.000000000000000000 ) ) ;
#49071 = CARTESIAN_POINT ( 'NONE',  ( 15.48611046165106941, -13.43736321338083783, -1.500000000000002220 ) ) ;
#49072 = EDGE_LOOP ( 'NONE', ( #78794, #56443 ) ) ;
#49073 = ORIENTED_EDGE ( 'NONE', *, *, #76159, .F. ) ;
#49075 = ORIENTED_EDGE ( 'NONE', *, *, #90840, .F. ) ;
#49074 = CIRCLE ( 'NONE', #37670, 28.45799999999999486 ) ;
#49076 = B_SPLINE_CURVE_WITH_KNOTS ( 'NONE', 3,
 ( #13083, #20200, #68390, #6488 ),
 .UNSPECIFIED., .F., .F.,
 ( 4, 4 ),
 ( 0.000000000000000000, 9.999999999998897304E-05 ),
 .UNSPECIFIED. ) ;
#49077 = ORIENTED_EDGE ( 'NONE', *, *, #20160, .F. ) ;
#49078 = DIRECTION ( 'NONE',  ( 0.000000000000000000, 0.000000000000000000, 1.000000000000000000 ) ) ;
#49079 = CARTESIAN_POINT ( 'NONE',  ( 10.19088217375349892, 20.72639945755932800, 11.49999999999998934 ) ) ;
#49080 = CARTESIAN_POINT ( 'NONE',  ( -41.52287095715006870, -23.48786465467240347, 11.44779295918255180 ) ) ;
#49081 = CARTESIAN_POINT ( 'NONE',  ( -17.59887021274124663, -10.25344800880639262, -1.500000000000002220 ) ) ;
#49082 = ORIENTED_EDGE ( 'NONE', *, *, #88194, .T. ) ;
#49083 = FACE_OUTER_BOUND ( 'NONE', #3753, .T. ) ;
#49084 = DIRECTION ( 'NONE',  ( 0.000000000000000000, -1.000000000000000000, 0.000000000000000000 ) ) ;
#49085 = FACE_OUTER_BOUND ( 'NONE', #16873, .T. ) ;
#49086 = CARTESIAN_POINT ( 'NONE',  ( 32.98733314340959311, 5.965225279485572685, 2.074222136288530027 ) ) ;
#49087 = ORIENTED_EDGE ( 'NONE', *, *, #69523, .T. ) ;
#49088 = PLANE ( 'NONE',  #66312 ) ;
#49089 = CARTESIAN_POINT ( 'NONE',  ( -49.10457154551148307, -25.26385639663606497, 3.999772272082692037 ) ) ;
#49090 = ORIENTED_EDGE ( 'NONE', *, *, #74985, .T. ) ;
#49091 = CARTESIAN_POINT ( 'NONE',  ( -20.31193019649481357, 4.361987795224258946, 11.49999999999998934 ) ) ;
#49092 = ORIENTED_EDGE ( 'NONE', *, *, #71219, .T. ) ;
#49094 = ORIENTED_EDGE ( 'NONE', *, *, #20786, .T. ) ;
#49093 = DIRECTION ( 'NONE',  ( 0.000000000000000000, 1.000000000000000000, -0.000000000000000000 ) ) ;
#49095 = AXIS2_PLACEMENT_3D ( 'NONE', #27410, #3582, #91166 ) ;
#49096 = B_SPLINE_CURVE_WITH_KNOTS ( 'NONE', 3,
 ( #21707, #6505, #14102, #7001 ),
 .UNSPECIFIED., .F., .F.,
 ( 4, 4 ),
 ( 0.000000000000000000, 9.999999999998897304E-05 ),
 .UNSPECIFIED. ) ;
#49097 = EDGE_CURVE ( 'NONE', #4416, #61038, #28861, .T. ) ;
#49098 = B_SPLINE_SURFACE_WITH_KNOTS ( 'NONE', 3, 3, ( 
 ( #76811, #6816, #23020, #32150 ),
 ( #15423, #84938, #8319, #23522 ),
 ( #61125, #46382, #47390, #61629 ),
 ( #53518, #92549, #77316, #30151 ),
 ( #54499, #7817, #31152, #92054 ),
 ( #70223, #14921, #93043, #45894 ),
 ( #62121, #15921, #703, #7310 ) ),
 .UNSPECIFIED., .F., .F., .F.,
 ( 4, 3, 4 ),
 ( 4, 4 ),
 ( 0.7945040050992242531, 0.8970133687736498995, 0.9995227324480754350 ),
 ( 0.08951674469141676638, 0.09057079611598997659 ),
 .UNSPECIFIED. ) ;
#49099 = DIRECTION ( 'NONE',  ( -1.000000000000000000, 0.000000000000000000, 0.000000000000000000 ) ) ;
#49100 = FACE_OUTER_BOUND ( 'NONE', #11071, .T. ) ;
#49101 = ORIENTED_EDGE ( 'NONE', *, *, #89045, .T. ) ;
#49102 = ORIENTED_EDGE ( 'NONE', *, *, #45364, .F. ) ;
#49103 = CARTESIAN_POINT ( 'NONE',  ( 31.93426202889373400, 6.376774720514426953, 6.907000118922836940 ) ) ;
#49104 = CARTESIAN_POINT ( 'NONE',  ( -58.62287095715004881, -23.47593901973091235, -1.443836447539007972 ) ) ;
#49105 = CARTESIAN_POINT ( 'NONE',  ( -28.16513019978995302, -24.66613713371811656, 1.682082916390950533 ) ) ;
#49107 = ORIENTED_EDGE ( 'NONE', *, *, #25034, .T. ) ;
#49106 = CARTESIAN_POINT ( 'NONE',  ( -21.12782282263547984, 6.412464199276892707, 11.49999999999999645 ) ) ;
#49108 = CARTESIAN_POINT ( 'NONE',  ( -103.6250747051918353, -24.51314013834315375, 0.6176544820404142877 ) ) ;
#49109 = VECTOR ( 'NONE', #13493, 1000.000000000000000 ) ;
#49110 = CARTESIAN_POINT ( 'NONE',  ( -22.20892344277460850, -4.061126821146308963, -1.500000000000002220 ) ) ;
#49111 = ADVANCED_FACE ( 'NONE', ( #5286 ), #34747, .T. ) ;
#49112 = EDGE_CURVE ( 'NONE', #62582, #16286, #96634, .T. ) ;
#49113 = EDGE_CURVE ( 'NONE', #86042, #11910, #9443, .T. ) ;
#49115 = ORIENTED_EDGE ( 'NONE', *, *, #59093, .T. ) ;
#49114 = CARTESIAN_POINT ( 'NONE',  ( -90.52287095715006160, -23.47593901973090524, -1.443836447538996426 ) ) ;
#49116 = VECTOR ( 'NONE', #76685, 1000.000000000000000 ) ;
#49117 = EDGE_LOOP ( 'NONE', ( #63396, #5016, #21800, #65444 ) ) ;
#49118 = EDGE_CURVE ( 'NONE', #5913, #76909, #43431, .T. ) ;
#49119 = DIRECTION ( 'NONE',  ( -3.773278334444167608E-23, 1.000000000000000000, 0.000000000000000000 ) ) ;
#49120 = CARTESIAN_POINT ( 'NONE',  ( 9.478389368232452483, -2.682774720514426559, -23.17485683983816003 ) ) ;
#49121 = ORIENTED_EDGE ( 'NONE', *, *, #41109, .T. ) ;
#49122 = CARTESIAN_POINT ( 'NONE',  ( 3.105769797727405024, 20.95935918496786599, 11.49999999999998934 ) ) ;
#49123 = CARTESIAN_POINT ( 'NONE',  ( -128.6228709571500417, -29.50248528299804818, 1.056150453629047137 ) ) ;
#49124 = CARTESIAN_POINT ( 'NONE',  ( 29.72852606603716552, -4.950008708102185295, 27.41398129243886217 ) ) ;
#49125 = SPHERICAL_SURFACE ( 'NONE', #75113, 6.600000000000001421 ) ;
#49126 = CARTESIAN_POINT ( 'NONE',  ( -105.6228709571500275, -25.00182538069145721, 7.747789668545099317 ) ) ;
#49127 = CARTESIAN_POINT ( 'NONE',  ( 21.60277357391871433, -5.133695162202882578, -1.500000000000002220 ) ) ;
#49128 = FACE_OUTER_BOUND ( 'NONE', #24420, .T. ) ;
#49129 = ADVANCED_FACE ( 'NONE', ( #31611 ), #69179, .T. ) ;
#49130 = VERTEX_POINT ( 'NONE', #6282 ) ;
#49131 = CARTESIAN_POINT ( 'NONE',  ( -5.486124437288584232, -6.376774720514417183, 19.74568812963598319 ) ) ;
#49132 = CARTESIAN_POINT ( 'NONE',  ( -50.58953762381672448, -23.47596703998600276, 11.44779298504227505 ) ) ;
#49133 = CARTESIAN_POINT ( 'NONE',  ( -4.539579955115475407, -18.87035741768621122, 11.49999999999999645 ) ) ;
#49134 = DIRECTION ( 'NONE',  ( 3.773278334444166432E-23, -1.000000000000000000, 0.000000000000000000 ) ) ;
#49135 = CARTESIAN_POINT ( 'NONE',  ( -31.52287095715006160, -24.64898659630367206, 1.056161002820817485 ) ) ;
#49136 = VECTOR ( 'NONE', #5086, 1000.000000000000000 ) ;
#49137 = EDGE_CURVE ( 'NONE', #34853, #54541, #39222, .T. ) ;
#49138 = CARTESIAN_POINT ( 'NONE',  ( 18.23270504744370868, -6.907985942191454676, -1.500000000000002220 ) ) ;
#49139 = CC_DESIGN_APPROVAL ( #78479, ( #83064 ) ) ;
#49140 = CARTESIAN_POINT ( 'NONE',  ( 6.977786103627443559, 20.27319509581574408, 11.49999999999998934 ) ) ;
#49141 = CARTESIAN_POINT ( 'NONE',  ( 9.616086099857337643, -1.335655600570672119, 18.31352460785937097 ) ) ;
#49142 = CARTESIAN_POINT ( 'NONE',  ( -60.62578132507420037, -24.92592662360294042, 8.075495902990192931 ) ) ;
#49143 = CYLINDRICAL_SURFACE ( 'NONE', #63270, 91.74549126261078413 ) ;
#49144 = CARTESIAN_POINT ( 'NONE',  ( -74.62287095715005592, -29.50248528299804818, 1.056150453629036701 ) ) ;
#49145 = CARTESIAN_POINT ( 'NONE',  ( -4.508144621425604903, 22.28865971958312997, -1.500000000000002220 ) ) ;
#49146 = EDGE_CURVE ( 'NONE', #2242, #78619, #47576, .T. ) ;
#49147 = AXIS2_PLACEMENT_3D ( 'NONE', #95666, #18532, #88556 ) ;
#49148 = DIRECTION ( 'NONE',  ( 0.000000000000000000, -1.000000000000000000, 0.000000000000000000 ) ) ;
#49149 = DIRECTION ( 'NONE',  ( 1.000000000000000000, 0.000000000000000000, 0.000000000000000000 ) ) ;
#49150 = DIRECTION ( 'NONE',  ( -0.000000000000000000, 1.000000000000000000, -0.000000000000000000 ) ) ;
#49151 = CARTESIAN_POINT ( 'NONE',  ( -18.79874323561663729, 6.599581278811135654, 11.49999999999999645 ) ) ;
#49152 = CARTESIAN_POINT ( 'NONE',  ( -101.6228709571501128, -24.35013146730204525, 9.818937971375103047 ) ) ;
#49153 = AXIS2_PLACEMENT_3D ( 'NONE', #91278, #36488, #21749 ) ;
#49154 = CARTESIAN_POINT ( 'NONE',  ( -39.64842002074407645, -23.96169478059713143, 10.65365249895718769 ) ) ;
#49155 = CARTESIAN_POINT ( 'NONE',  ( 8.971512145086503409, -1.028487854913504362, -3.750000000000000000 ) ) ;
#49156 = VERTEX_POINT ( 'NONE', #52469 ) ;
#49157 = CARTESIAN_POINT ( 'NONE',  ( -120.6228709571500701, -25.00158670708909625, 2.256160236439166411 ) ) ;
#49158 = DIRECTION ( 'NONE',  ( -0.000000000000000000, 1.000000000000000000, -1.155373159085149695E-17 ) ) ;
#49159 = CARTESIAN_POINT ( 'NONE',  ( -7.614213781628100364, -20.28429660096114517, -1.500000000000002220 ) ) ;
#49160 = DIRECTION ( 'NONE',  ( -1.000000000000000000, -3.773278334444167608E-23, -8.201307833595939069E-29 ) ) ;
#49161 = CARTESIAN_POINT ( 'NONE',  ( 14.32981562401322506, -13.22600733894156200, -1.500000000000002220 ) ) ;
#49162 = CARTESIAN_POINT ( 'NONE',  ( -60.62287095715004881, -24.99132157543084531, 2.256160258750667502 ) ) ;
#49163 = EDGE_CURVE ( 'NONE', #40340, #89470, #82053, .T. ) ;
#49164 = ORIENTED_EDGE ( 'NONE', *, *, #50242, .F. ) ;
#49165 = CARTESIAN_POINT ( 'NONE',  ( -69.62287095715005592, -24.64965695001468404, 8.947790433994184056 ) ) ;
#49166 = CARTESIAN_POINT ( 'NONE',  ( -14.48729221511043441, 14.40292172154154926, 11.49999999999999645 ) ) ;
#49167 = DIRECTION ( 'NONE',  ( -9.524068072025174096E-40, -2.173523156925980399E-06, 0.9999999999976378895 ) ) ;
#49168 = EDGE_CURVE ( 'NONE', #78009, #95252, #76281, .T. ) ;
#49169 = CARTESIAN_POINT ( 'NONE',  ( -0.02075734969026423599, 0.3587747205144213303, -0.08597719988137648983 ) ) ;
#49170 = ORIENTED_EDGE ( 'NONE', *, *, #24017, .T. ) ;
#49171 = CARTESIAN_POINT ( 'NONE',  ( -74.62287095715005592, -23.48783264082478794, -1.443836473390067265 ) ) ;
#49172 = CARTESIAN_POINT ( 'NONE',  ( 33.00535138976576377, 3.570691370340801640, -12.97242311383999791 ) ) ;
#49173 = CARTESIAN_POINT ( 'NONE',  ( -113.9228709571500957, -23.47593901973090880, -1.443836447538996870 ) ) ;
#49174 = FACE_OUTER_BOUND ( 'NONE', #24704, .T. ) ;
#49175 = B_SPLINE_CURVE_WITH_KNOTS ( 'NONE', 3,
 ( #45793, #84340, #14824, #6223 ),
 .UNSPECIFIED., .F., .F.,
 ( 4, 4 ),
 ( 0.000000000000000000, 9.999999999998897304E-05 ),
 .UNSPECIFIED. ) ;
#49176 = FACE_OUTER_BOUND ( 'NONE', #68474, .T. ) ;
#49177 = CARTESIAN_POINT ( 'NONE',  ( -29.49875734969025842, 5.965225279485572685, 23.37402280011862743 ) ) ;
#49178 = VECTOR ( 'NONE', #74540, 1000.000000000000000 ) ;
#49179 = ORIENTED_EDGE ( 'NONE', *, *, #4303, .F. ) ;
#49180 = CARTESIAN_POINT ( 'NONE',  ( -82.52287095715006160, -23.47593901973090169, -1.443836447538996648 ) ) ;
#49181 = CARTESIAN_POINT ( 'NONE',  ( 22.95104020007722667, -0.4190376320207603866, 11.49999999999999645 ) ) ;
#49182 = CARTESIAN_POINT ( 'NONE',  ( 10.97283692364161922, -19.94330716608196852, -1.500000000000002220 ) ) ;
#49183 = CARTESIAN_POINT ( 'NONE',  ( -110.5864147487693288, -24.92592662359561828, 8.075495903018000021 ) ) ;
#49184 = VECTOR ( 'NONE', #25426, 1000.000000000000114 ) ;
#49185 = CARTESIAN_POINT ( 'NONE',  ( 33.00535138976592719, 3.570691370340881576, -12.97242311383975988 ) ) ;
#49186 = CARTESIAN_POINT ( 'NONE',  ( -90.63674641968886192, -24.15503026093915651, -0.2815557561904460382 ) ) ;
#49187 = DIRECTION ( 'NONE',  ( -1.000000000000000000, 0.000000000000000000, 0.000000000000000000 ) ) ;
#49188 = CARTESIAN_POINT ( 'NONE',  ( -89.52287095715007581, -23.73907113217668297, -1.053371485781303907 ) ) ;
#49189 = CARTESIAN_POINT ( 'NONE',  ( -13.92312151449838531, -16.86485062357919773, 11.49999999999998934 ) ) ;
#49190 = DIRECTION ( 'NONE',  ( -3.773278334453080206E-23, 0.9999999999976377785, 2.173523156925979975E-06 ) ) ;
#49191 = CARTESIAN_POINT ( 'NONE',  ( -115.6228709571500417, -23.48783264082478794, -1.443836473390058384 ) ) ;
#49192 = CARTESIAN_POINT ( 'NONE',  ( 6.573941812937369455, -7.905506363763796338E-18, 0.2639660507643297183 ) ) ;
#49193 = CARTESIAN_POINT ( 'NONE',  ( -58.50879486179008637, -23.96119346886881019, -0.6495511937832116889 ) ) ;
#49194 = VERTEX_POINT ( 'NONE', #53475 ) ;
#49195 = CARTESIAN_POINT ( 'NONE',  ( -18.43012528856881715, -8.789534013050598560, 11.49999999999998934 ) ) ;
#49196 = ORIENTED_EDGE ( 'NONE', *, *, #33752, .F. ) ;
#49197 = EDGE_LOOP ( 'NONE', ( #14460, #84384 ) ) ;
#49198 = CARTESIAN_POINT ( 'NONE',  ( -6.685540227124203483, -22.02754839873749404, 11.49999999999998934 ) ) ;
#49199 = CARTESIAN_POINT ( 'NONE',  ( -6.720452724358975338, -5.876774720514411854, 19.46153846153846700 ) ) ;
#49200 = ORIENTED_EDGE ( 'NONE', *, *, #3009, .F. ) ;
#49201 = CARTESIAN_POINT ( 'NONE',  ( -109.8650237084402619, -25.29042187987247914, 5.784623108531866897 ) ) ;
#49202 = CARTESIAN_POINT ( 'NONE',  ( -76.62287095715007013, -24.64965695001468404, 8.947790433994182280 ) ) ;
#49203 = VECTOR ( 'NONE', #58972, 1000.000000000000114 ) ;
#49204 = CARTESIAN_POINT ( 'NONE',  ( -98.62287095715009855, -24.51387760970724372, 9.387446482453414731 ) ) ;
#49205 = CARTESIAN_POINT ( 'NONE',  ( -96.62287095715005592, -24.50216790748097750, 0.6166512839513716981 ) ) ;
#49207 = ORIENTED_EDGE ( 'NONE', *, *, #93416, .F. ) ;
#49206 = CARTESIAN_POINT ( 'NONE',  ( 2.936642053869352953, -21.15864249054145674, 11.49999999999999645 ) ) ;
#49208 = EDGE_LOOP ( 'NONE', ( #90898, #32464, #42091, #12846 ) ) ;
#49209 = CARTESIAN_POINT ( 'NONE',  ( -19.85906585229243504, 9.992431322412627992, -1.500000000000002220 ) ) ;
#49210 = CARTESIAN_POINT ( 'NONE',  ( 7.914317726235799100, 19.11507755054979896, 11.49999999999998934 ) ) ;
#49212 = ORIENTED_EDGE ( 'NONE', *, *, #12403, .F. ) ;
#49211 = CIRCLE ( 'NONE', #92853, 28.96799999999999287 ) ;
#49213 = CARTESIAN_POINT ( 'NONE',  ( -6.369015873774380943, -6.376774720514413630, 19.23384392940399934 ) ) ;
#49214 = CARTESIAN_POINT ( 'NONE',  ( -41.62287095715006302, -29.50247984919015209, -1.443849546365060466 ) ) ;
#49215 = EDGE_LOOP ( 'NONE', ( #38075, #18027, #89352, #72600 ) ) ;
#49216 = EDGE_CURVE ( 'NONE', #45568, #79343, #45850, .T. ) ;
#49217 = LINE ( 'NONE', #86752, #94777 ) ;
#49218 = VERTEX_POINT ( 'NONE', #84403 ) ;
#49219 = AXIS2_PLACEMENT_3D ( 'NONE', #85803, #63490, #1069 ) ;
#49221 = EDGE_CURVE ( 'NONE', #9489, #43107, #46849, .T. ) ;
#49220 = CARTESIAN_POINT ( 'NONE',  ( 13.80377080874918150, 6.475225279485574248, -27.21172484903264532 ) ) ;
#49222 = CARTESIAN_POINT ( 'NONE',  ( 8.587038044527741221, -19.06309208085484386, -1.500000000000002220 ) ) ;
#49223 = CARTESIAN_POINT ( 'NONE',  ( -11.18773875818744656, -18.78983145652188469, 11.49999999999999645 ) ) ;
#49224 = EDGE_CURVE ( 'NONE', #70309, #46658, #2273, .T. ) ;
#49225 = CARTESIAN_POINT ( 'NONE',  ( -68.62287095715005592, -29.50248528299804818, 1.056150453629036701 ) ) ;
#49226 = CARTESIAN_POINT ( 'NONE',  ( 5.092794675178905273, -3.306008726340172288, -27.56219045528442280 ) ) ;
#49227 = CARTESIAN_POINT ( 'NONE',  ( 22.48772827135616126, 0.8316936486096353498, -1.500000000000002220 ) ) ;
#49228 = EDGE_CURVE ( 'NONE', #49448, #67210, #77768, .T. ) ;
#49229 = CARTESIAN_POINT ( 'NONE',  ( -3.950822543831816080, -20.53616823614468956, -1.500000000000002220 ) ) ;
#49230 = CARTESIAN_POINT ( 'NONE',  ( -38.63478458652770087, -24.34968618360933235, 0.1864209137778849723 ) ) ;
#49231 = CARTESIAN_POINT ( 'NONE',  ( -8.499999999999987566, 18.74999999999999645, 0.000000000000000000 ) ) ;
#49232 = CARTESIAN_POINT ( 'NONE',  ( 10.54059822343757702, -5.876774720514426953, 17.17691942396159988 ) ) ;
#49233 = ORIENTED_EDGE ( 'NONE', *, *, #63206, .T. ) ;
#49234 = ORIENTED_EDGE ( 'NONE', *, *, #23545, .F. ) ;
#49235 = VERTEX_POINT ( 'NONE', #60595 ) ;
#49236 = CARTESIAN_POINT ( 'NONE',  ( -52.54159836110628135, -24.34968618360933945, 0.1864209137778880532 ) ) ;
#49237 = ORIENTED_EDGE ( 'NONE', *, *, #27357, .F. ) ;
#49238 = CARTESIAN_POINT ( 'NONE',  ( -21.38522110535750542, 1.317000383210971792, -1.500000000000002220 ) ) ;
#49239 = ADVANCED_FACE ( 'NONE', ( #70179 ), #664, .F. ) ;
#49240 = CARTESIAN_POINT ( 'NONE',  ( 21.86734719908870872, 4.625976558377421277, 11.49999999999999645 ) ) ;
#49241 = ORIENTED_EDGE ( 'NONE', *, *, #89712, .T. ) ;
#49242 = DIRECTION ( 'NONE',  ( 0.000000000000000000, 0.000000000000000000, 1.000000000000000000 ) ) ;
#49243 = CARTESIAN_POINT ( 'NONE',  ( 2.841100885065937387, 20.89556961663114265, -1.500000000000002220 ) ) ;
#49244 = CARTESIAN_POINT ( 'NONE',  ( -30.40788173565302088, -25.13746717394300845, 7.291421475381016926 ) ) ;
#49245 = CARTESIAN_POINT ( 'NONE',  ( 3.323502641304225236, -6.376774720514426065, 21.72931788002195219 ) ) ;
#49246 = APPLICATION_CONTEXT ( 'configuration controlled 3d designs of mechanical parts and assemblies' ) ;
#49247 = CARTESIAN_POINT ( 'NONE',  ( 8.160000000000000142, -10.15233964170348457, -1.303165529866009420 ) ) ;
#49248 = CARTESIAN_POINT ( 'NONE',  ( -101.5471480383779408, -24.65952944569305316, 1.056160979905706121 ) ) ;
#49249 = CARTESIAN_POINT ( 'NONE',  ( 21.54648482299927181, -4.703075207800759827, -1.500000000000002220 ) ) ;
#49250 = EDGE_LOOP ( 'NONE', ( #9368, #44379, #21086, #43825 ) ) ;
#49251 = CARTESIAN_POINT ( 'NONE',  ( -65.55949235626067662, -23.85049219812685806, 10.88485053497527311 ) ) ;
#49252 = AXIS2_PLACEMENT_3D ( 'NONE', #52410, #50920, #81860 ) ;
#49253 = CARTESIAN_POINT ( 'NONE',  ( -111.6228709571500417, -24.66019654487199730, 8.947790411086124607 ) ) ;
#49254 = CARTESIAN_POINT ( 'NONE',  ( -60.52842363010253735, -25.00158670708910336, 2.256160236439220590 ) ) ;
#49255 = CARTESIAN_POINT ( 'NONE',  ( -62.57945178327253899, -24.66019654487199730, 8.947790411086124607 ) ) ;
#49256 = B_SPLINE_CURVE_WITH_KNOTS ( 'NONE', 3,
 ( #83361, #68651, #5744, #13847 ),
 .UNSPECIFIED., .F., .F.,
 ( 4, 4 ),
 ( 0.000000000000000000, 9.999999999998898659E-05 ),
 .UNSPECIFIED. ) ;
#49257 = CIRCLE ( 'NONE', #52495, 2.000000000000000000 ) ;
#49258 = CARTESIAN_POINT ( 'NONE',  ( -25.53098197642538736, -24.91566218739149363, 4.942811707542018596 ) ) ;
#49259 = CARTESIAN_POINT ( 'NONE',  ( -117.5228709571500758, -24.34917612406837151, 0.1852690917426621509 ) ) ;
#49260 = CARTESIAN_POINT ( 'NONE',  ( -14.61619677566029729, 15.53698580111986693, 11.49999999999998934 ) ) ;
#49261 = CARTESIAN_POINT ( 'NONE',  ( -92.22287095715003602, -23.47596703998600631, 11.44779298504227683 ) ) ;
#49262 = CARTESIAN_POINT ( 'NONE',  ( 5.471383689419962337, 5.965225279485594001, -29.02273493113403902 ) ) ;
#49263 = DIRECTION ( 'NONE',  ( -3.773278334453079618E-23, 0.9999999999976377785, 2.173523156925979975E-06 ) ) ;
#49264 = CARTESIAN_POINT ( 'NONE',  ( 24.71017632900191074, 3.356774720514427379, 1.647607965253217621 ) ) ;
#49265 = CARTESIAN_POINT ( 'NONE',  ( 6.619388286264371146, -21.57091762011834390, -1.500000000000002220 ) ) ;
#49266 = B_SPLINE_CURVE_WITH_KNOTS ( 'NONE', 3,
 ( #13576, #39427, #39925, #16078, #68873, #86597, #78977, #54170, #24687, #54661, #15083, #48047, #53665, #46050, #93201, #8972, #70377, #23687, #85092, #93702, #24193, #47550, #46541 ),
 .UNSPECIFIED., .F., .F.,
 ( 4, 1, 1, 1, 1, 1, 1, 1, 1, 1, 1, 1, 1, 1, 1, 1, 1, 1, 1, 1, 4 ),
 ( 0.000000000000000000, 0.06038661931106227565, 0.1208832485859964029, 0.1827546186251403082, 0.2478110297583512034, 0.2812991000432494282, 0.3150876241506579412, 0.3497023955502757131, 0.3848565811185565289, 0.4209661972261032892, 0.4585111882611391243, 0.4971747221273126183, 0.5376020478662695279, 0.5805030184200120624, 0.6274675400267057945, 0.6783882095592440598, 0.7339832205925608255, 0.7937467045508355135, 0.8577136721607333536, 0.9266978643613864586, 1.000000000000000000 ),
 .UNSPECIFIED. ) ;
#49267 = FACE_OUTER_BOUND ( 'NONE', #59866, .T. ) ;
#49268 = ORIENTED_EDGE ( 'NONE', *, *, #80585, .T. ) ;
#49269 = LINE ( 'NONE', #95419, #95192 ) ;
#49270 = CARTESIAN_POINT ( 'NONE',  ( 2.909586618535765723, -5.876774720514411854, 19.75512108203924200 ) ) ;
#49271 = CARTESIAN_POINT ( 'NONE',  ( -0.6023826358649750912, 19.72334862104828090, 11.49999999999999645 ) ) ;
#49272 = CARTESIAN_POINT ( 'NONE',  ( -66.62287095715005592, -29.50250786944525672, 11.44777988621623699 ) ) ;
#49273 = CARTESIAN_POINT ( 'NONE',  ( 282.9764569301858046, -2.682774720514426559, 20.79159422840526616 ) ) ;
#49274 = ORIENTED_EDGE ( 'NONE', *, *, #62145, .T. ) ;
#49275 = CARTESIAN_POINT ( 'NONE',  ( 30.09341516180546350, 1.682774720514426114, -11.39311774897855756 ) ) ;
#49276 = DIRECTION ( 'NONE',  ( -6.924038193813838377E-14, 0.000000000000000000, -1.000000000000000000 ) ) ;
#49277 = DIRECTION ( 'NONE',  ( -2.501730345825856179E-15, 6.879758451021104590E-15, -1.000000000000000000 ) ) ;
#49278 = CARTESIAN_POINT ( 'NONE',  ( -126.6228709571501128, -24.50321055353807509, 9.387540953477524042 ) ) ;
#49279 = DIRECTION ( 'NONE',  ( -0.000000000000000000, 0.000000000000000000, -1.000000000000000000 ) ) ;
#49280 = DIRECTION ( 'NONE',  ( 0.000000000000000000, -0.9999999999976377785, -2.173523156925979128E-06 ) ) ;
#49281 = CARTESIAN_POINT ( 'NONE',  ( -74.52287095715007581, -23.47593901973090169, -1.443836447538996870 ) ) ;
#49282 = EDGE_CURVE ( 'NONE', #38251, #86491, #14383, .T. ) ;
#49283 = CARTESIAN_POINT ( 'NONE',  ( -19.76903914530799966, 0.2396048511829373395, -1.500000000000002220 ) ) ;
#49284 = ORIENTED_EDGE ( 'NONE', *, *, #6681, .F. ) ;
#49285 = CARTESIAN_POINT ( 'NONE',  ( -6.636546740042271963, -19.09123619949631134, 11.49999999999999645 ) ) ;
#49286 = CARTESIAN_POINT ( 'NONE',  ( 6.351517594976544778, -5.876774720514417183, 20.09206396488320578 ) ) ;
#49287 = ADVANCED_FACE ( 'NONE', ( #15380 ), #601, .T. ) ;
#49288 = ORIENTED_EDGE ( 'NONE', *, *, #35756, .F. ) ;
#49289 = CARTESIAN_POINT ( 'NONE',  ( 22.33191539159863481, -4.132774720514426292, -16.26852658953813346 ) ) ;
#49290 = CARTESIAN_POINT ( 'NONE',  ( -41.55620429048338593, -23.47596703998600276, 11.44779298504227505 ) ) ;
#49291 = DIRECTION ( 'NONE',  ( 0.000000000000000000, 0.000000000000000000, 1.000000000000000000 ) ) ;
#49292 = CARTESIAN_POINT ( 'NONE',  ( -122.5228709571500616, -23.47596703998600631, 11.44779298504227860 ) ) ;
#49293 = CARTESIAN_POINT ( 'NONE',  ( -103.6228709571500417, -23.47596703998600631, 11.44779298504227860 ) ) ;
#49294 = CARTESIAN_POINT ( 'NONE',  ( -81.52287095715006160, -24.65952944569304606, 1.056160979905698794 ) ) ;
#49295 = CARTESIAN_POINT ( 'NONE',  ( 17.67427751897593069, 9.450557017276361549, -1.500000000000002220 ) ) ;
#49296 = DIRECTION ( 'NONE',  ( 1.000000000000000000, -0.000000000000000000, -0.000000000000000000 ) ) ;
#49297 = EDGE_LOOP ( 'NONE', ( #54544, #61221, #32518, #97745 ) ) ;
#49298 = CARTESIAN_POINT ( 'NONE',  ( -51.52287095715006870, -23.96127896941631619, -0.6493128931038041340 ) ) ;
#49299 = CARTESIAN_POINT ( 'NONE',  ( -35.62991159852106904, -24.83618233451448987, 1.606449574219547261 ) ) ;
#49300 = LINE ( 'NONE', #17835, #58146 ) ;
#49301 = CARTESIAN_POINT ( 'NONE',  ( 2.230654205607476737, -2.168404344971008868E-16, 0.1647943925233645579 ) ) ;
#49302 = CARTESIAN_POINT ( 'NONE',  ( -101.7587712593593636, -25.25648092924479826, 3.908092476104340296 ) ) ;
#49303 = VECTOR ( 'NONE', #11208, 1000.000000000000000 ) ;
#49304 = DIRECTION ( 'NONE',  ( -0.09824042138329590335, 4.470611911092166224E-17, -0.9951627101165078093 ) ) ;
#49305 = FACE_OUTER_BOUND ( 'NONE', #43697, .T. ) ;
#49306 = ORIENTED_EDGE ( 'NONE', *, *, #30509, .T. ) ;
#49307 = CARTESIAN_POINT ( 'NONE',  ( -20.26613141553852060, -1.498020344548873561, -1.500000000000002220 ) ) ;
#49308 = VERTEX_POINT ( 'NONE', #70681 ) ;
#49309 = CARTESIAN_POINT ( 'NONE',  ( -32.51246533390832383, -23.73766607897670866, -1.055555164236441801 ) ) ;
#49310 = VECTOR ( 'NONE', #29062, 1000.000000000000114 ) ;
#49311 = CARTESIAN_POINT ( 'NONE',  ( -127.5550739197475139, -24.66019654487200441, 8.947790411086106843 ) ) ;
#49312 = ORIENTED_EDGE ( 'NONE', *, *, #60215, .T. ) ;
#49313 = FACE_OUTER_BOUND ( 'NONE', #14599, .T. ) ;
#49314 = B_SPLINE_CURVE_WITH_KNOTS ( 'NONE', 3,
 ( #16813, #92430, #47778, #31534 ),
 .UNSPECIFIED., .F., .F.,
 ( 4, 4 ),
 ( 0.2799858555236601210, 0.2889922867957759878 ),
 .UNSPECIFIED. ) ;
#49315 = CARTESIAN_POINT ( 'NONE',  ( -49.35312698006249832, -25.12215289943983265, 6.504948950085263526 ) ) ;
#49317 = DIRECTION ( 'NONE',  ( 1.000000000000000000, 3.773278334444167608E-23, 8.201307833595939069E-29 ) ) ;
#49316 = VECTOR ( 'NONE', #17857, 1000.000000000000000 ) ;
#49318 = CARTESIAN_POINT ( 'NONE',  ( 10.98566517548414012, -18.08203305749968592, 11.49999999999999645 ) ) ;
#49319 = CARTESIAN_POINT ( 'NONE',  ( 19.07224962250127831, -11.27678277851665634, 11.49999999999998934 ) ) ;
#49320 = CARTESIAN_POINT ( 'NONE',  ( 13.18781518674367348, -15.76626393773247337, 11.49999999999998934 ) ) ;
#49321 = ORIENTED_EDGE ( 'NONE', *, *, #11213, .F. ) ;
#49322 = CARTESIAN_POINT ( 'NONE',  ( -91.58953762381672448, -23.47596703998600631, 11.44779298504227683 ) ) ;
#49323 = ORIENTED_EDGE ( 'NONE', *, *, #84767, .F. ) ;
#49324 = CARTESIAN_POINT ( 'NONE',  ( -4.568292318365942073, -0.3587747205144265483, 30.06720597538392425 ) ) ;
#49325 = CARTESIAN_POINT ( 'NONE',  ( -58.52287095715006160, -29.50250786944525672, 11.44777988621623876 ) ) ;
#49326 = ORIENTED_EDGE ( 'NONE', *, *, #35493, .F. ) ;
#49328 = ORIENTED_EDGE ( 'NONE', *, *, #57819, .T. ) ;
#49327 = EDGE_CURVE ( 'NONE', #42928, #5789, #72195, .T. ) ;
#49329 = ORIENTED_EDGE ( 'NONE', *, *, #47363, .T. ) ;
#49330 = CARTESIAN_POINT ( 'NONE',  ( -112.6228709571501554, -24.34917612406838572, 0.1852690917426693118 ) ) ;
#49331 = CARTESIAN_POINT ( 'NONE',  ( 7.166666666666668739, -6.376774720514420736, 20.78665865384614975 ) ) ;
#49332 = CARTESIAN_POINT ( 'NONE',  ( -91.62287095715005592, -24.51283580621363711, 0.6167428607019886933 ) ) ;
#49333 = CARTESIAN_POINT ( 'NONE',  ( -16.33875328525262560, 12.67428768300982256, -1.500000000000002220 ) ) ;
#49334 = CARTESIAN_POINT ( 'NONE',  ( -18.79206335510377102, -10.79472360063173397, 11.49999999999999645 ) ) ;
#49335 = EDGE_LOOP ( 'NONE', ( #32436, #40490, #10226, #30516 ) ) ;
#49336 = EDGE_CURVE ( 'NONE', #97163, #52247, #85904, .T. ) ;
#49337 = PLANE ( 'NONE',  #1260 ) ;
#49338 = CARTESIAN_POINT ( 'NONE',  ( 2.610950917001260141, -5.876774720514411854, 19.54489930512155027 ) ) ;
#49339 = CARTESIAN_POINT ( 'NONE',  ( 15.70178742502441693, -15.98865493379879332, -1.500000000000002220 ) ) ;
#49340 = EDGE_CURVE ( 'NONE', #451, #3529, #36187, .T. ) ;
#49341 = PLANE ( 'NONE',  #72505 ) ;
#49342 = CARTESIAN_POINT ( 'NONE',  ( -10.79305683637731406, 5.965225279485594001, -27.49869550653260930 ) ) ;
#49343 = ORIENTED_EDGE ( 'NONE', *, *, #10265, .F. ) ;
#49344 = CARTESIAN_POINT ( 'NONE',  ( -29.49875734969026198, -5.965225279485572685, 10.11402280011862587 ) ) ;
#49345 = PLANE ( 'NONE',  #60473 ) ;
#49346 = ADVANCED_FACE ( 'NONE', ( #72693 ), #9779, .T. ) ;
#49347 = ORIENTED_EDGE ( 'NONE', *, *, #35907, .F. ) ;
#49348 = EDGE_CURVE ( 'NONE', #47587, #75526, #24997, .T. ) ;
#49349 = ORIENTED_EDGE ( 'NONE', *, *, #84088, .T. ) ;
#49350 = CARTESIAN_POINT ( 'NONE',  ( -46.62845405595144399, -24.51419770103157347, 9.386484678747180510 ) ) ;
#49351 = EDGE_LOOP ( 'NONE', ( #82240, #89016, #57195, #22431 ) ) ;
#49352 = DIRECTION ( 'NONE',  ( 0.000000000000000000, 1.000000000000000000, 0.000000000000000000 ) ) ;
#49353 = CARTESIAN_POINT ( 'NONE',  ( 6.361473516681357410, -20.28576754457002451, -1.500000000000002220 ) ) ;
#49354 = EDGE_LOOP ( 'NONE', ( #88245, #511, #11147, #84236 ) ) ;
#49355 = CARTESIAN_POINT ( 'NONE',  ( -88.63180385516216120, -24.15543982623907837, -0.2315651400026634832 ) ) ;
#49356 = CARTESIAN_POINT ( 'NONE',  ( 6.711561834375728175, -20.75310922853297058, -1.500000000000002220 ) ) ;
#49357 = CARTESIAN_POINT ( 'NONE',  ( -52.49087273462620118, -24.51419770103158413, 9.386484678747187615 ) ) ;
#49358 = B_SPLINE_CURVE_WITH_KNOTS ( 'NONE', 3,
 ( #89748, #12616, #43575, #74514, #5006, #91731 ),
 .UNSPECIFIED., .F., .F.,
 ( 4, 2, 4 ),
 ( 0.000000000000000000, 0.001380901958385383991, 0.002761803916770767982 ),
 .UNSPECIFIED. ) ;
#49359 = DIRECTION ( 'NONE',  ( -3.773278334453080206E-23, 0.9999999999976377785, 2.173523156925979975E-06 ) ) ;
#49360 = CARTESIAN_POINT ( 'NONE',  ( 5.400898774349120579, -5.876774720514417183, 20.36357656736558042 ) ) ;
#49361 = CARTESIAN_POINT ( 'NONE',  ( -15.17958814119055155, -15.74432251006154715, -1.500000000000002220 ) ) ;
#49362 = DIRECTION ( 'NONE',  ( -0.000000000000000000, 1.000000000000000000, -0.000000000000000000 ) ) ;
#49363 = ORIENTED_EDGE ( 'NONE', *, *, #87565, .F. ) ;
#49364 = ADVANCED_FACE ( 'NONE', ( #95519 ), #37844, .T. ) ;
#49365 = CARTESIAN_POINT ( 'NONE',  ( 29.57907552799942508, -3.316774720514426456, 29.21818156447043791 ) ) ;
#49366 = CARTESIAN_POINT ( 'NONE',  ( -85.60742799767531608, -23.48786465467240703, 11.44779295918254647 ) ) ;
#49367 = ORIENTED_EDGE ( 'NONE', *, *, #69313, .T. ) ;
#49368 = CARTESIAN_POINT ( 'NONE',  ( 32.25183987940364005, -0.3587747205144265483, 2.026414261721653176 ) ) ;
#49369 = ORIENTED_EDGE ( 'NONE', *, *, #58219, .F. ) ;
#49370 = CARTESIAN_POINT ( 'NONE',  ( -58.62287095715004881, -29.50248528299804818, 1.056150453629034924 ) ) ;
#49371 = CARTESIAN_POINT ( 'NONE',  ( -82.56324448010200001, -23.48783264082478439, -1.443836473390069486 ) ) ;
#49372 = CARTESIAN_POINT ( 'NONE',  ( -7.948041996521916452, 19.69052605537007850, 11.49999999999998934 ) ) ;
#49373 = DIRECTION ( 'NONE',  ( 0.000000000000000000, 1.000000000000000000, 1.478457507934778393E-16 ) ) ;
#49374 = CARTESIAN_POINT ( 'NONE',  ( -30.60515864328932878, -24.57438384523503316, 0.5319095616429412310 ) ) ;
#49375 = CIRCLE ( 'NONE', #2360, 1.835999999999931465 ) ;
#49376 = CARTESIAN_POINT ( 'NONE',  ( -114.5228709571500616, -24.64898659630529565, 1.056161002820831474 ) ) ;
#49377 = CARTESIAN_POINT ( 'NONE',  ( -68.64045969480598330, -23.96119346886880663, -0.6495511937832112448 ) ) ;
#49378 = CARTESIAN_POINT ( 'NONE',  ( 7.440116899146960172, 17.95454168335740874, -1.500000000000002220 ) ) ;
#49379 = CARTESIAN_POINT ( 'NONE',  ( -45.48070769923166523, -24.73486907724918282, 1.287355809206962576 ) ) ;
#49380 = ORIENTED_EDGE ( 'NONE', *, *, #58258, .F. ) ;
#49381 = CARTESIAN_POINT ( 'NONE',  ( -7.007757480239389380, 18.17491015770016816, 11.49999999999999645 ) ) ;
#49382 = CARTESIAN_POINT ( 'NONE',  ( -5.533628790199073499, -6.376774720514417183, 19.87297243748313491 ) ) ;
#49383 = B_SPLINE_CURVE_WITH_KNOTS ( 'NONE', 3,
 ( #40059, #63414, #55798, #48178 ),
 .UNSPECIFIED., .F., .F.,
 ( 4, 4 ),
 ( 4.653101527641955381E-09, 0.0004001893594499267054 ),
 .UNSPECIFIED. ) ;
#49384 = CARTESIAN_POINT ( 'NONE',  ( -28.67218957988115235, -24.78612079304045679, 7.984269984107190687 ) ) ;
#49385 = EDGE_CURVE ( 'NONE', #62379, #50557, #19388, .T. ) ;
#49386 = ORIENTED_EDGE ( 'NONE', *, *, #39279, .F. ) ;
#49387 = AXIS2_PLACEMENT_3D ( 'NONE', #74510, #42586, #51687 ) ;
#49388 = CARTESIAN_POINT ( 'NONE',  ( 3.960462906497916435, -6.376774720514427841, 21.82884394085917279 ) ) ;
#49389 = CARTESIAN_POINT ( 'NONE',  ( -89.50577417353618159, -24.51314013834317862, 0.6176544820404262781 ) ) ;
#49390 = DIRECTION ( 'NONE',  ( 3.614007241618349141E-17, -9.637352644315597708E-17, -1.000000000000000000 ) ) ;
#49391 = EDGE_CURVE ( 'NONE', #10252, #20796, #97514, .T. ) ;
#49392 = CARTESIAN_POINT ( 'NONE',  ( -29.62287095715004881, -24.57333416927490433, 1.056161302446588124 ) ) ;
#49393 = CARTESIAN_POINT ( 'NONE',  ( 11.96684523812195700, 15.63349346248531546, 11.49999999999998934 ) ) ;
#49394 = EDGE_LOOP ( 'NONE', ( #58671, #82999, #26352, #94465 ) ) ;
#49396 = B_SPLINE_CURVE_WITH_KNOTS ( 'NONE', 3,
 ( #4200, #35154, #10810, #56001 ),
 .UNSPECIFIED., .F., .F.,
 ( 4, 4 ),
 ( 0.000000000000000000, 9.999999999998897304E-05 ),
 .UNSPECIFIED. ) ;
#49395 = PLANE ( 'NONE',  #35925 ) ;
#49397 = CARTESIAN_POINT ( 'NONE',  ( -3.594920434497504758, 22.80983129501555950, -1.500000000000002220 ) ) ;
#49398 = PERSON_AND_ORGANIZATION ( #70597, #27821 ) ;
#49399 = EDGE_CURVE ( 'NONE', #27352, #95575, #11281, .T. ) ;
#49400 = ORIENTED_EDGE ( 'NONE', *, *, #18593, .F. ) ;
#49401 = DIRECTION ( 'NONE',  ( 1.000000000000000000, 3.773278334444166432E-23, 8.201307841325785021E-29 ) ) ;
#49402 = CARTESIAN_POINT ( 'NONE',  ( -1.955883090540335045, -6.376774720514411854, 19.49432735726521315 ) ) ;
#49403 = CARTESIAN_POINT ( 'NONE',  ( -109.4831753910024901, -25.15417620785191133, 3.089146885367800799 ) ) ;
#49404 = DIRECTION ( 'NONE',  ( -3.773278334453080206E-23, 0.9999999999976377785, 2.173523156925979975E-06 ) ) ;
#49405 = PLANE ( 'NONE',  #25612 ) ;
#49406 = CARTESIAN_POINT ( 'NONE',  ( -69.45824367449309023, -25.31201693057247937, 5.785093212486929204 ) ) ;
#49407 = CARTESIAN_POINT ( 'NONE',  ( -73.52287095715007581, -23.47593901973090169, -1.443836447538996870 ) ) ;
#49408 = CARTESIAN_POINT ( 'NONE',  ( -6.132916590032589710, 18.96384228413732842, -1.500000000000002220 ) ) ;
#49409 = EDGE_CURVE ( 'NONE', #51679, #63420, #65006, .T. ) ;
#49410 = B_SPLINE_CURVE_WITH_KNOTS ( 'NONE', 3,
 ( #23146, #42423, #95685, #87571 ),
 .UNSPECIFIED., .F., .F.,
 ( 4, 4 ),
 ( 0.8804146069980227640, 0.8894210382701381867 ),
 .UNSPECIFIED. ) ;
#49411 = CARTESIAN_POINT ( 'NONE',  ( -39.62287095715005592, -29.50248528299804818, 1.056150453629031594 ) ) ;
#49412 = CARTESIAN_POINT ( 'NONE',  ( 19.48829924427396421, 3.997931079995220127, -1.500000000000002220 ) ) ;
#49413 = ORIENTED_EDGE ( 'NONE', *, *, #14856, .F. ) ;
#49414 = DIRECTION ( 'NONE',  ( 0.000000000000000000, -0.000000000000000000, -1.000000000000000000 ) ) ;
#49415 = CARTESIAN_POINT ( 'NONE',  ( -125.5228709571500616, -23.47593901973090524, -1.443836447538996204 ) ) ;
#49416 = CARTESIAN_POINT ( 'NONE',  ( -72.62287095715005592, -24.64898659630367916, 1.056161002820824368 ) ) ;
#49417 = VECTOR ( 'NONE', #35419, 1000.000000000000114 ) ;
#49418 = CARTESIAN_POINT ( 'NONE',  ( 6.055070915967790235, -6.376774720518116446, -28.43998667026512095 ) ) ;
#49419 = CARTESIAN_POINT ( 'NONE',  ( 19.16185898538474675, 8.078635803559651052, 11.49999999999999645 ) ) ;
#49420 = CARTESIAN_POINT ( 'NONE',  ( -8.160000000000000142, -2.191226316053958875E-18, 2.701633758479787833E-17 ) ) ;
#49421 = CC_DESIGN_PERSON_AND_ORGANIZATION_ASSIGNMENT ( #12298, #89936, ( #11661 ) ) ;
#49422 = CARTESIAN_POINT ( 'NONE',  ( -50.50951590840232797, -25.18536261067197302, 3.296990267075738501 ) ) ;
#49423 = CARTESIAN_POINT ( 'NONE',  ( 17.70901601935662839, 14.43836031950349152, 11.49999999999999645 ) ) ;
#49424 = VERTEX_POINT ( 'NONE', #96516 ) ;
#49425 = CARTESIAN_POINT ( 'NONE',  ( -103.5228709571500758, -29.50250786944525672, 11.44777988621623166 ) ) ;
#49426 = DIRECTION ( 'NONE',  ( -1.000000000000000000, -0.000000000000000000, -0.000000000000000000 ) ) ;
#49427 = ORIENTED_EDGE ( 'NONE', *, *, #56796, .F. ) ;
#49428 = CARTESIAN_POINT ( 'NONE',  ( 6.697674113365701842, 19.09646837838083400, 11.49999999999998934 ) ) ;
#49429 = LINE ( 'NONE', #80863, #69563 ) ;
#49430 = CARTESIAN_POINT ( 'NONE',  ( 33.13288845015618023, -5.965225279485572685, -0.1650522222209214185 ) ) ;
#49431 = DIRECTION ( 'NONE',  ( 0.000000000000000000, 0.000000000000000000, 1.000000000000000000 ) ) ;
#49432 = ORIENTED_EDGE ( 'NONE', *, *, #87194, .F. ) ;
#49433 = CARTESIAN_POINT ( 'NONE',  ( -79.61344979208379868, -25.31277616797718366, 5.267994557577900139 ) ) ;
#49434 = CARTESIAN_POINT ( 'NONE',  ( 14.43441819135929371, -3.316774720514426456, -28.36222020317710246 ) ) ;
#49435 = CARTESIAN_POINT ( 'NONE',  ( -14.92271332039470444, 13.28099397388983327, -1.500000000000002220 ) ) ;
#49436 = CARTESIAN_POINT ( 'NONE',  ( -20.39251343623233836, 4.912230638944180328, 11.49999999999999645 ) ) ;
#49437 = CARTESIAN_POINT ( 'NONE',  ( -28.59609234217529306, -24.77774177186768156, 8.035888287207853864 ) ) ;
#49438 = CARTESIAN_POINT ( 'NONE',  ( -79.58953762381673869, -24.64965694238406968, 8.947790433994654791 ) ) ;
#49439 = CARTESIAN_POINT ( 'NONE',  ( 21.39010012190943755, 5.354582491813655309, 11.49999999999998934 ) ) ;
#49440 = AXIS2_PLACEMENT_3D ( 'NONE', #58408, #66538, #82221 ) ;
#49441 = CARTESIAN_POINT ( 'NONE',  ( -107.5228709571501042, -24.66019654487199730, 8.947790411086115725 ) ) ;
#49442 = ORIENTED_EDGE ( 'NONE', *, *, #68826, .F. ) ;
#49443 = DIRECTION ( 'NONE',  ( 0.000000000000000000, -2.173523156925980399E-06, 0.9999999999976378895 ) ) ;
#49444 = CARTESIAN_POINT ( 'NONE',  ( -118.5228709571500758, -24.64898659630368627, 1.056161002820833028 ) ) ;
#49445 = DIRECTION ( 'NONE',  ( -0.000000000000000000, 2.173523156925979552E-06, -0.9999999999976378895 ) ) ;
#49446 = ORIENTED_EDGE ( 'NONE', *, *, #60712, .T. ) ;
#49447 = DIRECTION ( 'NONE',  ( -1.000000000000000000, -3.773278334444167608E-23, -8.201307833595939069E-29 ) ) ;
#49448 = VERTEX_POINT ( 'NONE', #20375 ) ;
#49449 = ORIENTED_EDGE ( 'NONE', *, *, #48200, .F. ) ;
#49450 = EDGE_CURVE ( 'NONE', #49130, #61311, #50855, .T. ) ;
#49451 = PLANE ( 'NONE',  #53467 ) ;
#49452 = DIRECTION ( 'NONE',  ( -3.773278334453079030E-23, 0.9999999999976377785, 2.173523156925979128E-06 ) ) ;
#49453 = CARTESIAN_POINT ( 'NONE',  ( -122.5228709571500616, -23.48786465467241769, 11.44779295918253759 ) ) ;
#49454 = CARTESIAN_POINT ( 'NONE',  ( 11.66944253441096002, 16.90307425063352298, -1.500000000000002220 ) ) ;
#49455 = AXIS2_PLACEMENT_3D ( 'NONE', #2779, #73771, #26101 ) ;
#49456 = ORIENTED_EDGE ( 'NONE', *, *, #18826, .T. ) ;
#49457 = CARTESIAN_POINT ( 'NONE',  ( -20.27875734969026311, -7.835183881457444599, 24.00402280011862288 ) ) ;
#49458 = CARTESIAN_POINT ( 'NONE',  ( -10.22357262723052784, 3.975302591317960044, 29.38944064375215248 ) ) ;
#49459 = FACE_OUTER_BOUND ( 'NONE', #76697, .T. ) ;
#49460 = CARTESIAN_POINT ( 'NONE',  ( -16.35649155429130985, -15.18990082740072367, -1.500000000000002220 ) ) ;
#49461 = AXIS2_PLACEMENT_3D ( 'NONE', #18474, #49445, #58060 ) ;
#49462 = CARTESIAN_POINT ( 'NONE',  ( 32.64853395142472436, -3.736174708400741729, -2.687157883629963884 ) ) ;
#49463 = DIRECTION ( 'NONE',  ( -2.246662546894773332E-15, 7.121496375062676691E-15, -1.000000000000000000 ) ) ;
#49464 = ORIENTED_EDGE ( 'NONE', *, *, #77694, .F. ) ;
#49465 = CARTESIAN_POINT ( 'NONE',  ( -43.58953762381671737, -24.65952944569304606, 1.056160979905696351 ) ) ;
#49466 = DIRECTION ( 'NONE',  ( 3.278764309610055092E-18, 4.688851412615178005E-17, 1.000000000000000000 ) ) ;
#49467 = EDGE_CURVE ( 'NONE', #76836, #48580, #98931, .T. ) ;
#49468 = CARTESIAN_POINT ( 'NONE',  ( -2.238888094254589234, -20.74146561784671761, -1.500000000000002220 ) ) ;
#49469 = ADVANCED_FACE ( 'NONE', ( #73684 ), #43738, .T. ) ;
#49470 = ORIENTED_EDGE ( 'NONE', *, *, #77187, .T. ) ;
#49472 = EDGE_LOOP ( 'NONE', ( #1738, #64280, #18138, #96597 ) ) ;
#49471 = CARTESIAN_POINT ( 'NONE',  ( 14.73162737928355170, -3.582999323269832725, -27.37940951657878941 ) ) ;
#49473 = ORIENTED_EDGE ( 'NONE', *, *, #29255, .F. ) ;
#49474 = CARTESIAN_POINT ( 'NONE',  ( 10.34999999999999254, 4.999999999999998224, 0.000000000000000000 ) ) ;
#49475 = CARTESIAN_POINT ( 'NONE',  ( -8.945158345017247825, -19.07159632999312393, -1.500000000000002220 ) ) ;
#49476 = ORIENTED_EDGE ( 'NONE', *, *, #84017, .T. ) ;
#49477 = DIRECTION ( 'NONE',  ( -1.257682986112628661E-16, 0.000000000000000000, -1.000000000000000000 ) ) ;
#49478 = DIRECTION ( 'NONE',  ( 0.000000000000000000, 0.000000000000000000, -1.000000000000000000 ) ) ;
#49479 = CARTESIAN_POINT ( 'NONE',  ( -120.5884185014208612, -24.83644354573579349, 8.397322867130096569 ) ) ;
#49480 = CARTESIAN_POINT ( 'NONE',  ( -86.54785887183577131, -24.35071581493543391, 9.817618358456027039 ) ) ;
#49481 = CARTESIAN_POINT ( 'NONE',  ( -36.55620429048339304, -24.65952944569304606, 1.056160979905692132 ) ) ;
#49482 = CARTESIAN_POINT ( 'NONE',  ( -21.25272785503416273, -4.502612752106283978, -1.500000000000002220 ) ) ;
#49483 = CARTESIAN_POINT ( 'NONE',  ( -63.52287095715006160, -24.51387760970724372, 9.387446482453409402 ) ) ;
#49485 = ORIENTED_EDGE ( 'NONE', *, *, #59316, .F. ) ;
#49484 = CARTESIAN_POINT ( 'NONE',  ( -8.840690135214121170, 20.45858245768130956, 11.49999999999999645 ) ) ;
#49486 = ADVANCED_FACE ( 'NONE', ( #82290 ), #11778, .F. ) ;
#49487 = CARTESIAN_POINT ( 'NONE',  ( -51.27521478229555640, -25.24728804126394621, 5.568540310635312629 ) ) ;
#49488 = CARTESIAN_POINT ( 'NONE',  ( -41.32836283488544638, 2.803225279485573207, 39.26872235229541985 ) ) ;
#49489 = CARTESIAN_POINT ( 'NONE',  ( -71.29929988823592169, -25.25728961307881093, 6.086721405243116223 ) ) ;
#49490 = VERTEX_POINT ( 'NONE', #42751 ) ;
#49492 = VERTEX_POINT ( 'NONE', #36119 ) ;
#49491 = CARTESIAN_POINT ( 'NONE',  ( -5.891837592278976743, -6.376774720514418959, 20.62654306927474934 ) ) ;
#49493 = ORIENTED_EDGE ( 'NONE', *, *, #85502, .F. ) ;
#49494 = VECTOR ( 'NONE', #2228, 1000.000000000000000 ) ;
#49495 = CARTESIAN_POINT ( 'NONE',  ( 31.50451260799805198, -4.115674466082359650, -1.392914706732841790 ) ) ;
#49496 = DIRECTION ( 'NONE',  ( -0.000000000000000000, -1.000000000000000000, -0.000000000000000000 ) ) ;
#49497 = DIRECTION ( 'NONE',  ( 0.000000000000000000, -1.478457507934778393E-16, -1.000000000000000000 ) ) ;
#49498 = ORIENTED_EDGE ( 'NONE', *, *, #2877, .T. ) ;
#49499 = CARTESIAN_POINT ( 'NONE',  ( -42.62287095715004881, -23.48786465467240347, 11.44779295918255180 ) ) ;
#49500 = CARTESIAN_POINT ( 'NONE',  ( -4.914914792326205983, -21.87198836336805385, -1.500000000000002220 ) ) ;
#49501 = ORIENTED_EDGE ( 'NONE', *, *, #76721, .F. ) ;
#49502 = DIRECTION ( 'NONE',  ( -3.773278334453079030E-23, 0.9999999999976377785, 2.173523156925979128E-06 ) ) ;
#49503 = CARTESIAN_POINT ( 'NONE',  ( -94.56143569909596636, -23.48786465467241058, 11.44779295918254469 ) ) ;
#49504 = CARTESIAN_POINT ( 'NONE',  ( -39.45226965286418164, -25.29606862819456836, 4.310991840858520163 ) ) ;
#49505 = CARTESIAN_POINT ( 'NONE',  ( -7.749999999999996447, 24.84999999999999787, 0.000000000000000000 ) ) ;
#49506 = CARTESIAN_POINT ( 'NONE',  ( -30.60910590307086565, -24.37907397113049512, 9.703205396196695531 ) ) ;
#49507 = EDGE_CURVE ( 'NONE', #81696, #71483, #2094, .T. ) ;
#49508 = B_SPLINE_CURVE_WITH_KNOTS ( 'NONE', 3,
 ( #33408, #27303, #56774, #18189, #42045, #58264 ),
 .UNSPECIFIED., .F., .F.,
 ( 4, 2, 4 ),
 ( 6.384118678612889102E-06, 0.001386860460828375635, 0.002767336802978138423 ),
 .UNSPECIFIED. ) ;
#49509 = CARTESIAN_POINT ( 'NONE',  ( 13.16580039582533423, -14.52177825760336205, -1.500000000000002220 ) ) ;
#49510 = CARTESIAN_POINT ( 'NONE',  ( -87.52287095715006160, -23.47593901973090524, -1.443836447538996648 ) ) ;
#49511 = ORIENTED_EDGE ( 'NONE', *, *, #57305, .T. ) ;
#49512 = CARTESIAN_POINT ( 'NONE',  ( -15.55086147716002110, 14.89234021980106881, 11.49999999999998934 ) ) ;
#49513 = CARTESIAN_POINT ( 'NONE',  ( -75.55620429048337883, -25.00182538069145721, 7.747789668545099317 ) ) ;
#49514 = CARTESIAN_POINT ( 'NONE',  ( -71.01839045479064794, -25.12219088163715952, 6.841307120826038535 ) ) ;
#49515 = FACE_OUTER_BOUND ( 'NONE', #96867, .T. ) ;
#49516 = LINE ( 'NONE', #80450, #86049 ) ;
#49518 = CIRCLE ( 'NONE', #824, 0.3000000000000016542 ) ;
#49517 = CARTESIAN_POINT ( 'NONE',  ( 20.74614131242519477, 9.816050768296040729, -1.500000000000002220 ) ) ;
#49519 = ADVANCED_FACE ( 'NONE', ( #19880 ), #65102, .T. ) ;
#49520 = VECTOR ( 'NONE', #29319, 1000.000000000000114 ) ;
#49521 = SECURITY_CLASSIFICATION_LEVEL ( 'unclassified' ) ;
#49522 = CARTESIAN_POINT ( 'NONE',  ( -31.58953762381672092, -24.66019654487198665, 8.947790411086138818 ) ) ;
#49523 = CARTESIAN_POINT ( 'NONE',  ( -49.55329769530813167, -23.96119346886879953, -0.6495511937832113558 ) ) ;
#49524 = CARTESIAN_POINT ( 'NONE',  ( 16.71511084712224360, -11.16500066668146829, 11.49999999999999645 ) ) ;
#49525 = CARTESIAN_POINT ( 'NONE',  ( 5.092794675178905273, 3.306008726340172288, -27.56219045528442280 ) ) ;
#49526 = CARTESIAN_POINT ( 'NONE',  ( -32.54530050952666898, -24.15620529776627734, 10.23563542870661358 ) ) ;
#49528 = CARTESIAN_POINT ( 'NONE',  ( -121.6228709571500417, -24.64965695001469115, 8.947790433994175174 ) ) ;
#49527 = AXIS2_PLACEMENT_3D ( 'NONE', #92267, #67955, #90281 ) ;
#49529 = CARTESIAN_POINT ( 'NONE',  ( -102.5562042904833788, -24.64898659630528499, 1.056161002820828143 ) ) ;
#49530 = DIRECTION ( 'NONE',  ( -0.06975647374412546897, -0.9975640502598241977, 4.700301109882543835E-17 ) ) ;
#49531 = CARTESIAN_POINT ( 'NONE',  ( -15.99800673754971037, 11.70972097625665675, 11.49999999999998934 ) ) ;
#49532 = AXIS2_PLACEMENT_3D ( 'NONE', #30225, #61699, #44474 ) ;
#49533 = CARTESIAN_POINT ( 'NONE',  ( 20.57455539870835182, 3.407774720514426647, -18.22080502500614330 ) ) ;
#49534 = CARTESIAN_POINT ( 'NONE',  ( -10.80270875523330965, -16.48872379891551532, -1.500000000000002220 ) ) ;
#49535 = VECTOR ( 'NONE', #75620, 1000.000000000000114 ) ;
#49536 = DIRECTION ( 'NONE',  ( 0.000000000000000000, -1.000000000000000000, 0.000000000000000000 ) ) ;
#49537 = PERSON_AND_ORGANIZATION ( #27119, #39406 ) ;
#49538 = CARTESIAN_POINT ( 'NONE',  ( -57.52287095715007581, -23.72773821059536914, 11.05748984161097326 ) ) ;
#49539 = CARTESIAN_POINT ( 'NONE',  ( 3.020285327128866992, -6.376774720514406525, 19.15473963397401391 ) ) ;
#49540 = CARTESIAN_POINT ( 'NONE',  ( -11.82494684808912844, 16.90534455221803967, 11.49999999999999645 ) ) ;
#49541 = EDGE_CURVE ( 'NONE', #61801, #78854, #92815, .T. ) ;
#49542 = PLANE ( 'NONE',  #31846 ) ;
#49543 = CARTESIAN_POINT ( 'NONE',  ( -10.49914784070103124, -20.09245350529190688, 11.49999999999999645 ) ) ;
#49544 = ORIENTED_EDGE ( 'NONE', *, *, #28353, .F. ) ;
#49545 = CARTESIAN_POINT ( 'NONE',  ( -69.45438311041971247, -25.25639499014904743, 6.630172782259688091 ) ) ;
#49546 = CARTESIAN_POINT ( 'NONE',  ( -97.50898914409353324, -24.51314013834316086, 0.6176544820404162861 ) ) ;
#49547 = CARTESIAN_POINT ( 'NONE',  ( -110.5228709571500332, -24.83602698348160231, 1.605859176311259295 ) ) ;
#49548 = PLANE ( 'NONE',  #56122 ) ;
#49549 = EDGE_CURVE ( 'NONE', #29476, #71994, #72021, .T. ) ;
#49550 = EDGE_CURVE ( 'NONE', #81022, #24863, #72518, .T. ) ;
#49551 = EDGE_LOOP ( 'NONE', ( #48458, #69012, #16527, #7677 ) ) ;
#49552 = CARTESIAN_POINT ( 'NONE',  ( -79.51137944035450289, -25.26749968020931192, 5.389239678618733542 ) ) ;
#49553 = CARTESIAN_POINT ( 'NONE',  ( -19.65108876255925807, -11.61119296138784662, 11.49999999999998934 ) ) ;
#49554 = CARTESIAN_POINT ( 'NONE',  ( -74.62362428499353939, -24.65952944569304606, 1.056160979905701680 ) ) ;
#49555 = FACE_OUTER_BOUND ( 'NONE', #69021, .T. ) ;
#49557 = EDGE_CURVE ( 'NONE', #99147, #56283, #41187, .T. ) ;
#49556 = CARTESIAN_POINT ( 'NONE',  ( -82.54711958133198380, -24.35071581493543036, 9.817618358456032368 ) ) ;
#49558 = CARTESIAN_POINT ( 'NONE',  ( 5.070899574700155732, -21.93562493352797915, 11.49999999999999645 ) ) ;
#49559 = ORIENTED_EDGE ( 'NONE', *, *, #83909, .T. ) ;
#49560 = CARTESIAN_POINT ( 'NONE',  ( -111.5228709571500758, -24.66019654487200441, 8.947790411086108620 ) ) ;
#49561 = CARTESIAN_POINT ( 'NONE',  ( -6.887433846447126307, -20.85920400149894149, -1.500000000000002220 ) ) ;
#49562 = CARTESIAN_POINT ( 'NONE',  ( -127.2834313257731367, -25.38352531986206273, 4.245363004327343148 ) ) ;
#49563 = CARTESIAN_POINT ( 'NONE',  ( -111.5524851600246734, -24.34968618360933945, 0.1864209137778883862 ) ) ;
#49564 = CARTESIAN_POINT ( 'NONE',  ( -70.25279295878802088, -25.03356033692018912, 7.559852777879553010 ) ) ;
#49565 = ORIENTED_EDGE ( 'NONE', *, *, #46005, .T. ) ;
#49566 = CARTESIAN_POINT ( 'NONE',  ( -48.63974770086845467, -24.15620529776627734, 10.23563542870660470 ) ) ;
#49567 = CARTESIAN_POINT ( 'NONE',  ( 0.03625801282051022839, -6.376774720514410077, 19.27714342948718240 ) ) ;
#49568 = ORIENTED_EDGE ( 'NONE', *, *, #8636, .T. ) ;
#49569 = CARTESIAN_POINT ( 'NONE',  ( -88.52287095715007581, -24.33832256527049509, 0.1851278514138626485 ) ) ;
#49570 = CARTESIAN_POINT ( 'NONE',  ( 14.40702264168333890, -14.58922348230443689, 11.49999999999998934 ) ) ;
#49571 = ORIENTED_EDGE ( 'NONE', *, *, #84368, .T. ) ;
#49572 = ORIENTED_EDGE ( 'NONE', *, *, #27171, .T. ) ;
#49573 = VERTEX_POINT ( 'NONE', #86726 ) ;
#49574 = EDGE_CURVE ( 'NONE', #90740, #19180, #72359, .T. ) ;
#49575 = CARTESIAN_POINT ( 'NONE',  ( -71.92287095715006728, -23.47593901973090169, -1.443836447538997536 ) ) ;
#49576 = CARTESIAN_POINT ( 'NONE',  ( 13.31140876108729998, -18.89465134148960956, -1.500000000000002220 ) ) ;
#49577 = CARTESIAN_POINT ( 'NONE',  ( -104.5154210034890951, -24.15620529776629155, 10.23563542870659759 ) ) ;
#49578 = CARTESIAN_POINT ( 'NONE',  ( -11.21218820807429140, -16.99972530465495169, -1.500000000000002220 ) ) ;
#49579 = EDGE_LOOP ( 'NONE', ( #79637, #33341, #83281, #87652 ) ) ;
#49580 = CARTESIAN_POINT ( 'NONE',  ( -70.52590259285405239, -25.03444510360072783, 7.555793054676811060 ) ) ;
#49581 = CARTESIAN_POINT ( 'NONE',  ( -29.54488130240525479, -24.07305817887745292, 10.23563548314527338 ) ) ;
#49582 = CARTESIAN_POINT ( 'NONE',  ( -89.43576144935765626, -25.11033443737753501, 2.832404817301928723 ) ) ;
#49583 = CARTESIAN_POINT ( 'NONE',  ( -70.52593452554701514, -25.25855380673795736, 7.557316893954395098 ) ) ;
#49584 = ORIENTED_EDGE ( 'NONE', *, *, #42073, .F. ) ;
#49585 = CARTESIAN_POINT ( 'NONE',  ( -29.00221282414159418, -24.76881061849349308, 3.230370487592436390 ) ) ;
#49586 = CARTESIAN_POINT ( 'NONE',  ( -93.52287095715004739, -24.33927499327855770, 9.819080762295802955 ) ) ;
#49587 = ORIENTED_EDGE ( 'NONE', *, *, #64031, .T. ) ;
#49588 = B_SPLINE_CURVE_WITH_KNOTS ( 'NONE', 3,
 ( #40604, #88278, #63965, #17761, #63455, #72063 ),
 .UNSPECIFIED., .F., .F.,
 ( 4, 2, 4 ),
 ( 6.391158118961560919E-06, 0.001387004593080777906, 0.002767618028042594189 ),
 .UNSPECIFIED. ) ;
#49589 = CARTESIAN_POINT ( 'NONE',  ( -7.357705842588929457, 19.43699106120834230, -1.500000000000002220 ) ) ;
#49590 = ADVANCED_FACE ( 'NONE', ( #32443 ), #94336, .T. ) ;
#49591 = ORIENTED_EDGE ( 'NONE', *, *, #54147, .F. ) ;
#49593 = ORIENTED_EDGE ( 'NONE', *, *, #2599, .F. ) ;
#49592 = CARTESIAN_POINT ( 'NONE',  ( -125.5562618372648416, -23.85016227208582151, -0.8807180028928047744 ) ) ;
#49594 = VECTOR ( 'NONE', #88112, 1000.000000000000000 ) ;
#49595 = EDGE_CURVE ( 'NONE', #70388, #16861, #41996, .T. ) ;
#49596 = FACE_OUTER_BOUND ( 'NONE', #7734, .T. ) ;
#49597 = CARTESIAN_POINT ( 'NONE',  ( -97.52287095715006160, -24.35013146730203815, 9.818937971375095941 ) ) ;
#49598 = VERTEX_POINT ( 'NONE', #86231 ) ;
#49599 = ORIENTED_EDGE ( 'NONE', *, *, #4337, .T. ) ;
#49600 = VECTOR ( 'NONE', #70937, 1000.000000000000000 ) ;
#49601 = LINE ( 'NONE', #72931, #17055 ) ;
#49602 = CARTESIAN_POINT ( 'NONE',  ( -98.58953762381672448, -23.48786465467241769, 11.44779295918254292 ) ) ;
#49603 = VECTOR ( 'NONE', #38253, 1000.000000000000114 ) ;
#49604 = CARTESIAN_POINT ( 'NONE',  ( -43.49278784741275672, -24.35071581493542681, 9.817618358456032368 ) ) ;
#49606 = ORIENTED_EDGE ( 'NONE', *, *, #80690, .F. ) ;
#49605 = CARTESIAN_POINT ( 'NONE',  ( -21.42919730060085115, -5.301375089729956969, 11.49999999999999645 ) ) ;
#49607 = ADVANCED_FACE ( 'NONE', ( #2505 ), #55800, .T. ) ;
#49608 = AXIS2_PLACEMENT_3D ( 'NONE', #59273, #5977, #5481 ) ;
#49609 = DIRECTION ( 'NONE',  ( 0.000000000000000000, -0.000000000000000000, -1.000000000000000000 ) ) ;
#49610 = CARTESIAN_POINT ( 'NONE',  ( -19.71520456405594857, 11.01310763156902972, -1.500000000000002220 ) ) ;
#49611 = VECTOR ( 'NONE', #52034, 1000.000000000000000 ) ;
#49612 = EDGE_CURVE ( 'NONE', #20569, #68532, #3905, .T. ) ;
#49614 = ORIENTED_EDGE ( 'NONE', *, *, #84082, .F. ) ;
#49613 = CARTESIAN_POINT ( 'NONE',  ( -127.6228709571500559, -29.50250786944525672, 11.44777988621622633 ) ) ;
#49615 = VERTEX_POINT ( 'NONE', #58782 ) ;
#49616 = DIRECTION ( 'NONE',  ( 0.000000000000000000, 0.000000000000000000, -1.000000000000000000 ) ) ;
#49617 = LINE ( 'NONE', #42006, #34379 ) ;
#49618 = ORIENTED_EDGE ( 'NONE', *, *, #12814, .F. ) ;
#49619 = CARTESIAN_POINT ( 'NONE',  ( -10.65520286329281596, -18.28862552182625123, 11.49999999999998934 ) ) ;
#49620 = CARTESIAN_POINT ( 'NONE',  ( -78.94558681842012504, -25.03137978718093493, 6.087055896365015428 ) ) ;
#49621 = CARTESIAN_POINT ( 'NONE',  ( -7.282824509310913186, -6.376774720514415407, 19.84584863393302356 ) ) ;
#49622 = CARTESIAN_POINT ( 'NONE',  ( -39.52287095715006870, -23.47593901973090524, -1.443836447538997092 ) ) ;
#49623 = CARTESIAN_POINT ( 'NONE',  ( 2.725811458822067657, 22.07344620009914138, -1.500000000000002220 ) ) ;
#49624 = CARTESIAN_POINT ( 'NONE',  ( -49.21454750704995007, -25.13941389702027251, 7.069183600260903866 ) ) ;
#49625 = B_SPLINE_CURVE_WITH_KNOTS ( 'NONE', 3,
 ( #66618, #5184, #89923, #10805 ),
 .UNSPECIFIED., .F., .F.,
 ( 4, 4 ),
 ( 0.000000000000000000, 9.999999999998897304E-05 ),
 .UNSPECIFIED. ) ;
#49626 = EDGE_LOOP ( 'NONE', ( #28954, #6628, #29487, #93980 ) ) ;
#49627 = CARTESIAN_POINT ( 'NONE',  ( 33.74607884027702909, 5.965225279485572685, -4.999864028243830916 ) ) ;
#49628 = CARTESIAN_POINT ( 'NONE',  ( -37.47959251893834676, -24.65952944569304250, 1.056160979905692576 ) ) ;
#49629 = CARTESIAN_POINT ( 'NONE',  ( -39.62287095715005592, -29.50250786944525672, 11.44777988621624232 ) ) ;
#49630 = FACE_OUTER_BOUND ( 'NONE', #77103, .T. ) ;
#49631 = EDGE_CURVE ( 'NONE', #59549, #18030, #28670, .T. ) ;
#49632 = CARTESIAN_POINT ( 'NONE',  ( 10.22484414329051994, 16.58839404647166660, -1.500000000000002220 ) ) ;
#49633 = CARTESIAN_POINT ( 'NONE',  ( 9.988417798295188277, 18.97302403871600518, -1.500000000000002220 ) ) ;
#49634 = CARTESIAN_POINT ( 'NONE',  ( -1.174900045708346497, -5.876774720514411854, 19.48569229636960998 ) ) ;
#49635 = DIRECTION ( 'NONE',  ( -0.1478094111296165969, 0.9890158633619159367, 0.000000000000000000 ) ) ;
#49636 = CARTESIAN_POINT ( 'NONE',  ( -77.56399945295062537, -23.48783264082476663, -1.443836473390097241 ) ) ;
#49637 = CARTESIAN_POINT ( 'NONE',  ( -7.601706241105644857, -21.46296766604531570, -1.500000000000002220 ) ) ;
#49638 = EDGE_CURVE ( 'NONE', #12728, #19742, #51673, .T. ) ;
#49639 = DIRECTION ( 'NONE',  ( -4.023404472900583808E-15, 0.9999991912942591821, 0.001271774676439518803 ) ) ;
#49640 = CARTESIAN_POINT ( 'NONE',  ( -98.58874431278923112, -24.34968618360934656, 0.1864209137778829184 ) ) ;
#49641 = CARTESIAN_POINT ( 'NONE',  ( -2.794871794871791604, -6.376774720514427841, 21.75000000000001066 ) ) ;
#49642 = CARTESIAN_POINT ( 'NONE',  ( -11.57717615966994273, 16.22069937712612031, 11.49999999999999645 ) ) ;
#49643 = CARTESIAN_POINT ( 'NONE',  ( -101.6228709571500985, -23.96177878511308990, 10.65340807706329507 ) ) ;
#49644 = CARTESIAN_POINT ( 'NONE',  ( -39.58112737576117013, -24.51419770103158413, 9.386484678747189392 ) ) ;
#49645 = CARTESIAN_POINT ( 'NONE',  ( -48.54086027304399664, -24.34968618360933945, 0.1864209137778883862 ) ) ;
#49646 = ORIENTED_EDGE ( 'NONE', *, *, #77808, .F. ) ;
#49647 = CARTESIAN_POINT ( 'NONE',  ( -25.57928830845510504, -24.89106019490560229, 4.019483868920429082 ) ) ;
#49648 = DIRECTION ( 'NONE',  ( -3.773278334453080206E-23, 0.9999999999976377785, 2.173523156925979975E-06 ) ) ;
#49649 = CARTESIAN_POINT ( 'NONE',  ( 16.47784684176308545, -14.13017478139203220, -1.500000000000002220 ) ) ;
#49650 = CARTESIAN_POINT ( 'NONE',  ( -51.92861116955014467, -25.24941396888022993, 6.270627690012409161 ) ) ;
#49651 = CARTESIAN_POINT ( 'NONE',  ( 12.07855387261060898, -15.37489856218140183, -1.500000000000002220 ) ) ;
#49652 = VECTOR ( 'NONE', #22773, 1000.000000000000000 ) ;
#49653 = FACE_OUTER_BOUND ( 'NONE', #70827, .T. ) ;
#49654 = ORIENTED_EDGE ( 'NONE', *, *, #96170, .T. ) ;
#49655 = SECURITY_CLASSIFICATION_LEVEL ( 'unclassified' ) ;
#49656 = CARTESIAN_POINT ( 'NONE',  ( -29.52287095715006160, -29.50250786944501158, 11.44777977277940550 ) ) ;
#49657 = CARTESIAN_POINT ( 'NONE',  ( -16.05948562299510485, -12.68841425896798469, 11.49999999999999645 ) ) ;
#49658 = CARTESIAN_POINT ( 'NONE',  ( -85.58953762381673869, -23.47593901973091235, -1.443836447539002865 ) ) ;
#49659 = AXIS2_PLACEMENT_3D ( 'NONE', #105, #83837, #14314 ) ;
#49660 = CARTESIAN_POINT ( 'NONE',  ( -39.62287095715006302, -24.33927499327853994, 9.819080762295820719 ) ) ;
#49661 = ADVANCED_FACE ( 'NONE', ( #28324 ), #35449, .T. ) ;
#49662 = ORIENTED_EDGE ( 'NONE', *, *, #4601, .F. ) ;
#49663 = CARTESIAN_POINT ( 'NONE',  ( -62.62287095715011986, -24.34917612406837861, 0.1852690917426612072 ) ) ;
#49664 = CARTESIAN_POINT ( 'NONE',  ( 30.93860345374796239, -5.965225279485572685, 28.07639619989137003 ) ) ;
#49665 = CIRCLE ( 'NONE', #56186, 18.35000000000000142 ) ;
#49666 = DIRECTION ( 'NONE',  ( -0.1254312216594016538, -0.000000000000000000, -0.9921023176230513441 ) ) ;
#49667 = AXIS2_PLACEMENT_3D ( 'NONE', #14126, #45103, #71284 ) ;
#49668 = DIRECTION ( 'NONE',  ( 0.5656310827093757876, -2.995395837334947501E-15, 0.8246584009594636333 ) ) ;
#49669 = ORIENTED_EDGE ( 'NONE', *, *, #49, .T. ) ;
#49670 = EDGE_CURVE ( 'NONE', #60943, #41466, #88135, .T. ) ;
#49671 = CARTESIAN_POINT ( 'NONE',  ( -66.54900992194662024, -24.15620529776628089, 10.23563542870660470 ) ) ;
#49672 = EDGE_CURVE ( 'NONE', #43797, #26418, #20700, .T. ) ;
#49673 = VECTOR ( 'NONE', #64278, 1000.000000000000114 ) ;
#49674 = EDGE_CURVE ( 'NONE', #44036, #47480, #62645, .T. ) ;
#49675 = CARTESIAN_POINT ( 'NONE',  ( 20.38051395842347802, -10.57019977742728578, 11.49999999999999645 ) ) ;
#49676 = CARTESIAN_POINT ( 'NONE',  ( 6.135622925040504327, -21.92205258971886650, 11.49999999999998934 ) ) ;
#49677 = CARTESIAN_POINT ( 'NONE',  ( -110.6272416013937629, -24.52399227489125266, 9.353111116836528183 ) ) ;
#49678 = CARTESIAN_POINT ( 'NONE',  ( 0.3000000000000007661, 0.000000000000000000, 0.000000000000000000 ) ) ;
#49679 = CARTESIAN_POINT ( 'NONE',  ( -90.62361245199505788, -25.00158670708910691, 2.256160236439220590 ) ) ;
#49680 = EDGE_CURVE ( 'NONE', #40241, #82993, #90727, .T. ) ;
#49681 = CARTESIAN_POINT ( 'NONE',  ( -66.52287095715006160, -23.48783264082476663, -1.443836473390092134 ) ) ;
#49682 = CARTESIAN_POINT ( 'NONE',  ( -70.26176671494545189, -25.13346133754408029, 7.099798033859436863 ) ) ;
#49683 = CARTESIAN_POINT ( 'NONE',  ( -20.57654891367511851, 7.437132321665034240, -1.500000000000002220 ) ) ;
#49684 = DIRECTION ( 'NONE',  ( 0.000000000000000000, 1.020425574104004369E-16, -1.000000000000000000 ) ) ;
#49685 = CARTESIAN_POINT ( 'NONE',  ( -26.65941713821050030, -24.79461012552177124, 2.761438400537009397 ) ) ;
#49686 = DIRECTION ( 'NONE',  ( 0.000000000000000000, 0.000000000000000000, 1.000000000000000000 ) ) ;
#49687 = CARTESIAN_POINT ( 'NONE',  ( -58.48922440719672977, -24.65952944569304606, 1.056160979905697461 ) ) ;
#49688 = EDGE_LOOP ( 'NONE', ( #59602, #17236, #17996, #10790 ) ) ;
#49689 = CARTESIAN_POINT ( 'NONE',  ( -6.584652030910324250, 19.34213596296284265, -1.500000000000002220 ) ) ;
#49690 = ORIENTED_EDGE ( 'NONE', *, *, #30644, .F. ) ;
#49691 = ORIENTED_EDGE ( 'NONE', *, *, #92956, .T. ) ;
#49692 = VERTEX_POINT ( 'NONE', #19207 ) ;
#49693 = EDGE_CURVE ( 'NONE', #70905, #51313, #96837, .T. ) ;
#49694 = EDGE_CURVE ( 'NONE', #51872, #78417, #81115, .T. ) ;
#49695 = CARTESIAN_POINT ( 'NONE',  ( -21.58539018223340022, -8.019882488244659768, -1.500000000000002220 ) ) ;
#49696 = CARTESIAN_POINT ( 'NONE',  ( -105.5562042904834215, -23.48783264082478794, -1.443836473390059716 ) ) ;
#49697 = CARTESIAN_POINT ( 'NONE',  ( -1.972954090310384379, -20.06304030521763337, -1.500000000000002220 ) ) ;
#49698 = VERTEX_POINT ( 'NONE', #42572 ) ;
#49699 = VECTOR ( 'NONE', #81892, 1000.000000000000114 ) ;
#49700 = CARTESIAN_POINT ( 'NONE',  ( -67.62287095715004170, -24.51387760970723306, 9.387446482453416507 ) ) ;
#49701 = CARTESIAN_POINT ( 'NONE',  ( 6.660000000000001030, -6.553980293839118509, 7.335060089566987962 ) ) ;
#49702 = ADVANCED_FACE ( 'NONE', ( #13086 ), #89732, .T. ) ;
#49703 = B_SPLINE_CURVE_WITH_KNOTS ( 'NONE', 3,
 ( #98270, #21641, #4944, #29774, #51121, #58733 ),
 .UNSPECIFIED., .F., .F.,
 ( 4, 2, 4 ),
 ( 0.000000000000000000, 0.001380764517854758677, 0.002761529035709517355 ),
 .UNSPECIFIED. ) ;
#49704 = CARTESIAN_POINT ( 'NONE',  ( 21.57151214508649772, 3.625915217019311583E-15, -1.699999999999999956 ) ) ;
#49705 = CARTESIAN_POINT ( 'NONE',  ( -53.63875462047889187, -24.15620529776627734, 10.23563542870660825 ) ) ;
#49707 = EDGE_LOOP ( 'NONE', ( #81641, #64689, #9276, #97170 ) ) ;
#49706 = CARTESIAN_POINT ( 'NONE',  ( -19.99122433398336440, 7.574256484821010105, 11.49999999999999645 ) ) ;
#49708 = ORIENTED_EDGE ( 'NONE', *, *, #759, .T. ) ;
#49709 = CARTESIAN_POINT ( 'NONE',  ( -4.481184387785930312, -21.81124396384582909, 11.49999999999998934 ) ) ;
#49710 = CARTESIAN_POINT ( 'NONE',  ( 18.97174343470660318, 8.267356841975738391, 11.49999999999998934 ) ) ;
#49711 = EDGE_CURVE ( 'NONE', #8718, #11023, #52167, .T. ) ;
#49712 = VERTEX_POINT ( 'NONE', #11596 ) ;
#49713 = DIRECTION ( 'NONE',  ( -1.084136044942898696E-16, -0.000000000000000000, 1.000000000000000000 ) ) ;
#49714 = CARTESIAN_POINT ( 'NONE',  ( -70.79599823016188509, -25.03707830618030172, 7.590867772707287742 ) ) ;
#49715 = VERTEX_POINT ( 'NONE', #65919 ) ;
#49716 = LINE ( 'NONE', #9632, #51039 ) ;
#49717 = ORIENTED_EDGE ( 'NONE', *, *, #48454, .F. ) ;
#49718 = CARTESIAN_POINT ( 'NONE',  ( -111.3776484685884185, -25.28710546256126079, 4.332404433089555695 ) ) ;
#49719 = CARTESIAN_POINT ( 'NONE',  ( -20.36979505965413395, -4.774807507659313721, -1.500000000000002220 ) ) ;
#49720 = CARTESIAN_POINT ( 'NONE',  ( 16.40513048700843513, 14.50174154637248591, 11.49999999999999645 ) ) ;
#49721 = ADVANCED_FACE ( 'NONE', ( #27827 ), #7130, .T. ) ;
#49722 = FACE_OUTER_BOUND ( 'NONE', #96889, .T. ) ;
#49723 = CARTESIAN_POINT ( 'NONE',  ( 19.74966320730700176, -10.79507447929251107, -1.500000000000002220 ) ) ;
#49724 = CARTESIAN_POINT ( 'NONE',  ( 9.933205088616889000, -18.45388779576350302, 11.49999999999998934 ) ) ;
#49725 = EDGE_CURVE ( 'NONE', #47965, #41069, #57794, .T. ) ;
#49726 = CARTESIAN_POINT ( 'NONE',  ( -26.27733073949819698, -24.97067096850452472, 6.353770577458710989 ) ) ;
#49727 = CARTESIAN_POINT ( 'NONE',  ( -108.8968792378191495, -25.09877477843093629, 7.294521336928838195 ) ) ;
#49728 = LINE ( 'NONE', #95382, #28153 ) ;
#49729 = ORIENTED_EDGE ( 'NONE', *, *, #28812, .T. ) ;
#49730 = EDGE_CURVE ( 'NONE', #18995, #57039, #74986, .T. ) ;
#49731 = VERTEX_POINT ( 'NONE', #34943 ) ;
#49732 = ORIENTED_EDGE ( 'NONE', *, *, #23866, .F. ) ;
#49733 = CARTESIAN_POINT ( 'NONE',  ( -52.59912246993389573, -23.96119346886881019, -0.6495511937831939253 ) ) ;
#49734 = VERTEX_POINT ( 'NONE', #12092 ) ;
#49735 = AXIS2_PLACEMENT_3D ( 'NONE', #6981, #91211, #68878 ) ;
#49736 = CARTESIAN_POINT ( 'NONE',  ( 20.92345209525186078, -4.499874906010187026, -1.500000000000002220 ) ) ;
#49737 = B_SPLINE_CURVE_WITH_KNOTS ( 'NONE', 3,
 ( #41652, #43146, #56885, #64510, #74092, #2588 ),
 .UNSPECIFIED., .F., .F.,
 ( 4, 2, 4 ),
 ( 0.000000000000000000, 0.001380901958385388761, 0.002761803916770777523 ),
 .UNSPECIFIED. ) ;
#49738 = ORIENTED_EDGE ( 'NONE', *, *, #17308, .T. ) ;
#49739 = CARTESIAN_POINT ( 'NONE',  ( -28.58953762381671737, -23.31699783904767287, 11.44779300560929514 ) ) ;
#49740 = VECTOR ( 'NONE', #33599, 1000.000000000000000 ) ;
#49741 = CARTESIAN_POINT ( 'NONE',  ( 18.35617536642501690, 10.39506492455470088, -1.500000000000002220 ) ) ;
#49742 = CARTESIAN_POINT ( 'NONE',  ( -30.60105355972280350, -24.67579744659554208, 8.908675929220796874 ) ) ;
#49743 = CARTESIAN_POINT ( 'NONE',  ( 3.251543564379332008, -6.376774720514424288, 21.68810402963413964 ) ) ;
#49744 = CARTESIAN_POINT ( 'NONE',  ( -43.52287095715006160, -23.47596703998600631, 11.44779298504229281 ) ) ;
#49745 = VECTOR ( 'NONE', #91009, 1000.000000000000114 ) ;
#49746 = CARTESIAN_POINT ( 'NONE',  ( -80.39981004835770761, -25.30877073141563827, 4.506608216669599543 ) ) ;
#49747 = CARTESIAN_POINT ( 'NONE',  ( -129.5221660731197630, -23.73791477778912551, 11.05961554403170055 ) ) ;
#49748 = CARTESIAN_POINT ( 'NONE',  ( -21.12052157030387889, 6.262089831203976331, -1.500000000000002220 ) ) ;
#49749 = VERTEX_POINT ( 'NONE', #43062 ) ;
#49750 = CARTESIAN_POINT ( 'NONE',  ( -65.58122294851770562, -24.83644354573579349, 8.397322867130094792 ) ) ;
#49751 = DIRECTION ( 'NONE',  ( 3.773278334444166432E-23, -1.000000000000000000, 0.000000000000000000 ) ) ;
#49752 = DIRECTION ( 'NONE',  ( 0.9822594791677485837, 0.000000000000000000, -0.1875268396392986980 ) ) ;
#49753 = VECTOR ( 'NONE', #80670, 1000.000000000000000 ) ;
#49754 = CARTESIAN_POINT ( 'NONE',  ( -28.40056905271415744, -24.97190405984839146, 2.662461283694066871 ) ) ;
#49755 = CARTESIAN_POINT ( 'NONE',  ( -0.02075734969026423599, 5.965225279485572685, -0.08597719988137648983 ) ) ;
#49756 = LINE ( 'NONE', #50245, #49852 ) ;
#49757 = CARTESIAN_POINT ( 'NONE',  ( 16.11712757473013014, 13.99349609535929773, -1.500000000000002220 ) ) ;
#49758 = CARTESIAN_POINT ( 'NONE',  ( -70.43046027505549489, -25.31470333651159166, 4.855693143746263374 ) ) ;
#49759 = CARTESIAN_POINT ( 'NONE',  ( -51.94816396996625940, -25.31392319263089519, 5.203681702801226550 ) ) ;
#49760 = LINE ( 'NONE', #3579, #51957 ) ;
#49761 = CARTESIAN_POINT ( 'NONE',  ( 32.16024265030974050, -5.965225279485572685, 16.27760796525321751 ) ) ;
#49762 = CARTESIAN_POINT ( 'NONE',  ( 14.20245820080859289, -17.52920931871068433, -1.500000000000002220 ) ) ;
#49763 = DIRECTION ( 'NONE',  ( 1.000000000000000000, 0.000000000000000000, 0.000000000000000000 ) ) ;
#49764 = ORIENTED_EDGE ( 'NONE', *, *, #77185, .F. ) ;
#49765 = DIRECTION ( 'NONE',  ( -0.000000000000000000, 1.000000000000000000, -0.000000000000000000 ) ) ;
#49766 = CARTESIAN_POINT ( 'NONE',  ( -79.50886169859143138, -24.15543982623907127, -0.2315651400026654261 ) ) ;
#49767 = CARTESIAN_POINT ( 'NONE',  ( 18.87426695099163254, 5.791883100666666451, 11.49999999999999645 ) ) ;
#49768 = CARTESIAN_POINT ( 'NONE',  ( -49.52287095715006870, -24.50216790748205398, 0.6166512839542435120 ) ) ;
#49769 = DIRECTION ( 'NONE',  ( 3.389844910009033029E-15, -1.000000000000000000, 0.000000000000000000 ) ) ;
#49770 = ORIENTED_EDGE ( 'NONE', *, *, #49550, .F. ) ;
#49771 = CARTESIAN_POINT ( 'NONE',  ( -80.13654269935766195, -25.21083105912962097, 3.409327675794633361 ) ) ;
#49772 = CARTESIAN_POINT ( 'NONE',  ( -29.81116077451118329, -24.60094588784620839, 4.841837093663297509 ) ) ;
#49773 = CARTESIAN_POINT ( 'NONE',  ( -101.1944152955115044, -25.12268512865201586, 6.858246136620771871 ) ) ;
#49774 = CARTESIAN_POINT ( 'NONE',  ( 2.580163054138214562, 21.43444414123800712, -1.500000000000002220 ) ) ;
#49775 = CIRCLE ( 'NONE', #41658, 3.570000000000003837 ) ;
#49776 = CARTESIAN_POINT ( 'NONE',  ( -126.6228709571500559, -23.72773821059537269, 11.05748984161097681 ) ) ;
#49777 = DIRECTION ( 'NONE',  ( -3.773278334444167608E-23, 1.000000000000000000, 0.000000000000000000 ) ) ;
#49778 = CARTESIAN_POINT ( 'NONE',  ( -41.32836283488544638, 2.803225279485573207, 39.26872235229541985 ) ) ;
#49779 = LINE ( 'NONE', #12182, #15070 ) ;
#49780 = CARTESIAN_POINT ( 'NONE',  ( 5.507670110241905448, 19.00313184189250038, 11.49999999999998934 ) ) ;
#49781 = B_SPLINE_CURVE_WITH_KNOTS ( 'NONE', 3,
 ( #91292, #52241, #51235, #20267 ),
 .UNSPECIFIED., .F., .F.,
 ( 4, 4 ),
 ( 0.000000000000000000, 9.999999999997510880E-05 ),
 .UNSPECIFIED. ) ;
#49782 = ORIENTED_EDGE ( 'NONE', *, *, #32989, .T. ) ;
#49783 = CIRCLE ( 'NONE', #90250, 6.119803529381341534 ) ;
#49784 = CARTESIAN_POINT ( 'NONE',  ( -15.67655817637044890, 12.86142704545212290, 11.49999999999999645 ) ) ;
#49785 = CARTESIAN_POINT ( 'NONE',  ( 11.22265027773143231, 6.376774720513926908, -28.06709888789093554 ) ) ;
#49786 = ORIENTED_EDGE ( 'NONE', *, *, #7607, .F. ) ;
#49787 = LINE ( 'NONE', #26440, #63746 ) ;
#49788 = CARTESIAN_POINT ( 'NONE',  ( -37.52287095715006870, -24.66019654487199375, 8.947790411086122830 ) ) ;
#49789 = CARTESIAN_POINT ( 'NONE',  ( -51.52530242769704927, -25.25461990700743442, 6.116794828230213810 ) ) ;
#49790 = CARTESIAN_POINT ( 'NONE',  ( 23.91005183030481263, -2.682774720514426559, -14.40591128290692069 ) ) ;
#49791 = EDGE_CURVE ( 'NONE', #64023, #43186, #25059, .T. ) ;
#49792 = DIRECTION ( 'NONE',  ( -1.000000000000000000, 0.000000000000000000, -1.334402673828313586E-16 ) ) ;
#49793 = EDGE_CURVE ( 'NONE', #36340, #97022, #3259, .T. ) ;
#49794 = DIRECTION ( 'NONE',  ( 4.089440751051245812E-15, -1.000000000000000000, -1.042451643221144600E-15 ) ) ;
#49795 = CARTESIAN_POINT ( 'NONE',  ( 19.36564117097816862, 5.170944958934900804, -1.500000000000002220 ) ) ;
#49796 = ADVANCED_FACE ( 'NONE', ( #64671 ), #87981, .F. ) ;
#49797 = DIRECTION ( 'NONE',  ( -0.000000000000000000, -1.000000000000000000, -0.000000000000000000 ) ) ;
#49798 = VERTEX_POINT ( 'NONE', #39433 ) ;
#49799 = EDGE_CURVE ( 'NONE', #74994, #97261, #806, .T. ) ;
#49800 = AXIS2_PLACEMENT_3D ( 'NONE', #78653, #15267, #62459 ) ;
#49801 = ADVANCED_FACE ( 'NONE', ( #26583 ), #365, .F. ) ;
#49802 = CARTESIAN_POINT ( 'NONE',  ( -4.993225604111834137, -0.3587747205143964613, -29.11654937215279304 ) ) ;
#49803 = FACE_OUTER_BOUND ( 'NONE', #15610, .T. ) ;
#49804 = CARTESIAN_POINT ( 'NONE',  ( -100.5562042904833788, -24.99156044556202261, 7.747789690856172307 ) ) ;
#49805 = DIRECTION ( 'NONE',  ( 0.000000000000000000, 0.000000000000000000, 1.000000000000000000 ) ) ;
#49806 = CARTESIAN_POINT ( 'NONE',  ( -73.52211523830358431, -23.48783264082477018, -1.443836473390094355 ) ) ;
#49807 = CARTESIAN_POINT ( 'NONE',  ( 14.78821595474961192, 4.792189181182580526, -27.68628040864189899 ) ) ;
#49808 = CARTESIAN_POINT ( 'NONE',  ( -84.58953762381673869, -24.64898659630367561, 1.056161002820385164 ) ) ;
#49809 = ORIENTED_EDGE ( 'NONE', *, *, #14470, .T. ) ;
#49810 = AXIS2_PLACEMENT_3D ( 'NONE', #2436, #9537, #41497 ) ;
#49811 = CARTESIAN_POINT ( 'NONE',  ( 3.964343641299885146, 19.94596313931659992, -1.500000000000002220 ) ) ;
#49812 = VERTEX_POINT ( 'NONE', #33183 ) ;
#49813 = B_SPLINE_CURVE_WITH_KNOTS ( 'NONE', 3,
 ( #82603, #68877, #76475, #45057 ),
 .UNSPECIFIED., .F., .F.,
 ( 4, 4 ),
 ( 0.000000000000000000, 0.002094050480769216183 ),
 .UNSPECIFIED. ) ;
#49814 = EDGE_CURVE ( 'NONE', #47093, #91990, #75144, .T. ) ;
#49815 = CARTESIAN_POINT ( 'NONE',  ( -16.74478417649319084, -15.65585335247391896, -1.500000000000002220 ) ) ;
#49816 = CARTESIAN_POINT ( 'NONE',  ( 31.62831224182126988, 4.127879075750807480, 27.04291028225966542 ) ) ;
#49817 = CARTESIAN_POINT ( 'NONE',  ( -122.5228709571501042, -24.51283580621365132, 0.6167428607019895814 ) ) ;
#49818 = EDGE_LOOP ( 'NONE', ( #59705, #55075, #20777, #52473 ) ) ;
#49819 = B_SPLINE_CURVE_WITH_KNOTS ( 'NONE', 3,
 ( #22961, #60075, #83883, #69672, #7761, #53954 ),
 .UNSPECIFIED., .F., .F.,
 ( 4, 2, 4 ),
 ( 0.000000000000000000, 0.001380764517853251853, 0.002761529035706503706 ),
 .UNSPECIFIED. ) ;
#49820 = DIRECTION ( 'NONE',  ( 3.773278334444167608E-23, -1.000000000000000000, 0.000000000000000000 ) ) ;
#49821 = CARTESIAN_POINT ( 'NONE',  ( -50.04767967325393840, -25.26264170184645508, 7.063298022568840651 ) ) ;
#49822 = EDGE_CURVE ( 'NONE', #96700, #79877, #84362, .T. ) ;
#49823 = CARTESIAN_POINT ( 'NONE',  ( -30.47287095715007865, -24.75746604436832499, 8.625480456497754744 ) ) ;
#49824 = CARTESIAN_POINT ( 'NONE',  ( 13.39648796734645231, 16.42122281929413319, 11.49999999999999645 ) ) ;
#49825 = CARTESIAN_POINT ( 'NONE',  ( 19.81268554055766273, 9.900562300003143079, 11.49999999999998934 ) ) ;
#49826 = CARTESIAN_POINT ( 'NONE',  ( 13.11803791274172681, -15.88952355948706341, -1.500000000000002220 ) ) ;
#49827 = ORIENTED_EDGE ( 'NONE', *, *, #16198, .F. ) ;
#49828 = CARTESIAN_POINT ( 'NONE',  ( -111.5562042904833930, -23.48783264082479150, -1.443836473390061492 ) ) ;
#49829 = ORIENTED_EDGE ( 'NONE', *, *, #15057, .T. ) ;
#49830 = CARTESIAN_POINT ( 'NONE',  ( -54.61288136965932694, -23.48783264082476308, -1.443836473390098130 ) ) ;
#49831 = CARTESIAN_POINT ( 'NONE',  ( 2.598243466966731585, -5.876774720514413630, 20.31174627870924709 ) ) ;
#49832 = EDGE_LOOP ( 'NONE', ( #2772, #58766, #49501, #53708 ) ) ;
#49833 = VERTEX_POINT ( 'NONE', #25572 ) ;
#49834 = VERTEX_POINT ( 'NONE', #69881 ) ;
#49835 = CARTESIAN_POINT ( 'NONE',  ( -83.62287095715004170, -23.73907113216991860, -1.053371485793229256 ) ) ;
#49836 = CARTESIAN_POINT ( 'NONE',  ( -28.51174970316478863, -23.57371711286328519, 11.05961558438220926 ) ) ;
#49837 = CARTESIAN_POINT ( 'NONE',  ( -109.3584176993576591, -29.50249212968922308, 4.206193347771797875 ) ) ;
#49838 = CARTESIAN_POINT ( 'NONE',  ( -14.21563987850626276, 15.01860006206015008, -1.500000000000002220 ) ) ;
#49839 = CARTESIAN_POINT ( 'NONE',  ( 21.40858030128615397, -3.853468400179685727, 11.49999999999999645 ) ) ;
#49840 = ORIENTED_EDGE ( 'NONE', *, *, #78833, .F. ) ;
#49841 = CARTESIAN_POINT ( 'NONE',  ( -62.55620429048339304, -24.65952944569304606, 1.056160979905697905 ) ) ;
#49842 = CARTESIAN_POINT ( 'NONE',  ( -75.52287095715011844, -23.48783264082477373, -1.443836473390087694 ) ) ;
#49843 = CARTESIAN_POINT ( 'NONE',  ( 5.309366582633749054, -21.77581755331916824, -1.500000000000002220 ) ) ;
#49844 = EDGE_CURVE ( 'NONE', #8748, #76027, #87473, .T. ) ;
#49845 = DIRECTION ( 'NONE',  ( 0.000000000000000000, 0.000000000000000000, 1.000000000000000000 ) ) ;
#49846 = PLANE ( 'NONE',  #1116 ) ;
#49847 = VERTEX_POINT ( 'NONE', #48925 ) ;
#49848 = CARTESIAN_POINT ( 'NONE',  ( 29.58031977903354459, 3.717801497966991775, 29.19834312781581076 ) ) ;
#49849 = CARTESIAN_POINT ( 'NONE',  ( 13.59451591917074431, -3.316774720514426456, -28.23515841827053308 ) ) ;
#49850 = B_SPLINE_SURFACE_WITH_KNOTS ( 'NONE', 3, 3, ( 
 ( #34408, #96304, #56766, #81080 ),
 ( #4466, #49644, #12054, #73470 ),
 ( #18179, #41525, #27295, #26295 ),
 ( #66374, #57270, #42035, #72980 ),
 ( #49154, #65387, #80079, #10563 ),
 ( #34907, #19664, #35416, #97303 ),
 ( #59243, #21651, #20663, #97792 ) ),
 .UNSPECIFIED., .F., .F., .F.,
 ( 4, 3, 4 ),
 ( 4, 4 ),
 ( 0.7945040050992251413, 0.8970133687736508987, 0.9995227324480766562 ),
 ( 0.9097251710157197024, 0.9111578850782391381 ),
 .UNSPECIFIED. ) ;
#49851 = EDGE_LOOP ( 'NONE', ( #94493, #49786, #3900, #14888 ) ) ;
#49852 = VECTOR ( 'NONE', #26897, 1000.000000000000000 ) ;
#49853 = ORIENTED_EDGE ( 'NONE', *, *, #29330, .T. ) ;
#49854 = EDGE_CURVE ( 'NONE', #18022, #36077, #79853, .T. ) ;
#49855 = LINE ( 'NONE', #66588, #78151 ) ;
#49856 = ORIENTED_EDGE ( 'NONE', *, *, #24832, .T. ) ;
#49857 = B_SPLINE_CURVE_WITH_KNOTS ( 'NONE', 3,
 ( #35989, #43611, #19259, #52224 ),
 .UNSPECIFIED., .F., .F.,
 ( 4, 4 ),
 ( 0.000000000000000000, 9.999999999998206125E-05 ),
 .UNSPECIFIED. ) ;
#49858 = CARTESIAN_POINT ( 'NONE',  ( -17.78888362263414535, -11.56919986243916654, -1.500000000000002220 ) ) ;
#49859 = VERTEX_POINT ( 'NONE', #18956 ) ;
#49860 = CARTESIAN_POINT ( 'NONE',  ( -88.62596719604175632, -24.51314013834316086, 0.6176544820404141767 ) ) ;
#49861 = CARTESIAN_POINT ( 'NONE',  ( 21.83686239284238084, -0.8075297431944471471, -1.500000000000002220 ) ) ;
#49862 = CARTESIAN_POINT ( 'NONE',  ( -103.6250708163186118, -24.51419770103158058, 9.386484678747171628 ) ) ;
#49863 = LINE ( 'NONE', #67082, #55003 ) ;
#49864 = CARTESIAN_POINT ( 'NONE',  ( -111.7814946224345789, -25.28710546256127145, 4.332404433089555695 ) ) ;
#49865 = CARTESIAN_POINT ( 'NONE',  ( -21.47987282208850601, -4.139150239982721580, -1.500000000000002220 ) ) ;
#49866 = CARTESIAN_POINT ( 'NONE',  ( 6.697025426467099862, -5.876774720514423400, 21.43052570396496037 ) ) ;
#49867 = ORIENTED_EDGE ( 'NONE', *, *, #51790, .F. ) ;
#49868 = PLANE ( 'NONE',  #76111 ) ;
#49869 = CARTESIAN_POINT ( 'NONE',  ( -49.06509223983938739, -25.12782660346821828, 6.860564634149458385 ) ) ;
#49870 = CIRCLE ( 'NONE', #87075, 2.249999999999998668 ) ;
#49871 = ORIENTED_EDGE ( 'NONE', *, *, #15169, .F. ) ;
#49872 = CARTESIAN_POINT ( 'NONE',  ( 30.53060340732035982, -1.477225279485574028, 19.84760796525321780 ) ) ;
#49873 = ORIENTED_EDGE ( 'NONE', *, *, #41493, .T. ) ;
#49874 = DIRECTION ( 'NONE',  ( -3.773278334453079030E-23, 0.9999999999976377785, 2.173523156925979128E-06 ) ) ;
#49875 = CARTESIAN_POINT ( 'NONE',  ( -10.25850006537117487, -22.80581235653748706, 0.3010598746230520595 ) ) ;
#49876 = CARTESIAN_POINT ( 'NONE',  ( -19.44786352930952233, -8.617208915446557427, 11.49999999999998934 ) ) ;
#49877 = DIRECTION ( 'NONE',  ( 1.000000000000000000, 0.000000000000000000, 4.335561085774420994E-16 ) ) ;
#49878 = DIRECTION ( 'NONE',  ( 0.000000000000000000, 0.000000000000000000, -1.000000000000000000 ) ) ;
#49879 = FACE_OUTER_BOUND ( 'NONE', #95131, .T. ) ;
#49880 = VECTOR ( 'NONE', #12613, 1000.000000000000000 ) ;
#49881 = CARTESIAN_POINT ( 'NONE',  ( -84.62287095715008434, -23.96177878511308634, 10.65340807706329862 ) ) ;
#49882 = CARTESIAN_POINT ( 'NONE',  ( -19.27395093635484713, 2.380100695660296140, -1.500000000000002220 ) ) ;
#49883 = CARTESIAN_POINT ( 'NONE',  ( -117.5162819473935372, -24.66019654487200441, 8.947790411086112172 ) ) ;
#49884 = VERTEX_POINT ( 'NONE', #77476 ) ;
#49885 = CARTESIAN_POINT ( 'NONE',  ( 18.72186718581493636, -5.619560887262019300, 11.49999999999999645 ) ) ;
#49886 = CARTESIAN_POINT ( 'NONE',  ( -5.439936175300728927, -6.376774720514410077, 19.67454710845353816 ) ) ;
#49887 = AXIS2_PLACEMENT_3D ( 'NONE', #67972, #67465, #90294 ) ;
#49888 = CARTESIAN_POINT ( 'NONE',  ( -116.5562042904833930, -23.48786465467241769, 11.44779295918253759 ) ) ;
#49889 = ORIENTED_EDGE ( 'NONE', *, *, #86230, .T. ) ;
#49890 = CARTESIAN_POINT ( 'NONE',  ( -97.62287095715004170, -23.72747288104441665, -1.053458166803661111 ) ) ;
#49891 = CARTESIAN_POINT ( 'NONE',  ( -89.55819824587750588, -23.73766607897671221, -1.055555164236434473 ) ) ;
#49892 = DIRECTION ( 'NONE',  ( -1.000000000000000000, -3.773278334444167608E-23, -8.201307833595939069E-29 ) ) ;
#49893 = CARTESIAN_POINT ( 'NONE',  ( -81.83126432988071031, -25.24813773485163537, 6.560967144104515647 ) ) ;
#49894 = CARTESIAN_POINT ( 'NONE',  ( -9.385407830382300531, 17.29636241635495608, -1.500000000000002220 ) ) ;
#49895 = ORIENTED_EDGE ( 'NONE', *, *, #83330, .T. ) ;
#49896 = B_SPLINE_CURVE_WITH_KNOTS ( 'NONE', 3,
 ( #29905, #13173, #67987, #75074, #28911, #60873 ),
 .UNSPECIFIED., .F., .F.,
 ( 4, 2, 4 ),
 ( 1.570755371633856203E-05, 0.001396183895866086452, 0.002776660238015834278 ),
 .UNSPECIFIED. ) ;
#49897 = CARTESIAN_POINT ( 'NONE',  ( -78.52287095715006160, -24.34917612406837151, 0.1852690917426541017 ) ) ;
#49898 = CARTESIAN_POINT ( 'NONE',  ( -77.62287095715005592, -29.50250243563736774, 8.947779886222141599 ) ) ;
#49899 = APPROVAL_STATUS ( 'not_yet_approved' ) ;
#49900 = ORIENTED_EDGE ( 'NONE', *, *, #58488, .T. ) ;
#49901 = DIRECTION ( 'NONE',  ( -3.773278334453079618E-23, 0.9999999999976377785, 2.173523156925979975E-06 ) ) ;
#49902 = CARTESIAN_POINT ( 'NONE',  ( -105.6228709571499991, -24.51254535404256885, 9.355368623467647637 ) ) ;
#49903 = CARTESIAN_POINT ( 'NONE',  ( -47.52204414629284202, -23.48783264082478084, -1.443836473390071706 ) ) ;
#49904 = CARTESIAN_POINT ( 'NONE',  ( -83.62287095715005592, -29.50248528299804818, 1.056150453629038477 ) ) ;
#49905 = CARTESIAN_POINT ( 'NONE',  ( -78.92501255663768234, -25.29489613318244068, 6.057562805997258160 ) ) ;
#49906 = EDGE_CURVE ( 'NONE', #53781, #80749, #93207, .T. ) ;
#49907 = CARTESIAN_POINT ( 'NONE',  ( -109.6228709571500559, -23.47596703998600631, 11.44779298504227860 ) ) ;
#49908 = CARTESIAN_POINT ( 'NONE',  ( 10.24059822343752479, -6.376774720514426953, -2.394817856121274864E-14 ) ) ;
#49909 = CARTESIAN_POINT ( 'NONE',  ( -4.495603250223349612, -19.44740727768710187, 11.49999999999998934 ) ) ;
#49910 = EDGE_CURVE ( 'NONE', #72067, #9106, #10520, .T. ) ;
#49911 = CARTESIAN_POINT ( 'NONE',  ( -0.08481413156557598976, -21.95201441650188201, 10.11439756690867320 ) ) ;
#49912 = CARTESIAN_POINT ( 'NONE',  ( 18.06118663784855372, 8.336529998961283994, -1.500000000000002220 ) ) ;
#49913 = VERTEX_POINT ( 'NONE', #61782 ) ;
#49914 = AXIS2_PLACEMENT_3D ( 'NONE', #99736, #76409, #46476 ) ;
#49915 = CARTESIAN_POINT ( 'NONE',  ( -56.52287095715006870, -24.65952944569304606, 1.056160979905695463 ) ) ;
#49916 = EDGE_CURVE ( 'NONE', #58574, #61812, #23692, .T. ) ;
#49917 = B_SPLINE_CURVE_WITH_KNOTS ( 'NONE', 3,
 ( #6913, #76908, #86037, #99739 ),
 .UNSPECIFIED., .F., .F.,
 ( 4, 4 ),
 ( 0.000000000000000000, 9.999999999997510880E-05 ),
 .UNSPECIFIED. ) ;
#49918 = EDGE_CURVE ( 'NONE', #23306, #16634, #16626, .T. ) ;
#49919 = LINE ( 'NONE', #80850, #33360 ) ;
#49920 = CARTESIAN_POINT ( 'NONE',  ( 11.22265027772288093, -3.316774720514091612, -28.06709888818796017 ) ) ;
#49921 = CARTESIAN_POINT ( 'NONE',  ( 7.312689604342500260, -19.48077458720139532, 11.49999999999999645 ) ) ;
#49922 = PLANE ( 'NONE',  #11120 ) ;
#49923 = EDGE_CURVE ( 'NONE', #25116, #66785, #85099, .T. ) ;
#49924 = CARTESIAN_POINT ( 'NONE',  ( -62.58953762381673158, -23.47596703998600276, 11.44779298504227505 ) ) ;
#49925 = CARTESIAN_POINT ( 'NONE',  ( 10.78062712001149492, -20.16176685268226976, 11.49999999999999645 ) ) ;
#49926 = ORIENTED_EDGE ( 'NONE', *, *, #30438, .T. ) ;
#49927 = B_SPLINE_SURFACE_WITH_KNOTS ( 'NONE', 3, 3, ( 
 ( #79577, #26296, #58741, #73471 ),
 ( #50630, #57271, #66867, #90186 ),
 ( #4467, #88201, #57757, #35899 ),
 ( #3966, #13050, #34409, #27296 ),
 ( #18671, #64890, #49645, #35417 ),
 ( #97793, #58253, #65389, #95800 ),
 ( #72480, #28284, #80577, #89196 ) ),
 .UNSPECIFIED., .F., .F., .F.,
 ( 4, 3, 4 ),
 ( 4, 4 ),
 ( 0.0004766839783839649258, 0.1029713700210903998, 0.2054660560637968370 ),
 ( 0.8197025155639751093, 0.8210934493545416490 ),
 .UNSPECIFIED. ) ;
#49928 = CARTESIAN_POINT ( 'NONE',  ( -64.62287095715008434, -24.51283580621364422, 0.6167428607019749265 ) ) ;
#49929 = CARTESIAN_POINT ( 'NONE',  ( -92.52287095715006160, -23.95044443724992078, 10.65354141964649237 ) ) ;
#49930 = EDGE_LOOP ( 'NONE', ( #70204, #30541, #21949, #48319 ) ) ;
#49931 = CARTESIAN_POINT ( 'NONE',  ( -13.58233929615340152, 14.99024694321910900, -1.500000000000002220 ) ) ;
#49932 = B_SPLINE_CURVE_WITH_KNOTS ( 'NONE', 3,
 ( #68772, #29210, #91597, #30700 ),
 .UNSPECIFIED., .F., .F.,
 ( 4, 4 ),
 ( 0.000000000000000000, 1.000000000000000000 ),
 .UNSPECIFIED. ) ;
#49933 = CARTESIAN_POINT ( 'NONE',  ( 7.267403311989051318, -5.876774720514426065, 21.43157132964656952 ) ) ;
#49934 = PLANE ( 'NONE',  #27470 ) ;
#49935 = AXIS2_PLACEMENT_3D ( 'NONE', #61745, #39389, #92169 ) ;
#49936 = DIRECTION ( 'NONE',  ( -3.773278334453079030E-23, 0.9999999999976377785, 2.173523156925979128E-06 ) ) ;
#49937 = ORIENTED_EDGE ( 'NONE', *, *, #41195, .T. ) ;
#49938 = CARTESIAN_POINT ( 'NONE',  ( -106.2228709571500787, -23.47596703998600631, 11.44779298504227860 ) ) ;
#49939 = CARTESIAN_POINT ( 'NONE',  ( -100.6228709571500275, -24.82558206586150007, 1.605769216559626233 ) ) ;
#49940 = CARTESIAN_POINT ( 'NONE',  ( 13.83478396660306942, -14.44641118834825910, -1.500000000000002220 ) ) ;
#49941 = CARTESIAN_POINT ( 'NONE',  ( -20.94189920129180038, 1.864940847883316488, 11.49999999999999645 ) ) ;
#49942 = CARTESIAN_POINT ( 'NONE',  ( 14.76093561896379214, 6.475225279485574248, -26.55548769130089681 ) ) ;
#49943 = CYLINDRICAL_SURFACE ( 'NONE', #93514, 1.699999999999999734 ) ;
#49944 = CARTESIAN_POINT ( 'NONE',  ( 21.84380375219137349, -3.031640915038902762, 11.49999999999998934 ) ) ;
#49945 = VECTOR ( 'NONE', #11871, 1000.000000000000000 ) ;
#49946 = CARTESIAN_POINT ( 'NONE',  ( -39.54917078480641379, -25.27806004098935233, 4.610327274970852152 ) ) ;
#49947 = DIRECTION ( 'NONE',  ( -3.773278334453079030E-23, 0.9999999999976377785, 2.173523156925979128E-06 ) ) ;
#49948 = FACE_OUTER_BOUND ( 'NONE', #15939, .T. ) ;
#49949 = CARTESIAN_POINT ( 'NONE',  ( -72.58096839274725198, -24.65952944569304250, 1.056160979905695463 ) ) ;
#49950 = DIRECTION ( 'NONE',  ( 0.000000000000000000, -2.173523156925980399E-06, 0.9999999999976378895 ) ) ;
#49951 = ORIENTED_EDGE ( 'NONE', *, *, #6224, .F. ) ;
#49952 = VECTOR ( 'NONE', #34057, 1000.000000000000000 ) ;
#49953 = B_SPLINE_CURVE_WITH_KNOTS ( 'NONE', 3,
 ( #45163, #76087, #6585, #37540, #29919, #60886, #32426, #86211 ),
 .UNSPECIFIED., .F., .F.,
 ( 4, 2, 2, 4 ),
 ( -0.001240355328176894791, -0.0002398155169399769290, 0.0007607242942969409324, 0.002761803916770776655 ),
 .UNSPECIFIED. ) ;
#49954 = ORIENTED_EDGE ( 'NONE', *, *, #7663, .F. ) ;
#49955 = DIRECTION ( 'NONE',  ( 0.000000000000000000, 0.000000000000000000, -1.000000000000000000 ) ) ;
#49956 = DIRECTION ( 'NONE',  ( -0.9913618264504693300, 5.365801633547209345E-16, 0.1311553622875920033 ) ) ;
#49957 = FACE_OUTER_BOUND ( 'NONE', #90111, .T. ) ;
#49958 = CARTESIAN_POINT ( 'NONE',  ( -10.66544979547405347, 17.54311462378693420, -1.500000000000002220 ) ) ;
#49959 = ORIENTED_EDGE ( 'NONE', *, *, #13406, .T. ) ;
#49960 = CARTESIAN_POINT ( 'NONE',  ( 13.91401389203221406, 5.965225279485572685, 158.0376437107427137 ) ) ;
#49961 = CARTESIAN_POINT ( 'NONE',  ( 7.116579217368891541, -5.876774720514415407, 20.51774267661129869 ) ) ;
#49962 = LINE ( 'NONE', #63692, #14002 ) ;
#49963 = CARTESIAN_POINT ( 'NONE',  ( -21.99995728619510516, 3.820703864638951952, 11.49999999999998934 ) ) ;
#49964 = DIRECTION ( 'NONE',  ( 0.6599726524652365089, 0.000000000000000000, -0.7512896232465879898 ) ) ;
#49965 = CARTESIAN_POINT ( 'NONE',  ( -31.62287095715005236, -23.48783264082477729, -1.443836473390074149 ) ) ;
#49966 = ORIENTED_EDGE ( 'NONE', *, *, #93990, .T. ) ;
#49967 = CARTESIAN_POINT ( 'NONE',  ( -31.24388727629348494, -24.86181185134534388, 1.747789972853592610 ) ) ;
#49968 = CARTESIAN_POINT ( 'NONE',  ( 31.13513474936814163, 4.540774720514427543, 3.331262582247520143 ) ) ;
#49969 = VECTOR ( 'NONE', #6586, 1000.000000000000000 ) ;
#49970 = CARTESIAN_POINT ( 'NONE',  ( -6.911038104174170194, -19.68591361114308214, -1.500000000000002220 ) ) ;
#49971 = VERTEX_POINT ( 'NONE', #77968 ) ;
#49972 = EDGE_CURVE ( 'NONE', #48183, #90746, #98566, .T. ) ;
#49974 = EDGE_LOOP ( 'NONE', ( #6888, #88242, #10281, #80922 ) ) ;
#49973 = CARTESIAN_POINT ( 'NONE',  ( -39.22702504168157134, -25.21450095976316064, 3.515138031494141835 ) ) ;
#49975 = ORIENTED_EDGE ( 'NONE', *, *, #76568, .F. ) ;
#49976 = CARTESIAN_POINT ( 'NONE',  ( -68.94461706535129508, -25.03149113892856192, 6.371760577998683672 ) ) ;
#49977 = CARTESIAN_POINT ( 'NONE',  ( -8.250207518706217158, 19.40231308534122689, -1.500000000000002220 ) ) ;
#49978 = EDGE_CURVE ( 'NONE', #9703, #51976, #60034, .T. ) ;
#49979 = ORIENTED_EDGE ( 'NONE', *, *, #89971, .F. ) ;
#49980 = LINE ( 'NONE', #66210, #54370 ) ;
#49981 = CARTESIAN_POINT ( 'NONE',  ( 6.365284455128204399, -5.876774720514413630, 19.73076923076922640 ) ) ;
#49982 = CARTESIAN_POINT ( 'NONE',  ( -120.5526909221348575, -24.83644354573579349, 8.397322867130096569 ) ) ;
#49983 = DIRECTION ( 'NONE',  ( 0.000000000000000000, -0.9999999999976377785, -2.173523156925979128E-06 ) ) ;
#49984 = CARTESIAN_POINT ( 'NONE',  ( 13.91401389203221406, 6.475225279485573360, 158.0376437107427137 ) ) ;
#49985 = CARTESIAN_POINT ( 'NONE',  ( -21.46818342838279392, -2.986162219498790904, -1.500000000000002220 ) ) ;
#49986 = CARTESIAN_POINT ( 'NONE',  ( -81.45245898465185519, -25.24759656628838655, 6.419335927061524671 ) ) ;
#49988 = EDGE_LOOP ( 'NONE', ( #85399, #70697, #52955, #81992 ) ) ;
#49987 = CARTESIAN_POINT ( 'NONE',  ( 6.060481786824854389, 21.40074245971799627, 11.49999999999999645 ) ) ;
#49989 = CARTESIAN_POINT ( 'NONE',  ( -72.62287095715007013, -24.35013146730203815, 9.818937971375111928 ) ) ;
#49990 = CARTESIAN_POINT ( 'NONE',  ( 15.01415361830771467, 3.567044333682583890, -27.41917996821035430 ) ) ;
#49991 = LINE ( 'NONE', #26639, #10034 ) ;
#49992 = ORIENTED_EDGE ( 'NONE', *, *, #44919, .F. ) ;
#49994 = ORIENTED_EDGE ( 'NONE', *, *, #21002, .T. ) ;
#49993 = FACE_OUTER_BOUND ( 'NONE', #69049, .T. ) ;
#49995 = ORIENTED_EDGE ( 'NONE', *, *, #49793, .F. ) ;
#49996 = CARTESIAN_POINT ( 'NONE',  ( -53.01255352321339842, 2.682774720514426559, 35.59556822165056644 ) ) ;
#49997 = DIRECTION ( 'NONE',  ( -1.000000000000000000, 0.000000000000000000, 0.000000000000000000 ) ) ;
#49998 = DIRECTION ( 'NONE',  ( 3.773278334444166432E-23, -1.000000000000000000, 0.000000000000000000 ) ) ;
#49999 = CARTESIAN_POINT ( 'NONE',  ( 29.73860345376316872, -5.356774720514427379, 17.30421508979847189 ) ) ;
#50000 = ORIENTED_EDGE ( 'NONE', *, *, #81833, .F. ) ;
#50001 = CARTESIAN_POINT ( 'NONE',  ( -130.5728709571500872, -24.99287569232926387, 8.157771170601387567 ) ) ;
#50002 = CARTESIAN_POINT ( 'NONE',  ( -16.74552829020559130, -14.98668287627115170, -1.500000000000002220 ) ) ;
#50003 = ORIENTED_EDGE ( 'NONE', *, *, #54781, .F. ) ;
#50004 = CARTESIAN_POINT ( 'NONE',  ( -99.68246233598412687, -25.07904460479134912, 7.390530277590735331 ) ) ;
#50005 = CARTESIAN_POINT ( 'NONE',  ( -101.6314124882551795, -23.96169478059713853, 10.65365249895717881 ) ) ;
#50006 = CARTESIAN_POINT ( 'NONE',  ( 2.590388488674697953, -6.376774720514415407, 19.94764386045124027 ) ) ;
#50007 = CARTESIAN_POINT ( 'NONE',  ( -19.38764004357183524, 5.965225279485572685, -21.62823517627350611 ) ) ;
#50008 = AXIS2_PLACEMENT_3D ( 'NONE', #42922, #28678, #82948 ) ;
#50009 = CARTESIAN_POINT ( 'NONE',  ( -97.24791950549985131, -24.66459861931856778, 1.095224832288509198 ) ) ;
#50010 = CARTESIAN_POINT ( 'NONE',  ( 19.59400933563812330, 0.1774559437341752532, -1.500000000000002220 ) ) ;
#50011 = CARTESIAN_POINT ( 'NONE',  ( -59.52287095715006160, -24.65952944569304961, 1.056160979905695463 ) ) ;
#50012 = VERTEX_POINT ( 'NONE', #51417 ) ;
#50013 = B_SPLINE_CURVE_WITH_KNOTS ( 'NONE', 3,
 ( #9539, #94772, #40500, #1942, #63858, #25260, #56239, #13895 ),
 .UNSPECIFIED., .F., .F.,
 ( 4, 2, 2, 4 ),
 ( 0.000000000000000000, 0.002001098010032680181, 0.003001647015049020272, 0.004002196020065360363 ),
 .UNSPECIFIED. ) ;
#50014 = CARTESIAN_POINT ( 'NONE',  ( -21.28347836979250118, 3.227085873532868021, 11.49999999999998934 ) ) ;
#50015 = LINE ( 'NONE', #72846, #12330 ) ;
#50016 = CARTESIAN_POINT ( 'NONE',  ( -81.42380231474228935, -25.31572696169300585, 5.197788986266723477 ) ) ;
#50017 = CARTESIAN_POINT ( 'NONE',  ( -63.62287095715004881, -24.65952944569303895, 1.056160979905696129 ) ) ;
#50018 = DIRECTION ( 'NONE',  ( 0.000000000000000000, 0.000000000000000000, -1.000000000000000000 ) ) ;
#50019 = CARTESIAN_POINT ( 'NONE',  ( -12.88233675513024856, -19.01995677650982230, -1.500000000000002220 ) ) ;
#50020 = PERSON_AND_ORGANIZATION_ROLE ( 'design_supplier' ) ;
#50021 = CARTESIAN_POINT ( 'NONE',  ( -92.62287095715005592, -23.47593901973091235, -1.443836447539002865 ) ) ;
#50022 = FACE_OUTER_BOUND ( 'NONE', #78005, .T. ) ;
#50023 = CARTESIAN_POINT ( 'NONE',  ( 18.22116949570664701, -8.484823103377051368, 11.49999999999999645 ) ) ;
#50024 = CARTESIAN_POINT ( 'NONE',  ( 282.9764569301858046, -0.3587747205144265483, 20.79159422840526616 ) ) ;
#50025 = DIRECTION ( 'NONE',  ( 1.000000000000000000, -1.232047923278981953E-16, 0.000000000000000000 ) ) ;
#50026 = VECTOR ( 'NONE', #73994, 1000.000000000000227 ) ;
#50027 = CARTESIAN_POINT ( 'NONE',  ( -98.62287095715005592, -29.50248528299804818, 1.056150453629042030 ) ) ;
#50028 = CARTESIAN_POINT ( 'NONE',  ( 31.41423154468143153, 4.132774720514426292, -0.3119954678742140053 ) ) ;
#50029 = CARTESIAN_POINT ( 'NONE',  ( -126.6228709571500559, -24.64965695001469825, 8.947790433994173398 ) ) ;
#50030 = CARTESIAN_POINT ( 'NONE',  ( 16.83370257367741019, -10.51912618480096206, 11.49999999999998934 ) ) ;
#50031 = LINE ( 'NONE', #55642, #43125 ) ;
#50032 = CARTESIAN_POINT ( 'NONE',  ( 6.816645498261984848, 18.52099371530728789, -1.500000000000002220 ) ) ;
#50033 = CARTESIAN_POINT ( 'NONE',  ( -42.56072380411180944, -23.73766607897670156, -1.055555164236442689 ) ) ;
#50034 = AXIS2_PLACEMENT_3D ( 'NONE', #84832, #70617, #69106 ) ;
#50035 = COORDINATED_UNIVERSAL_TIME_OFFSET ( 0, 0, .AHEAD. ) ;
#50036 = ADVANCED_FACE ( 'NONE', ( #28568 ), #42815, .T. ) ;
#50037 = CARTESIAN_POINT ( 'NONE',  ( -115.6228709571499706, -24.14321612903118108, -0.2833117244521116684 ) ) ;
#50038 = CARTESIAN_POINT ( 'NONE',  ( 3.672440828437461224, -6.376774720514402972, 18.52532110411518573 ) ) ;
#50039 = CARTESIAN_POINT ( 'NONE',  ( 6.226698476505521995, -19.64469265145860177, 11.49999999999999645 ) ) ;
#50040 = EDGE_CURVE ( 'NONE', #11737, #24496, #55280, .T. ) ;
#50041 = DIRECTION ( 'NONE',  ( 0.000000000000000000, -0.9999999999976377785, -2.173523156925979975E-06 ) ) ;
#50042 = CARTESIAN_POINT ( 'NONE',  ( -2.919094682108430483, 22.50186656173435296, 11.49999999999999645 ) ) ;
#50043 = ORIENTED_EDGE ( 'NONE', *, *, #68339, .T. ) ;
#50044 = CARTESIAN_POINT ( 'NONE',  ( -69.70298246041917878, -25.25639558095986459, 6.901994508171235942 ) ) ;
#50045 = CARTESIAN_POINT ( 'NONE',  ( -50.44230859488045127, -25.31264664644561435, 4.735025439241685952 ) ) ;
#50046 = ADVANCED_FACE ( 'NONE', ( #90962 ), #74247, .T. ) ;
#50047 = CARTESIAN_POINT ( 'NONE',  ( -111.3758965426668084, -25.18392475019902577, 6.830256960825760615 ) ) ;
#50048 = CARTESIAN_POINT ( 'NONE',  ( -80.96226385320382235, -29.50248939449842922, 2.947779886236309377 ) ) ;
#50049 = ORIENTED_EDGE ( 'NONE', *, *, #1362, .F. ) ;
#50050 = CARTESIAN_POINT ( 'NONE',  ( 0.3849403830293018358, -5.876774720514418071, 20.45311193189268906 ) ) ;
#50051 = CARTESIAN_POINT ( 'NONE',  ( -9.520747347383798243, -20.79447232172871907, 11.49999999999998934 ) ) ;
#50052 = CARTESIAN_POINT ( 'NONE',  ( -98.58953762381672448, -24.64965694238407323, 8.947790433994651238 ) ) ;
#50053 = DIRECTION ( 'NONE',  ( 0.000000000000000000, 0.000000000000000000, -1.000000000000000000 ) ) ;
#50054 = LINE ( 'NONE', #15458, #92194 ) ;
#50055 = CARTESIAN_POINT ( 'NONE',  ( -17.96456891314058879, -13.58578184957126034, 11.49999999999999645 ) ) ;
#50056 = EDGE_LOOP ( 'NONE', ( #97001, #21815, #88248, #9532 ) ) ;
#50057 = DIRECTION ( 'NONE',  ( -1.000000000000000000, 0.000000000000000000, 0.000000000000000000 ) ) ;
#50058 = CARTESIAN_POINT ( 'NONE',  ( 21.77894307773758698, -2.757304969434911879, -1.500000000000002220 ) ) ;
#50059 = CARTESIAN_POINT ( 'NONE',  ( -111.5501966621663996, -24.65952944569305316, 1.056160979905705677 ) ) ;
#50060 = CARTESIAN_POINT ( 'NONE',  ( -29.17238308422418669, -25.21724654464993520, 6.041339601850384433 ) ) ;
#50061 = ORIENTED_EDGE ( 'NONE', *, *, #61263, .F. ) ;
#50062 = DIRECTION ( 'NONE',  ( -1.000000000000000000, -3.773278334444166432E-23, -8.201307841325785021E-29 ) ) ;
#50063 = PLANE ( 'NONE',  #7337 ) ;
#50064 = ORIENTED_EDGE ( 'NONE', *, *, #926, .T. ) ;
#50065 = CARTESIAN_POINT ( 'NONE',  ( -49.52287095715006160, -23.48786465467241769, 11.44779295918255002 ) ) ;
#50066 = VECTOR ( 'NONE', #68011, 1000.000000000000114 ) ;
#50067 = CARTESIAN_POINT ( 'NONE',  ( 18.14102482237423075, -9.550406459077080967, 11.49999999999998934 ) ) ;
#50068 = ORIENTED_EDGE ( 'NONE', *, *, #61593, .T. ) ;
#50069 = VECTOR ( 'NONE', #51109, 1000.000000000000000 ) ;
#50070 = ORIENTED_EDGE ( 'NONE', *, *, #40634, .F. ) ;
#50071 = VERTEX_POINT ( 'NONE', #51916 ) ;
#50072 = CARTESIAN_POINT ( 'NONE',  ( 21.57151214508649772, 3.625915217019311583E-15, 0.5000000000000000000 ) ) ;
#50073 = CARTESIAN_POINT ( 'NONE',  ( 1.702247502073919394, 23.03039350466679025, -1.500000000000002220 ) ) ;
#50074 = CARTESIAN_POINT ( 'NONE',  ( -102.5228709571500758, -29.50247984919015209, -1.443849546365050029 ) ) ;
#50075 = CARTESIAN_POINT ( 'NONE',  ( -19.47531982339030776, -5.969937916086089480, -1.500000000000002220 ) ) ;
#50076 = ORIENTED_EDGE ( 'NONE', *, *, #2463, .T. ) ;
#50077 = CARTESIAN_POINT ( 'NONE',  ( -1.036876607668611117, -5.876774720514417183, 20.14881673916291405 ) ) ;
#50078 = VECTOR ( 'NONE', #70919, 1000.000000000000000 ) ;
#50079 = CARTESIAN_POINT ( 'NONE',  ( -51.64970124796896300, -25.24249896790658454, 3.668597825874434282 ) ) ;
#50080 = EDGE_CURVE ( 'NONE', #57247, #85245, #21433, .T. ) ;
#50081 = CARTESIAN_POINT ( 'NONE',  ( -105.6281938531929256, -24.52300882791530157, 0.6510814631126371488 ) ) ;
#50082 = DIRECTION ( 'NONE',  ( 1.000000000000000000, -0.000000000000000000, -0.000000000000000000 ) ) ;
#50083 = VERTEX_POINT ( 'NONE', #97577 ) ;
#50084 = CARTESIAN_POINT ( 'NONE',  ( -29.24577077129365321, -25.21532183541616590, 4.691558442423485076 ) ) ;
#50085 = CARTESIAN_POINT ( 'NONE',  ( 10.75273025779354796, -6.376774720514426953, 23.03521261039436752 ) ) ;
#50086 = ORIENTED_EDGE ( 'NONE', *, *, #98592, .T. ) ;
#50087 = VECTOR ( 'NONE', #44795, 1000.000000000000114 ) ;
#50088 = CARTESIAN_POINT ( 'NONE',  ( -18.04518632387085830, 10.29925911722504317, 11.49999999999998934 ) ) ;
#50090 = ADVANCED_FACE ( 'NONE', ( #34694 ), #98062, .T. ) ;
#50089 = ORIENTED_EDGE ( 'NONE', *, *, #63878, .T. ) ;
#50092 = EDGE_LOOP ( 'NONE', ( #48859, #30848, #31111, #12174 ) ) ;
#50091 = CARTESIAN_POINT ( 'NONE',  ( -40.35516601162786543, -25.30533514595981970, 5.080719793522692207 ) ) ;
#50093 = LINE ( 'NONE', #1916, #84350 ) ;
#50094 = CARTESIAN_POINT ( 'NONE',  ( -51.76227918482971546, -25.29444715957360756, 5.533495090563274488 ) ) ;
#50095 = VERTEX_POINT ( 'NONE', #75234 ) ;
#50096 = ORIENTED_EDGE ( 'NONE', *, *, #15189, .F. ) ;
#50097 = DIRECTION ( 'NONE',  ( 1.000000000000000000, -0.000000000000000000, -0.000000000000000000 ) ) ;
#50098 = CARTESIAN_POINT ( 'NONE',  ( -68.62287095715005592, -24.35013146730203459, 9.818937971375113705 ) ) ;
#50099 = CARTESIAN_POINT ( 'NONE',  ( -43.60778276898914640, -23.73791477778911130, 11.05961554403171121 ) ) ;
#50101 = ORIENTED_EDGE ( 'NONE', *, *, #41100, .F. ) ;
#50100 = CARTESIAN_POINT ( 'NONE',  ( 17.94654606563480215, 12.89224558282342947, 11.49999999999999645 ) ) ;
#50102 = CARTESIAN_POINT ( 'NONE',  ( -103.6308616004146330, -23.96119346886881019, -0.6495511937832079141 ) ) ;
#50103 = CARTESIAN_POINT ( 'NONE',  ( -3.801653518169780366, -22.29579330195574016, -1.500000000000002220 ) ) ;
#50105 = ORIENTED_EDGE ( 'NONE', *, *, #66935, .T. ) ;
#50104 = CARTESIAN_POINT ( 'NONE',  ( -99.22737670894692030, -25.30351348175197046, 5.230124031126243800 ) ) ;
#50106 = B_SPLINE_CURVE_WITH_KNOTS ( 'NONE', 3,
 ( #58102, #12888, #51474, #65721, #20502, #59592 ),
 .UNSPECIFIED., .F., .F.,
 ( 4, 2, 4 ),
 ( 0.000000000000000000, 0.001380901958385394833, 0.002761803916770789666 ),
 .UNSPECIFIED. ) ;
#50107 = ORIENTED_EDGE ( 'NONE', *, *, #97294, .T. ) ;
#50108 = DIRECTION ( 'NONE',  ( 2.615445361545220718E-15, -6.974520964120588319E-15, 1.000000000000000000 ) ) ;
#50109 = CC_DESIGN_PERSON_AND_ORGANIZATION_ASSIGNMENT ( #73962, #6442, ( #90652 ) ) ;
#50110 = AXIS2_PLACEMENT_3D ( 'NONE', #31782, #38887, #94172 ) ;
#50111 = CARTESIAN_POINT ( 'NONE',  ( -128.5895376238167103, -23.48783264082479505, -1.443836473390056829 ) ) ;
#50112 = ORIENTED_EDGE ( 'NONE', *, *, #28502, .T. ) ;
#50113 = CARTESIAN_POINT ( 'NONE',  ( -7.741094375770895653, -19.69850519626218599, 11.49999999999998934 ) ) ;
#50114 = CARTESIAN_POINT ( 'NONE',  ( -6.989144439031651501, -6.376774720514410077, 19.51167604195716621 ) ) ;
#50115 = DIRECTION ( 'NONE',  ( -3.773278334453080206E-23, 0.9999999999976377785, 2.173523156925979552E-06 ) ) ;
#50116 = CARTESIAN_POINT ( 'NONE',  ( 13.76814385225720372, 17.53657229028232223, -1.500000000000002220 ) ) ;
#50117 = CARTESIAN_POINT ( 'NONE',  ( 3.252401863874215593, 0.3587747205143964613, -29.35688408629929214 ) ) ;
#50118 = VERTEX_POINT ( 'NONE', #28079 ) ;
#50119 = LINE ( 'NONE', #49627, #91917 ) ;
#50120 = DIRECTION ( 'NONE',  ( 0.000000000000000000, 0.000000000000000000, -1.000000000000000000 ) ) ;
#50121 = ADVANCED_FACE ( 'NONE', ( #88982 ), #36680, .T. ) ;
#50122 = CARTESIAN_POINT ( 'NONE',  ( 15.63605935613269438, -5.965225279485572685, -27.55169773172585934 ) ) ;
#50123 = DIRECTION ( 'NONE',  ( 1.000000000000000000, 0.000000000000000000, -2.615445361545220718E-15 ) ) ;
#50124 = B_SPLINE_CURVE_WITH_KNOTS ( 'NONE', 3,
 ( #37494, #36489, #14143, #67958, #20756, #84662, #76534, #67454, #98885, #98380, #5046, #75538, #22748, #90784 ),
 .UNSPECIFIED., .F., .F.,
 ( 4, 2, 2, 2, 2, 2, 4 ),
 ( 1.404617285391336434E-17, 0.0002430483912727410896, 0.0004860967825454681388, 0.0009721935650909229419, 0.001458290347636377691, 0.001701338738909113739, 0.001944387130181849570 ),
 .UNSPECIFIED. ) ;
#50125 = CARTESIAN_POINT ( 'NONE',  ( -7.634514033349506512, -17.95459398628807435, 11.49999999999998934 ) ) ;
#50126 = CARTESIAN_POINT ( 'NONE',  ( 18.57079561221590325, -10.74342183689097574, -1.500000000000002220 ) ) ;
#50127 = CARTESIAN_POINT ( 'NONE',  ( -0.4909855769230798139, -6.376774720514410077, 19.14743589743590135 ) ) ;
#50128 = DIRECTION ( 'NONE',  ( 0.000000000000000000, 0.000000000000000000, -1.000000000000000000 ) ) ;
#50129 = PLANE ( 'NONE',  #58758 ) ;
#50130 = CARTESIAN_POINT ( 'NONE',  ( -22.67762270672801250, 1.536325718666671225, -1.500000000000002220 ) ) ;
#50131 =( LENGTH_UNIT ( ) NAMED_UNIT ( * ) SI_UNIT ( .MILLI., .METRE. ) );
#50132 = CARTESIAN_POINT ( 'NONE',  ( -98.62981750425619509, -24.15543982623907837, -0.2315651400026625395 ) ) ;
#50133 = CARTESIAN_POINT ( 'NONE',  ( -5.366453405989236813, 0.000000000000000000, 19.30000000000000071 ) ) ;
#50134 = CARTESIAN_POINT ( 'NONE',  ( -18.10700488460823721, -8.296952762055457953, 11.49999999999999645 ) ) ;
#50135 = CARTESIAN_POINT ( 'NONE',  ( -104.5573922166538665, -23.73766607897670866, -1.055555164236449572 ) ) ;
#50136 = AXIS2_PLACEMENT_3D ( 'NONE', #84668, #15156, #46122 ) ;
#50138 = B_SPLINE_CURVE_WITH_KNOTS ( 'NONE', 3,
 ( #71112, #25428, #72119, #94433, #1601, #86327, #63010, #2609, #16811, #33045, #26442, #79207, #49789, #24920 ),
 .UNSPECIFIED., .F., .F.,
 ( 4, 2, 2, 2, 2, 2, 4 ),
 ( 0.000000000000000000, 0.0002092458945023362355, 0.0004184917890046724711, 0.0008369835780093458095, 0.001255475367014019256, 0.001464721261516361509, 0.001673967156018703979 ),
 .UNSPECIFIED. ) ;
#50137 = CARTESIAN_POINT ( 'NONE',  ( -42.62287095715004881, -23.48783264082477373, -1.443836473390072817 ) ) ;
#50139 = CARTESIAN_POINT ( 'NONE',  ( -76.62287095715007013, -23.47596703998600631, 11.44779298504227860 ) ) ;
#50140 = ADVANCED_FACE ( 'NONE', ( #50418 ), #12339, .T. ) ;
#50141 = ORIENTED_EDGE ( 'NONE', *, *, #31358, .T. ) ;
#50142 = PLANE ( 'NONE',  #93135 ) ;
#50143 = CARTESIAN_POINT ( 'NONE',  ( -3.749999999999999112, 25.69999999999999574, 0.000000000000000000 ) ) ;
#50144 = CARTESIAN_POINT ( 'NONE',  ( -10.76533847658563126, -18.86179312034942868, -1.500000000000002220 ) ) ;
#50145 = CARTESIAN_POINT ( 'NONE',  ( -51.93008509245395032, -25.25437732972921268, 6.222362237587184985 ) ) ;
#50146 = VECTOR ( 'NONE', #50833, 1000.000000000000000 ) ;
#50147 = CARTESIAN_POINT ( 'NONE',  ( -14.81708852449743929, -12.69844354874750181, -1.500000000000002220 ) ) ;
#50148 = CYLINDRICAL_SURFACE ( 'NONE', #71803, 28.96799999999999642 ) ;
#50149 = AXIS2_PLACEMENT_3D ( 'NONE', #43191, #58909, #25953 ) ;
#50150 = DATE_TIME_ROLE ( 'classification_date' ) ;
#50151 = AXIS2_PLACEMENT_3D ( 'NONE', #42574, #88741, #35941 ) ;
#50152 = LINE ( 'NONE', #11080, #71077 ) ;
#50153 = CARTESIAN_POINT ( 'NONE',  ( -19.64171699416042571, -5.764624264842452384, 11.49999999999999645 ) ) ;
#50154 = CARTESIAN_POINT ( 'NONE',  ( 5.097264368846952998, -6.475225279485573360, -27.56135813788808164 ) ) ;
#50155 = EDGE_CURVE ( 'NONE', #30829, #80400, #14093, .T. ) ;
#50156 = CARTESIAN_POINT ( 'NONE',  ( -118.6228709571500701, -24.65952944569305316, 1.056160979905706565 ) ) ;
#50157 = VECTOR ( 'NONE', #63471, 1000.000000000000114 ) ;
#50158 = ORIENTED_EDGE ( 'NONE', *, *, #1223, .F. ) ;
#50159 = CARTESIAN_POINT ( 'NONE',  ( 8.125595504227240085, -10.01787066753315614, 1.310587897985998174 ) ) ;
#50160 = CARTESIAN_POINT ( 'NONE',  ( -39.48699591144466581, -25.18431008553413974, 3.925287068261696266 ) ) ;
#50161 = CARTESIAN_POINT ( 'NONE',  ( -60.62287095715004881, -29.50248789122583659, 2.256150453626215580 ) ) ;
#50162 = LINE ( 'NONE', #33421, #32797 ) ;
#50163 = EDGE_CURVE ( 'NONE', #64023, #32109, #44308, .T. ) ;
#50164 = CARTESIAN_POINT ( 'NONE',  ( -109.6235285405774249, -24.65952944569305316, 1.056160979905708786 ) ) ;
#50165 = ORIENTED_EDGE ( 'NONE', *, *, #5648, .F. ) ;
#50166 = CARTESIAN_POINT ( 'NONE',  ( 5.671814302646631667, -6.376774720514418959, 20.58085404595000512 ) ) ;
#50167 = CARTESIAN_POINT ( 'NONE',  ( 21.12055942831636202, -9.126644407798330860, 11.49999999999999645 ) ) ;
#50168 = CARTESIAN_POINT ( 'NONE',  ( 21.64774270073068863, 7.000884456547583845, -1.500000000000002220 ) ) ;
#50169 = CARTESIAN_POINT ( 'NONE',  ( -110.6263895210551595, -24.63419186844610920, 9.035850630976920428 ) ) ;
#50170 = CARTESIAN_POINT ( 'NONE',  ( -10.34999999999997833, 22.00000000000000000, 0.000000000000000000 ) ) ;
#50171 = CARTESIAN_POINT ( 'NONE',  ( -90.55339685531903626, -24.15503026093913164, -0.2815557561904542538 ) ) ;
#50172 = LINE ( 'NONE', #41564, #93317 ) ;
#50173 = DIRECTION ( 'NONE',  ( 1.000000000000000000, -0.000000000000000000, 0.000000000000000000 ) ) ;
#50174 = CARTESIAN_POINT ( 'NONE',  ( -18.37190169643047355, -11.86832528159398237, 11.49999999999998934 ) ) ;
#50175 = CARTESIAN_POINT ( 'NONE',  ( -69.64019056953976872, -23.96169478059712787, 10.65365249895718414 ) ) ;
#50176 = CARTESIAN_POINT ( 'NONE',  ( 27.86270917940689174, 5.965225279485572685, 29.49402280011862487 ) ) ;
#50177 = CARTESIAN_POINT ( 'NONE',  ( -51.04357394935764347, -25.31543073408252553, 4.940877929217665887 ) ) ;
#50178 = CARTESIAN_POINT ( 'NONE',  ( -96.52287095715006160, -23.47596703998600631, 11.44779298504228215 ) ) ;
#50179 = VERTEX_POINT ( 'NONE', #13827 ) ;
#50180 = CARTESIAN_POINT ( 'NONE',  ( 9.511415417357532931, -18.05363124325620205, -1.500000000000002220 ) ) ;
#50181 = ORIENTED_EDGE ( 'NONE', *, *, #50529, .T. ) ;
#50182 = EDGE_LOOP ( 'NONE', ( #20839, #62148, #84993, #65862 ) ) ;
#50183 = VERTEX_POINT ( 'NONE', #19950 ) ;
#50184 = EDGE_LOOP ( 'NONE', ( #94516, #20790, #75786, #88977 ) ) ;
#50185 = CARTESIAN_POINT ( 'NONE',  ( -18.14924840124409045, -14.16824886576183040, 11.49999999999998934 ) ) ;
#50186 = DIRECTION ( 'NONE',  ( -0.000000000000000000, 2.173523156925979552E-06, -0.9999999999976378895 ) ) ;
#50187 = CARTESIAN_POINT ( 'NONE',  ( 17.48260522047220888, -10.12088315688240314, -1.500000000000002220 ) ) ;
#50188 = ORIENTED_EDGE ( 'NONE', *, *, #43400, .F. ) ;
#50189 = CARTESIAN_POINT ( 'NONE',  ( 32.45853543194704116, -5.965225279485572685, 9.169203677920338080 ) ) ;
#50190 = DIRECTION ( 'NONE',  ( 0.8219392559241307517, 0.5637660281018075370, 0.08114015731558725519 ) ) ;
#50191 = CARTESIAN_POINT ( 'NONE',  ( -95.58514916329862388, -24.83618233451450408, 1.606449574219538157 ) ) ;
#50192 = CARTESIAN_POINT ( 'NONE',  ( -53.56013297064492917, -23.73791477778911840, 11.05961554403170766 ) ) ;
#50194 = VERTEX_POINT ( 'NONE', #65664 ) ;
#50193 = CARTESIAN_POINT ( 'NONE',  ( -11.99125074976391048, 17.70416384622758343, 11.49999999999999645 ) ) ;
#50195 = CARTESIAN_POINT ( 'NONE',  ( -79.22287095715006444, -23.47596703998600631, 11.44779298504227860 ) ) ;
#50196 = EDGE_LOOP ( 'NONE', ( #77719, #80259, #62718, #34824 ) ) ;
#50197 = CARTESIAN_POINT ( 'NONE',  ( -12.31279356157217109, -18.55646752483835016, -1.500000000000002220 ) ) ;
#50198 = CARTESIAN_POINT ( 'NONE',  ( -18.22997975830956108, -9.740667652671243459, 11.49999999999998934 ) ) ;
#50199 = AXIS2_PLACEMENT_3D ( 'NONE', #55408, #31550, #86345 ) ;
#50200 = ORIENTED_EDGE ( 'NONE', *, *, #98010, .F. ) ;
#50201 = ADVANCED_FACE ( 'NONE', ( #27079 ), #73746, .T. ) ;
#50202 = CARTESIAN_POINT ( 'NONE',  ( 2.920210193027767076, -5.876774720514413630, 19.64065332113010243 ) ) ;
#50203 = ORIENTED_EDGE ( 'NONE', *, *, #47825, .T. ) ;
#50204 = CARTESIAN_POINT ( 'NONE',  ( -0.02075734969026423599, -3.316774720514426456, -0.08597719988137648983 ) ) ;
#50205 = AXIS2_PLACEMENT_3D ( 'NONE', #92451, #5729, #61029 ) ;
#50206 = ORIENTED_EDGE ( 'NONE', *, *, #96456, .F. ) ;
#50207 = CARTESIAN_POINT ( 'NONE',  ( 5.097264368844749427, 6.475225279485576024, -27.56135813788841560 ) ) ;
#50208 = CARTESIAN_POINT ( 'NONE',  ( -8.531171415479239073, -19.09552649099111221, -1.500000000000002220 ) ) ;
#50209 = CARTESIAN_POINT ( 'NONE',  ( -21.90371867972833542, 1.011951690471867060, 11.49999999999999645 ) ) ;
#50210 = CARTESIAN_POINT ( 'NONE',  ( -73.58434121117628024, -24.51419770103157347, 9.386484678747175181 ) ) ;
#50211 = CARTESIAN_POINT ( 'NONE',  ( -14.39138815452349718, -17.32352244779961481, 11.49999999999998934 ) ) ;
#50212 = AXIS2_PLACEMENT_3D ( 'NONE', #18747, #44596, #36978 ) ;
#50213 = CARTESIAN_POINT ( 'NONE',  ( 2.313481123293766206, -20.83243486019555135, -1.500000000000002220 ) ) ;
#50214 = CARTESIAN_POINT ( 'NONE',  ( -38.58689981970802307, -24.34968618360933235, 0.1864209137778849723 ) ) ;
#50215 = CARTESIAN_POINT ( 'NONE',  ( 5.671814302646631667, -6.376774720514418959, 20.58085404595000512 ) ) ;
#50216 = CARTESIAN_POINT ( 'NONE',  ( -119.5526336030634695, -24.66019654487200441, 8.947790411086108620 ) ) ;
#50217 = CARTESIAN_POINT ( 'NONE',  ( -7.999999999999996447, -5.876774720514426953, 0.000000000000000000 ) ) ;
#50218 = ORIENTED_EDGE ( 'NONE', *, *, #87945, .T. ) ;
#50219 = VERTEX_POINT ( 'NONE', #4741 ) ;
#50220 = VECTOR ( 'NONE', #88346, 1000.000000000000114 ) ;
#50221 = VERTEX_POINT ( 'NONE', #66665 ) ;
#50222 = CARTESIAN_POINT ( 'NONE',  ( -99.29890324015507019, -25.26221131662738628, 6.243173681414228682 ) ) ;
#50223 = ORIENTED_EDGE ( 'NONE', *, *, #50357, .F. ) ;
#50224 = EDGE_CURVE ( 'NONE', #44267, #12270, #85645, .T. ) ;
#50225 = VECTOR ( 'NONE', #23375, 1000.000000000000000 ) ;
#50226 = CARTESIAN_POINT ( 'NONE',  ( 19.19993882694861753, 9.668096177433461946, -1.500000000000002220 ) ) ;
#50227 = B_SPLINE_CURVE_WITH_KNOTS ( 'NONE', 3,
 ( #19538, #20044, #74333, #51007 ),
 .UNSPECIFIED., .F., .F.,
 ( 4, 4 ),
 ( 0.000000000000000000, 9.999999999994735322E-05 ),
 .UNSPECIFIED. ) ;
#50228 = CARTESIAN_POINT ( 'NONE',  ( -59.52287095715006870, -23.73907113216987952, -1.053371485793253459 ) ) ;
#50229 = CARTESIAN_POINT ( 'NONE',  ( 19.72786461798894209, 7.474574171381012100, 11.49999999999998934 ) ) ;
#50230 = DIRECTION ( 'NONE',  ( -2.352173255807804438E-16, 2.352173255807796056E-16, 1.000000000000000000 ) ) ;
#50231 = CARTESIAN_POINT ( 'NONE',  ( -0.02075734969026423599, 5.965225279485572685, -0.08597719988137648983 ) ) ;
#50232 = ADVANCED_FACE ( 'NONE', ( #22919 ), #46795, .T. ) ;
#50233 = CARTESIAN_POINT ( 'NONE',  ( -87.62287095715008434, -23.96127896941631619, -0.6493128931037798202 ) ) ;
#50234 = CARTESIAN_POINT ( 'NONE',  ( -99.12380231474227799, -29.50249168492682728, 4.001565943926128632 ) ) ;
#50235 = CARTESIAN_POINT ( 'NONE',  ( -129.5897715217587063, -24.15620529776629510, 10.23563542870659759 ) ) ;
#50236 = CARTESIAN_POINT ( 'NONE',  ( -16.84257673422482426, -14.26466048179180568, -1.500000000000002220 ) ) ;
#50237 = EDGE_LOOP ( 'NONE', ( #66294, #86697, #60697, #28247 ) ) ;
#50238 = CARTESIAN_POINT ( 'NONE',  ( -65.64503599903511599, -24.15602025860896518, 10.28564288303535257 ) ) ;
#50239 = FACE_OUTER_BOUND ( 'NONE', #14367, .T. ) ;
#50240 = CARTESIAN_POINT ( 'NONE',  ( -41.56322468833811712, -25.27955966736181992, 5.062029455345571805 ) ) ;
#50241 = EDGE_CURVE ( 'NONE', #56196, #32160, #7722, .T. ) ;
#50242 = EDGE_CURVE ( 'NONE', #64856, #30322, #44496, .T. ) ;
#50243 = CARTESIAN_POINT ( 'NONE',  ( -25.50557291889858647, -24.91754783335685985, 3.798368663089755515 ) ) ;
#50244 = EDGE_CURVE ( 'NONE', #11737, #19028, #100046, .T. ) ;
#50245 = CARTESIAN_POINT ( 'NONE',  ( -4.993225604111835914, -5.965225279485592225, -29.11654937215278593 ) ) ;
#50246 = CARTESIAN_POINT ( 'NONE',  ( -6.767052838139933080, -20.26514109264706676, -1.500000000000002220 ) ) ;
#50247 = CARTESIAN_POINT ( 'NONE',  ( -97.62287095715011276, -24.35013146730204170, 9.818937971375104823 ) ) ;
#50248 = CARTESIAN_POINT ( 'NONE',  ( -90.70836042551606226, -25.31973986624387862, 5.294390042787146200 ) ) ;
#50249 = CARTESIAN_POINT ( 'NONE',  ( -70.62287095715005592, -24.99156045073392463, 7.747789690856161648 ) ) ;
#50250 = FACE_OUTER_BOUND ( 'NONE', #85604, .T. ) ;
#50251 = CARTESIAN_POINT ( 'NONE',  ( 11.36372850657041589, -19.49111573544105624, -1.500000000000002220 ) ) ;
#50252 = CARTESIAN_POINT ( 'NONE',  ( -65.58953762381672448, -24.99156044556120193, 7.747789690856343725 ) ) ;
#50253 = ORIENTED_EDGE ( 'NONE', *, *, #12771, .F. ) ;
#50254 = DIRECTION ( 'NONE',  ( -0.000000000000000000, 1.000000000000000000, -0.000000000000000000 ) ) ;
#50255 = CARTESIAN_POINT ( 'NONE',  ( -42.52287095715005449, -29.50250243563736774, 8.947779886222148704 ) ) ;
#50256 = CARTESIAN_POINT ( 'NONE',  ( -12.15653940608521566, -15.58205587995076868, 11.49999999999999645 ) ) ;
#50257 = CARTESIAN_POINT ( 'NONE',  ( -59.62287095715007723, -23.96127896941632685, -0.6493128931037863705 ) ) ;
#50258 = CARTESIAN_POINT ( 'NONE',  ( -67.50094105798223154, -24.34968618360932879, 0.1864209137778810865 ) ) ;
#50259 = EDGE_CURVE ( 'NONE', #10252, #2274, #21452, .T. ) ;
#50260 = VERTEX_POINT ( 'NONE', #53912 ) ;
#50261 = CARTESIAN_POINT ( 'NONE',  ( -32.50560602629348494, -29.50248678627064081, 1.747779886239157809 ) ) ;
#50262 = CARTESIAN_POINT ( 'NONE',  ( -70.52287095715007581, -23.48786465467241769, 11.44779295918254647 ) ) ;
#50263 = DIRECTION ( 'NONE',  ( -3.773278334444166432E-23, 1.000000000000000000, 0.000000000000000000 ) ) ;
#50264 = CARTESIAN_POINT ( 'NONE',  ( -17.57154585214776077, 12.61476001598989782, 11.49999999999998934 ) ) ;
#50265 = CARTESIAN_POINT ( 'NONE',  ( -6.741682653110981249, -5.965225279485572685, 30.62569541381301619 ) ) ;
#50266 = CARTESIAN_POINT ( 'NONE',  ( -66.52287095715003318, -24.66019654487199375, 8.947790411086119278 ) ) ;
#50267 = CARTESIAN_POINT ( 'NONE',  ( -10.25272501932627378, -4.561466182953243909, 29.07579354015162210 ) ) ;
#50268 = CARTESIAN_POINT ( 'NONE',  ( -41.62287095715006302, -29.50247984919015209, -1.443849546365060466 ) ) ;
#50269 = CARTESIAN_POINT ( 'NONE',  ( -19.19514693104756375, 4.742496307885142315, -1.500000000000002220 ) ) ;
#50270 = VERTEX_POINT ( 'NONE', #612 ) ;
#50271 = CARTESIAN_POINT ( 'NONE',  ( -20.21730713243277933, 1.494317884549376974, 11.49999999999999645 ) ) ;
#50272 = CARTESIAN_POINT ( 'NONE',  ( 5.930937628982182908, -5.876774720514417183, 20.24478033514397524 ) ) ;
#50273 = VECTOR ( 'NONE', #75745, 1000.000000000000000 ) ;
#50274 = EDGE_CURVE ( 'NONE', #80473, #77786, #54910, .T. ) ;
#50275 = ADVANCED_FACE ( 'NONE', ( #99057 ), #91957, .T. ) ;
#50276 = VERTEX_POINT ( 'NONE', #75721 ) ;
#50277 = CARTESIAN_POINT ( 'NONE',  ( -45.62287095715004881, -23.48783264082478084, -1.443836473390070374 ) ) ;
#50278 = CARTESIAN_POINT ( 'NONE',  ( -106.9228709571500673, -23.47596703998600631, 11.44779298504227860 ) ) ;
#50279 = CARTESIAN_POINT ( 'NONE',  ( 29.80070917940689412, -6.475225279485573360, 27.39560796525321607 ) ) ;
#50280 = AXIS2_PLACEMENT_3D ( 'NONE', #88884, #12231, #43212 ) ;
#50281 = LINE ( 'NONE', #66028, #35983 ) ;
#50282 = DIRECTION ( 'NONE',  ( 1.000000000000000000, 0.000000000000000000, -0.000000000000000000 ) ) ;
#50283 = CARTESIAN_POINT ( 'NONE',  ( 14.85562765054232059, -13.46834898924134372, 11.49999999999998934 ) ) ;
#50284 = EDGE_CURVE ( 'NONE', #81499, #79071, #49175, .T. ) ;
#50285 = FACE_OUTER_BOUND ( 'NONE', #58341, .T. ) ;
#50286 = ORIENTED_EDGE ( 'NONE', *, *, #28812, .F. ) ;
#50287 = ADVANCED_FACE ( 'NONE', ( #61531 ), #29558, .F. ) ;
#50288 = EDGE_CURVE ( 'NONE', #50993, #75137, #21930, .T. ) ;
#50289 = VECTOR ( 'NONE', #8520, 1000.000000000000114 ) ;
#50290 = CARTESIAN_POINT ( 'NONE',  ( -50.34997525821440689, -25.26258885166322088, 4.735128382460500163 ) ) ;
#50291 = DIRECTION ( 'NONE',  ( -1.000000000000000000, 0.000000000000000000, -0.000000000000000000 ) ) ;
#50292 = DIRECTION ( 'NONE',  ( -0.2425356250363331356, 0.9701425001453318764, 0.000000000000000000 ) ) ;
#50293 = VECTOR ( 'NONE', #65434, 1000.000000000000000 ) ;
#50294 = CARTESIAN_POINT ( 'NONE',  ( -95.62287095715005592, -29.50247984919015209, -1.443849546365050029 ) ) ;
#50295 = CARTESIAN_POINT ( 'NONE',  ( -73.63908853846434965, -23.96119346886880663, -0.6495511937832115779 ) ) ;
#50296 = VECTOR ( 'NONE', #68578, 1000.000000000000114 ) ;
#50297 = CARTESIAN_POINT ( 'NONE',  ( 15.35137209921619572, 4.335618847589792324, -28.31916638425222033 ) ) ;
#50298 = AXIS2_PLACEMENT_3D ( 'NONE', #30314, #46061, #13586 ) ;
#50299 = CARTESIAN_POINT ( 'NONE',  ( -51.54504057323880772, -25.12100811749006724, 7.112893600995336740 ) ) ;
#50300 = ORIENTED_EDGE ( 'NONE', *, *, #19841, .F. ) ;
#50301 = CARTESIAN_POINT ( 'NONE',  ( -0.6891947355827284794, 20.32259304938107292, 11.49999999999998934 ) ) ;
#50302 = ORIENTED_EDGE ( 'NONE', *, *, #95655, .F. ) ;
#50303 = CARTESIAN_POINT ( 'NONE',  ( -22.40196285382242536, -4.882868457752029379, -1.500000000000002220 ) ) ;
#50304 = CARTESIAN_POINT ( 'NONE',  ( 31.61913385939691423, 4.417689821282788643, 26.66246549260776177 ) ) ;
#50305 = VERTEX_POINT ( 'NONE', #6720 ) ;
#50306 = CARTESIAN_POINT ( 'NONE',  ( -109.5228709571501469, -24.34917612406837861, 0.1852690917426614847 ) ) ;
#50307 = CARTESIAN_POINT ( 'NONE',  ( 14.99280666621547731, 3.498378956622122615, -27.33228583850618065 ) ) ;
#50308 = B_SPLINE_CURVE_WITH_KNOTS ( 'NONE', 3,
 ( #21334, #92357, #6124, #37076, #68041, #87250 ),
 .UNSPECIFIED., .F., .F.,
 ( 4, 2, 4 ),
 ( 1.570755371634454886E-05, 0.001396183895866091439, 0.002776660238015838614 ),
 .UNSPECIFIED. ) ;
#50309 = DIRECTION ( 'NONE',  ( -0.000000000000000000, -1.000000000000000000, -0.000000000000000000 ) ) ;
#50310 = CARTESIAN_POINT ( 'NONE',  ( -16.93204426113827310, 12.72334981527875186, 11.49999999999999645 ) ) ;
#50311 = CARTESIAN_POINT ( 'NONE',  ( 12.08182546098005972, -18.57710416600862402, 11.49999999999998934 ) ) ;
#50312 = CARTESIAN_POINT ( 'NONE',  ( 4.697267095454844998, -20.06606415395816967, -1.500000000000002220 ) ) ;
#50313 = B_SPLINE_CURVE_WITH_KNOTS ( 'NONE', 3,
 ( #28082, #5730, #12342, #28572, #35694, #50925 ),
 .UNSPECIFIED., .F., .F.,
 ( 4, 2, 4 ),
 ( 6.391158118958419274E-06, 0.001387004593080773786, 0.002767618028042589419 ),
 .UNSPECIFIED. ) ;
#50314 = EDGE_LOOP ( 'NONE', ( #57682, #66472, #84615, #27496 ) ) ;
#50315 = CARTESIAN_POINT ( 'NONE',  ( -41.55303143007999722, -23.96119346886880663, -0.6495511937831991434 ) ) ;
#50316 = ORIENTED_EDGE ( 'NONE', *, *, #29760, .T. ) ;
#50317 = CARTESIAN_POINT ( 'NONE',  ( -54.54771575810656259, -24.15543982623906416, -0.2315651400026691176 ) ) ;
#50318 = CARTESIAN_POINT ( 'NONE',  ( -126.6228709571500559, -23.48786465467242124, 11.44779295918253403 ) ) ;
#50319 = ORIENTED_EDGE ( 'NONE', *, *, #32701, .F. ) ;
#50320 = ORIENTED_EDGE ( 'NONE', *, *, #83716, .F. ) ;
#50321 = EDGE_LOOP ( 'NONE', ( #62687, #70663, #14901, #99100 ) ) ;
#50322 = DIRECTION ( 'NONE',  ( -0.1875268396392987258, -0.000000000000000000, -0.9822594791677485837 ) ) ;
#50323 = CARTESIAN_POINT ( 'NONE',  ( -28.49462909715936831, -23.99193123636717218, 10.23563545308467226 ) ) ;
#50324 = DIRECTION ( 'NONE',  ( 0.000000000000000000, -1.000000000000000000, 0.000000000000000000 ) ) ;
#50325 = CARTESIAN_POINT ( 'NONE',  ( 11.01739540223112357, 17.63107602209319680, -1.500000000000002220 ) ) ;
#50326 = CARTESIAN_POINT ( 'NONE',  ( -19.66401359581072583, -9.230316601043258018, 11.49999999999999645 ) ) ;
#50327 = VERTEX_POINT ( 'NONE', #37673 ) ;
#50328 = DIRECTION ( 'NONE',  ( 0.9980236263794188822, 0.000000000000000000, -0.06283980576413537855 ) ) ;
#50329 = DIRECTION ( 'NONE',  ( -1.000000000000000000, -1.413818403454611288E-16, 0.000000000000000000 ) ) ;
#50330 = CARTESIAN_POINT ( 'NONE',  ( 11.36419782745769069, 19.35538867594532775, 11.49999999999998934 ) ) ;
#50331 = CARTESIAN_POINT ( 'NONE',  ( 27.86270917940689174, 5.965225279485572685, 29.49402280011862487 ) ) ;
#50332 = CARTESIAN_POINT ( 'NONE',  ( -4.926336369345164279, -5.965225279485592225, -28.61095484066304451 ) ) ;
#50333 = ORIENTED_EDGE ( 'NONE', *, *, #97897, .F. ) ;
#50334 = PLANE ( 'NONE',  #84166 ) ;
#50335 = CARTESIAN_POINT ( 'NONE',  ( 12.78578435864683449, -3.995361385602315796, -28.02483137475221397 ) ) ;
#50336 = ORIENTED_EDGE ( 'NONE', *, *, #27550, .F. ) ;
#50337 = ORIENTED_EDGE ( 'NONE', *, *, #73490, .T. ) ;
#50338 = AXIS2_PLACEMENT_3D ( 'NONE', #31599, #37716, #100086 ) ;
#50339 = CARTESIAN_POINT ( 'NONE',  ( -69.62287095715005592, -24.66019654487199020, 8.947790411086131712 ) ) ;
#50340 = ORIENTED_EDGE ( 'NONE', *, *, #21798, .F. ) ;
#50341 = EDGE_CURVE ( 'NONE', #8989, #25591, #39524, .T. ) ;
#50342 = CARTESIAN_POINT ( 'NONE',  ( -14.93283513470682067, -15.21490397768744529, -1.500000000000002220 ) ) ;
#50343 = ORIENTED_EDGE ( 'NONE', *, *, #84028, .T. ) ;
#50344 = CARTESIAN_POINT ( 'NONE',  ( -88.52215625292510026, -23.48783264082476663, -1.443836473390093467 ) ) ;
#50345 = EDGE_CURVE ( 'NONE', #52778, #37312, #90305, .T. ) ;
#50346 = CARTESIAN_POINT ( 'NONE',  ( 4.919149715316761373, 21.27959583485438344, 11.49999999999998934 ) ) ;
#50347 = PLANE ( 'NONE',  #7633 ) ;
#50348 = CARTESIAN_POINT ( 'NONE',  ( 19.67839991682829748, -11.23141783594569354, -1.500000000000002220 ) ) ;
#50349 = CARTESIAN_POINT ( 'NONE',  ( -12.84880425037202656, -0.3587747205143964613, -26.59900746623529244 ) ) ;
#50350 = CARTESIAN_POINT ( 'NONE',  ( -49.52287095715004739, -24.66019654487198665, 8.947790411086131712 ) ) ;
#50351 = CARTESIAN_POINT ( 'NONE',  ( -21.08706934527708654, 5.832127334627817739, -1.500000000000002220 ) ) ;
#50352 = CARTESIAN_POINT ( 'NONE',  ( -66.62287095715008434, -23.96127896941632685, -0.6493128931037854823 ) ) ;
#50353 = VERTEX_POINT ( 'NONE', #53413 ) ;
#50354 = CARTESIAN_POINT ( 'NONE',  ( 25.97917928778648999, 4.259874112196678553, -11.44717982150283220 ) ) ;
#50355 = CARTESIAN_POINT ( 'NONE',  ( -126.5562042904833930, -24.65952944569305316, 1.056160979905706121 ) ) ;
#50356 = EDGE_CURVE ( 'NONE', #35380, #69709, #81855, .T. ) ;
#50357 = EDGE_CURVE ( 'NONE', #80017, #9599, #8732, .T. ) ;
#50358 = ORIENTED_EDGE ( 'NONE', *, *, #84226, .T. ) ;
#50359 = ADVANCED_FACE ( 'NONE', ( #49313 ), #30549, .T. ) ;
#50360 = CARTESIAN_POINT ( 'NONE',  ( -90.62287095715002749, -24.52232992886364116, 0.6492154411906042588 ) ) ;
#50361 = VECTOR ( 'NONE', #56111, 1000.000000000000000 ) ;
#50362 = EDGE_LOOP ( 'NONE', ( #30083, #93860, #66894 ) ) ;
#50363 = DIRECTION ( 'NONE',  ( 0.03244919754393515293, 0.000000000000000000, -0.9994733861282923959 ) ) ;
#50364 = ADVANCED_FACE ( 'NONE', ( #56928 ), #17340, .T. ) ;
#50365 = CARTESIAN_POINT ( 'NONE',  ( -20.42750280573200783, -23.78525073545353408, 0.8294870405985487194 ) ) ;
#50366 = CARTESIAN_POINT ( 'NONE',  ( -19.37389216307569129, 8.798533688548827669, -1.500000000000002220 ) ) ;
#50367 = CARTESIAN_POINT ( 'NONE',  ( 2.100208336950355914, 0.000000000000000000, 1.249999999999996003 ) ) ;
#50368 = CARTESIAN_POINT ( 'NONE',  ( 4.143214286797170409, 4.821574250326515099, -3.549999999999999378 ) ) ;
#50369 = DIRECTION ( 'NONE',  ( -3.773278334453080206E-23, 0.9999999999976377785, 2.173523156925979975E-06 ) ) ;
#50370 = B_SPLINE_CURVE_WITH_KNOTS ( 'NONE', 3,
 ( #25979, #88890, #2659, #95993 ),
 .UNSPECIFIED., .F., .F.,
 ( 4, 4 ),
 ( 2.275056424024757261E-09, 0.0003976735161906177281 ),
 .UNSPECIFIED. ) ;
#50371 = CARTESIAN_POINT ( 'NONE',  ( -68.54455071335534910, -24.34968618360933590, 0.1864209137778813363 ) ) ;
#50372 = DIRECTION ( 'NONE',  ( -1.000000000000000000, -0.000000000000000000, -0.000000000000000000 ) ) ;
#50373 = ORIENTED_EDGE ( 'NONE', *, *, #57296, .T. ) ;
#50374 = CARTESIAN_POINT ( 'NONE',  ( -18.58057592369839384, -6.135153870360039896, 11.49999999999999645 ) ) ;
#50375 = CARTESIAN_POINT ( 'NONE',  ( -108.5228709571500758, -23.72773821059537269, 11.05748984161097681 ) ) ;
#50376 = CARTESIAN_POINT ( 'NONE',  ( -29.71696354036009780, -25.17832945473821837, 6.228946167112972887 ) ) ;
#50377 = ADVANCED_FACE ( 'NONE', ( #10737 ), #63540, .F. ) ;
#50378 = ORIENTED_EDGE ( 'NONE', *, *, #72131, .F. ) ;
#50379 = CARTESIAN_POINT ( 'NONE',  ( -80.43221577628075636, -25.30553498687082481, 4.967019777649441359 ) ) ;
#50380 = DIRECTION ( 'NONE',  ( 0.000000000000000000, 0.000000000000000000, -1.000000000000000000 ) ) ;
#50381 = CARTESIAN_POINT ( 'NONE',  ( -52.52287095715006870, -29.50250786944525672, 11.44777988621624054 ) ) ;
#50382 = DIRECTION ( 'NONE',  ( -3.773278334453079618E-23, 0.9999999999976377785, 2.173523156925979975E-06 ) ) ;
#50384 = EDGE_CURVE ( 'NONE', #5245, #16063, #44303, .T. ) ;
#50383 = CARTESIAN_POINT ( 'NONE',  ( 16.89532177248590372, -10.13005384644002227, -1.500000000000002220 ) ) ;
#50385 = VERTEX_POINT ( 'NONE', #55414 ) ;
#50386 = CARTESIAN_POINT ( 'NONE',  ( -78.52287095715004739, -23.48783264082476308, -1.443836473390091468 ) ) ;
#50387 = LINE ( 'NONE', #11809, #2587 ) ;
#50388 = ADVANCED_FACE ( 'NONE', ( #48302 ), #88361, .F. ) ;
#50389 = APPROVAL_DATE_TIME ( #36155, #56877 ) ;
#50390 = ORIENTED_EDGE ( 'NONE', *, *, #76324, .F. ) ;
#50391 = DIRECTION ( 'NONE',  ( 0.000000000000000000, 0.08084198211964954695, -0.9967269304714136968 ) ) ;
#50392 = CARTESIAN_POINT ( 'NONE',  ( -60.22287095715005734, -23.47596703998600276, 11.44779298504227860 ) ) ;
#50393 = CARTESIAN_POINT ( 'NONE',  ( -47.50673741778126669, -23.96119346886880663, -0.6495511937831951466 ) ) ;
#50394 = CARTESIAN_POINT ( 'NONE',  ( -118.5537768141336556, -24.34968618360933945, 0.1864209137778906622 ) ) ;
#50395 = CARTESIAN_POINT ( 'NONE',  ( -78.93018284415475705, -25.03722721891040948, 7.590183713343858329 ) ) ;
#50396 = DIRECTION ( 'NONE',  ( -3.773278334453079618E-23, 0.9999999999976377785, 2.173523156925979975E-06 ) ) ;
#50397 = CARTESIAN_POINT ( 'NONE',  ( -50.62287095715007013, -24.82558206586143257, 1.605769216559449708 ) ) ;
#50398 = CARTESIAN_POINT ( 'NONE',  ( 1.593314845114734535, -19.89410510517485164, 11.49999999999998934 ) ) ;
#50399 = CARTESIAN_POINT ( 'NONE',  ( -0.01140452636522266625, -22.90235944405398527, 6.868750951901480661 ) ) ;
#50400 = CARTESIAN_POINT ( 'NONE',  ( 14.69432462292611952, 13.40460087117274490, -1.500000000000002220 ) ) ;
#50401 = ORIENTED_EDGE ( 'NONE', *, *, #81833, .T. ) ;
#50402 = FACE_OUTER_BOUND ( 'NONE', #38713, .T. ) ;
#50403 = EDGE_CURVE ( 'NONE', #78274, #23327, #21277, .T. ) ;
#50404 = CARTESIAN_POINT ( 'NONE',  ( -29.52287095715006160, -24.26578402247989175, 9.819127079432160343 ) ) ;
#50405 = CARTESIAN_POINT ( 'NONE',  ( 9.313311959394031447, -3.316774720514592545, -28.06297399525112013 ) ) ;
#50406 = CARTESIAN_POINT ( 'NONE',  ( 20.70993026999094511, 1.908435391604796028, 11.49999999999999645 ) ) ;
#50407 = CARTESIAN_POINT ( 'NONE',  ( -3.106028565906091998, -5.876774720514426953, 3.106028565906120864 ) ) ;
#50409 = EDGE_CURVE ( 'NONE', #16877, #76855, #68712, .T. ) ;
#50408 = VECTOR ( 'NONE', #54990, 1000.000000000000000 ) ;
#50410 = PLANE ( 'NONE',  #90674 ) ;
#50411 = ORIENTED_EDGE ( 'NONE', *, *, #14774, .T. ) ;
#50412 = CARTESIAN_POINT ( 'NONE',  ( 30.53060340732036337, -5.297812262124697469, 1.539714685317310483 ) ) ;
#50413 = CARTESIAN_POINT ( 'NONE',  ( -127.5214699268525607, -24.15543982623907837, -0.2315651400026539075 ) ) ;
#50414 = ORIENTED_EDGE ( 'NONE', *, *, #34428, .T. ) ;
#50415 = CARTESIAN_POINT ( 'NONE',  ( 19.68333694646799614, 4.735253856516091098, 11.49999999999998934 ) ) ;
#50416 = CARTESIAN_POINT ( 'NONE',  ( 6.698292889820671725, -5.876774720514424288, 21.80822233811499444 ) ) ;
#50417 = CARTESIAN_POINT ( 'NONE',  ( -129.6228709571500417, -23.47593901973091235, -1.443836447538995760 ) ) ;
#50418 = FACE_OUTER_BOUND ( 'NONE', #96126, .T. ) ;
#50419 = ORIENTED_EDGE ( 'NONE', *, *, #51327, .F. ) ;
#50420 = CARTESIAN_POINT ( 'NONE',  ( -79.34687923781922336, -25.27781941911278807, 5.960409260969139922 ) ) ;
#50421 = DIRECTION ( 'NONE',  ( -0.000000000000000000, 1.000000000000000000, -0.000000000000000000 ) ) ;
#50422 = AXIS2_PLACEMENT_3D ( 'NONE', #55499, #54491, #24030 ) ;
#50423 = CARTESIAN_POINT ( 'NONE',  ( 18.22975119132022215, -8.346483668847822557, -1.500000000000002220 ) ) ;
#50424 = CARTESIAN_POINT ( 'NONE',  ( 20.40321384664088811, -4.974606123342796060, 11.49999999999999645 ) ) ;
#50425 = AXIS2_PLACEMENT_3D ( 'NONE', #26787, #96796, #81578 ) ;
#50426 = CARTESIAN_POINT ( 'NONE',  ( -54.62287095715006302, -24.35013146730203815, 9.818937971375117257 ) ) ;
#50427 = CARTESIAN_POINT ( 'NONE',  ( 29.64064043116815128, 5.965225279485572685, 28.71191112024341408 ) ) ;
#50428 = CARTESIAN_POINT ( 'NONE',  ( -9.261969182712835646, 20.05037652441878038, -1.500000000000002220 ) ) ;
#50429 = CARTESIAN_POINT ( 'NONE',  ( -47.22287095715006444, -23.47593901973090169, -1.443836447538997980 ) ) ;
#50430 = DIRECTION ( 'NONE',  ( 1.257682986112628661E-16, 0.000000000000000000, 1.000000000000000000 ) ) ;
#50431 = DIRECTION ( 'NONE',  ( 0.000000000000000000, -0.9999999999976377785, -2.173523156925979128E-06 ) ) ;
#50432 = CARTESIAN_POINT ( 'NONE',  ( -72.51646567591126313, -23.73766607897670156, -1.055555164236458454 ) ) ;
#50433 = CARTESIAN_POINT ( 'NONE',  ( -31.62287095715007013, -24.51283580621364067, 0.6167428607019773690 ) ) ;
#50434 = ORIENTED_EDGE ( 'NONE', *, *, #8302, .T. ) ;
#50435 = ORIENTED_EDGE ( 'NONE', *, *, #9009, .F. ) ;
#50436 = CARTESIAN_POINT ( 'NONE',  ( -42.92287095715005307, -23.47596703998600276, 11.44779298504227683 ) ) ;
#50437 = DIRECTION ( 'NONE',  ( 3.773278334444167608E-23, -1.000000000000000000, 0.000000000000000000 ) ) ;
#50438 = PLANE ( 'NONE',  #89252 ) ;
#50439 = CARTESIAN_POINT ( 'NONE',  ( 6.154377932377651739, 19.64630176443789367, -1.500000000000002220 ) ) ;
#50440 = CARTESIAN_POINT ( 'NONE',  ( 8.794441374123232791, -19.68457759291379716, 11.49999999999999645 ) ) ;
#50441 = ORIENTED_EDGE ( 'NONE', *, *, #43503, .T. ) ;
#50442 = FACE_OUTER_BOUND ( 'NONE', #3208, .T. ) ;
#50443 = CARTESIAN_POINT ( 'NONE',  ( 6.853365600657045142, -5.876774720514416295, 20.20310688689519196 ) ) ;
#50444 = DIRECTION ( 'NONE',  ( 0.000000000000000000, 2.173523156925980399E-06, -0.9999999999976378895 ) ) ;
#50445 = CARTESIAN_POINT ( 'NONE',  ( 11.81759748825469281, -18.92407201980706333, 11.49999999999998934 ) ) ;
#50446 = CARTESIAN_POINT ( 'NONE',  ( 29.70220533433691301, -3.316774720514426456, 28.20564067601639735 ) ) ;
#50447 = DIRECTION ( 'NONE',  ( 3.773278334444166432E-23, -1.000000000000000000, 0.000000000000000000 ) ) ;
#50448 = ORIENTED_EDGE ( 'NONE', *, *, #81764, .F. ) ;
#50449 = LINE ( 'NONE', #88513, #20925 ) ;
#50450 = DIRECTION ( 'NONE',  ( -0.000000000000000000, 2.173523156925979552E-06, -0.9999999999976378895 ) ) ;
#50451 = B_SPLINE_CURVE_WITH_KNOTS ( 'NONE', 3,
 ( #4257, #98579, #43812, #20956 ),
 .UNSPECIFIED., .F., .F.,
 ( 4, 4 ),
 ( 0.000000000000000000, 1.000000000000000000 ),
 .UNSPECIFIED. ) ;
#50452 = CARTESIAN_POINT ( 'NONE',  ( 8.688630223215852766, -18.96179456382524364, -1.500000000000002220 ) ) ;
#50453 = VERTEX_POINT ( 'NONE', #27955 ) ;
#50455 = VERTEX_POINT ( 'NONE', #11233 ) ;
#50454 = DIRECTION ( 'NONE',  ( 1.000000000000000000, 0.000000000000000000, 0.000000000000000000 ) ) ;
#50456 = VERTEX_POINT ( 'NONE', #88869 ) ;
#50457 = CARTESIAN_POINT ( 'NONE',  ( -50.60306404051401330, -25.30220920115066008, 4.715819228956954490 ) ) ;
#50458 = CARTESIAN_POINT ( 'NONE',  ( 16.02493003730957000, -13.65669227992738577, -1.500000000000002220 ) ) ;
#50459 = VERTEX_POINT ( 'NONE', #43193 ) ;
#50460 = DIRECTION ( 'NONE',  ( -0.3133898629642195011, 5.365801633547207373E-16, 0.9496245541219264785 ) ) ;
#50462 = EDGE_CURVE ( 'NONE', #83385, #62297, #76986, .T. ) ;
#50461 = CARTESIAN_POINT ( 'NONE',  ( 29.73860345376319003, 5.356774720496559894, 19.84760796525321780 ) ) ;
#50463 = DIRECTION ( 'NONE',  ( 0.000000000000000000, -0.9999999999976377785, -2.173523156925979128E-06 ) ) ;
#50464 = EDGE_CURVE ( 'NONE', #74711, #46787, #12828, .T. ) ;
#50465 = CARTESIAN_POINT ( 'NONE',  ( -76.50805816305593510, -24.15620529776628089, 10.23563542870660470 ) ) ;
#50466 = DIRECTION ( 'NONE',  ( -3.773278334453079030E-23, 0.9999999999976377785, 2.173523156925979128E-06 ) ) ;
#50467 = CARTESIAN_POINT ( 'NONE',  ( -4.559408409702599307, -21.23122434433648209, -1.500000000000002220 ) ) ;
#50468 = CARTESIAN_POINT ( 'NONE',  ( -48.52287095715006160, -24.64965694238574656, 8.947790433994203596 ) ) ;
#50470 = ORIENTED_EDGE ( 'NONE', *, *, #14073, .T. ) ;
#50469 = CARTESIAN_POINT ( 'NONE',  ( -13.35739915041183323, 17.77566839534079435, 11.49999999999999645 ) ) ;
#50471 = CARTESIAN_POINT ( 'NONE',  ( -51.27521478229555640, -25.31441802849524692, 5.568540164726730524 ) ) ;
#50472 = CARTESIAN_POINT ( 'NONE',  ( 6.853365600657045142, -6.376774720514415407, 20.20310688689519196 ) ) ;
#50473 = CARTESIAN_POINT ( 'NONE',  ( -36.58953762381672448, -23.48786465467240347, 11.44779295918255180 ) ) ;
#50474 = ORIENTED_EDGE ( 'NONE', *, *, #67636, .T. ) ;
#50475 = ADVANCED_FACE ( 'NONE', ( #18838 ), #28950, .T. ) ;
#50476 = ADVANCED_FACE ( 'NONE', ( #20322 ), #20825, .T. ) ;
#50478 = ORIENTED_EDGE ( 'NONE', *, *, #68739, .F. ) ;
#50477 = CARTESIAN_POINT ( 'NONE',  ( -50.38191529551148307, -25.12049752546737835, 2.832404795212222659 ) ) ;
#50479 = ORIENTED_EDGE ( 'NONE', *, *, #1684, .F. ) ;
#50480 = DIRECTION ( 'NONE',  ( 0.000000000000000000, -1.000000000000000000, 0.000000000000000000 ) ) ;
#50481 = VECTOR ( 'NONE', #60138, 1000.000000000000227 ) ;
#50482 = DIRECTION ( 'NONE',  ( -3.773278334453079030E-23, 0.9999999999976377785, 2.173523156925979128E-06 ) ) ;
#50483 = DIRECTION ( 'NONE',  ( -0.000000000000000000, -0.000000000000000000, -1.000000000000000000 ) ) ;
#50484 = EDGE_CURVE ( 'NONE', #58811, #31528, #35859, .T. ) ;
#50485 = CARTESIAN_POINT ( 'NONE',  ( 31.64143112576189765, 6.376774720514426953, 14.03360796525321774 ) ) ;
#50486 = ORIENTED_EDGE ( 'NONE', *, *, #38135, .T. ) ;
#50487 = CARTESIAN_POINT ( 'NONE',  ( -130.5728709571500872, -24.40567238644092640, 9.892971901584807881 ) ) ;
#50488 = CARTESIAN_POINT ( 'NONE',  ( -21.13723655771239152, -7.639886366525781014, -1.500000000000002220 ) ) ;
#50489 = VERTEX_POINT ( 'NONE', #26955 ) ;
#50490 = CARTESIAN_POINT ( 'NONE',  ( -124.6228709571500559, -29.50248528299804818, 1.056150453629045360 ) ) ;
#50491 = PLANE ( 'NONE',  #510 ) ;
#50492 = CARTESIAN_POINT ( 'NONE',  ( 6.190876379677949792, 3.316774720513832708, -27.38145114071290465 ) ) ;
#50493 = CARTESIAN_POINT ( 'NONE',  ( -116.5228709571500474, -24.50216790748204332, 0.6166512839542594993 ) ) ;
#50494 = CARTESIAN_POINT ( 'NONE',  ( -30.59464630539410734, -24.75152770810919378, 1.363349870542269082 ) ) ;
#50495 = CARTESIAN_POINT ( 'NONE',  ( 19.59400933563812330, 0.1774559437341752532, 11.49999999999998934 ) ) ;
#50496 = CARTESIAN_POINT ( 'NONE',  ( -50.33461658617051171, -25.31263903432395779, 4.734677650700013452 ) ) ;
#50498 = EDGE_LOOP ( 'NONE', ( #15903, #94486, #80415 ) ) ;
#50497 = APPROVAL_PERSON_ORGANIZATION ( #52124, #56303, #13043 ) ;
#50499 = CARTESIAN_POINT ( 'NONE',  ( -10.32266838563235467, 18.89866041204108527, -1.500000000000002220 ) ) ;
#50500 = PLANE ( 'NONE',  #7410 ) ;
#50501 = CARTESIAN_POINT ( 'NONE',  ( -71.30218710724507503, -25.25639427085534905, 6.299238331127512858 ) ) ;
#50502 = CARTESIAN_POINT ( 'NONE',  ( -50.52287095715006160, -24.91544648472626022, 1.928969306349430868 ) ) ;
#50503 = CARTESIAN_POINT ( 'NONE',  ( -70.35895856474229504, -25.31161946917133321, 5.313173610579343453 ) ) ;
#50504 = CARTESIAN_POINT ( 'NONE',  ( -19.49525799874905729, 12.17417675796824561, -1.500000000000002220 ) ) ;
#50505 = PERSON_AND_ORGANIZATION ( #70597, #27821 ) ;
#50506 = CARTESIAN_POINT ( 'NONE',  ( 3.176458874063926352, -5.965225279485592225, -28.85257003503889095 ) ) ;
#50507 = CARTESIAN_POINT ( 'NONE',  ( -53.53688776224935708, -24.51314013834315730, 0.6176544820404108460 ) ) ;
#50508 = CARTESIAN_POINT ( 'NONE',  ( 17.77915467781788195, 9.360003092772107181, 11.49999999999999645 ) ) ;
#50509 = DIRECTION ( 'NONE',  ( -0.1254312216594016538, -0.000000000000000000, -0.9921023176230513441 ) ) ;
#50510 = DIRECTION ( 'NONE',  ( 0.000000000000000000, 0.000000000000000000, -1.000000000000000000 ) ) ;
#50511 = LINE ( 'NONE', #41917, #21395 ) ;
#50512 = CARTESIAN_POINT ( 'NONE',  ( 13.86067930709089602, 5.152774720507880879, -28.23766061414428208 ) ) ;
#50513 = CARTESIAN_POINT ( 'NONE',  ( 14.73162737928355170, 2.682774720514426559, -27.37940951657878941 ) ) ;
#50514 = CARTESIAN_POINT ( 'NONE',  ( -9.893332137849947472, -17.22304987741864579, -1.500000000000002220 ) ) ;
#50515 = CARTESIAN_POINT ( 'NONE',  ( -113.5165029720520238, -24.34968618360933945, 0.1864209137778880254 ) ) ;
#50516 = CARTESIAN_POINT ( 'NONE',  ( 7.987771016649366729, -18.01272016045900415, -1.500000000000002220 ) ) ;
#50517 = EDGE_CURVE ( 'NONE', #64861, #45470, #68560, .T. ) ;
#50518 = CARTESIAN_POINT ( 'NONE',  ( -75.55620429048340725, -23.48786465467241058, 11.44779295918255180 ) ) ;
#50519 = DATE_AND_TIME ( #72368, #78063 ) ;
#50520 = CARTESIAN_POINT ( 'NONE',  ( -115.6228709571500559, -23.47593901973091235, -1.443836447538997536 ) ) ;
#50521 = CARTESIAN_POINT ( 'NONE',  ( -111.5228709571500616, -24.34917612406837151, 0.1852690917426604855 ) ) ;
#50522 = CARTESIAN_POINT ( 'NONE',  ( 13.11803791274172681, -15.88952355948706341, 11.49999999999999645 ) ) ;
#50523 = EDGE_CURVE ( 'NONE', #94249, #13162, #42701, .T. ) ;
#50524 = CARTESIAN_POINT ( 'NONE',  ( -121.5228709571500616, -24.65952944569305316, 1.056160979905705899 ) ) ;
#50525 = B_SPLINE_CURVE_WITH_KNOTS ( 'NONE', 3,
 ( #56953, #87887, #11259, #88895 ),
 .UNSPECIFIED., .F., .F.,
 ( 4, 4 ),
 ( 0.000000000000000000, 9.999999999998897304E-05 ),
 .UNSPECIFIED. ) ;
#50526 = CARTESIAN_POINT ( 'NONE',  ( -12.01393383709116947, -19.22582291892495121, 11.49999999999999645 ) ) ;
#50527 = AXIS2_PLACEMENT_3D ( 'NONE', #82161, #82658, #36986 ) ;
#50528 = ORIENTED_EDGE ( 'NONE', *, *, #87246, .F. ) ;
#50529 = EDGE_CURVE ( 'NONE', #84514, #97228, #27418, .T. ) ;
#50530 = CARTESIAN_POINT ( 'NONE',  ( -126.5895376238167245, -23.47593901973091235, -1.443836447538995760 ) ) ;
#50531 = LINE ( 'NONE', #89094, #58198 ) ;
#50532 = B_SPLINE_CURVE_WITH_KNOTS ( 'NONE', 3,
 ( #82688, #13169, #60870, #91795 ),
 .UNSPECIFIED., .F., .F.,
 ( 4, 4 ),
 ( 0.000000000000000000, 9.999999999997510880E-05 ),
 .UNSPECIFIED. ) ;
#50533 = CARTESIAN_POINT ( 'NONE',  ( -111.9545715455114987, -25.05712135967895193, 7.447789548357302891 ) ) ;
#50534 = PLANE ( 'NONE',  #65846 ) ;
#50535 = VERTEX_POINT ( 'NONE', #43682 ) ;
#50536 = ORIENTED_EDGE ( 'NONE', *, *, #19771, .T. ) ;
#50537 = LINE ( 'NONE', #27704, #76037 ) ;
#50538 = CARTESIAN_POINT ( 'NONE',  ( -22.79553223295561892, 1.966428799096173075, 11.49999999999998934 ) ) ;
#50539 = CARTESIAN_POINT ( 'NONE',  ( -91.62287095715004170, -29.50250243563736774, 8.947779886222139822 ) ) ;
#50540 = CARTESIAN_POINT ( 'NONE',  ( -21.50746323947805649, 1.722430922125298247, -1.500000000000002220 ) ) ;
#50541 = PLANE ( 'NONE',  #88471 ) ;
#50542 = CARTESIAN_POINT ( 'NONE',  ( -65.52287095715006160, -24.52232992886361984, 0.6492154411906035927 ) ) ;
#50543 = CARTESIAN_POINT ( 'NONE',  ( -6.869692127560369066, -21.44495933931894527, 11.49999999999999645 ) ) ;
#50544 = ORIENTED_EDGE ( 'NONE', *, *, #23619, .T. ) ;
#50545 = FACE_OUTER_BOUND ( 'NONE', #98305, .T. ) ;
#50546 = B_SPLINE_CURVE_WITH_KNOTS ( 'NONE', 3,
 ( #85094, #45553, #93203, #76971 ),
 .UNSPECIFIED., .F., .F.,
 ( 4, 4 ),
 ( 0.000000000000000000, 9.999999999998897304E-05 ),
 .UNSPECIFIED. ) ;
#50547 = AXIS2_PLACEMENT_3D ( 'NONE', #38535, #70999, #472 ) ;
#50548 = CARTESIAN_POINT ( 'NONE',  ( 10.99670386783381737, -19.00842362925918749, 11.49999999999998934 ) ) ;
#50549 = CARTESIAN_POINT ( 'NONE',  ( -111.6303161903200305, -23.73766607897671221, -1.055555164236450905 ) ) ;
#50550 = DIRECTION ( 'NONE',  ( -0.000000000000000000, 0.000000000000000000, -1.000000000000000000 ) ) ;
#50551 = ORIENTED_EDGE ( 'NONE', *, *, #79261, .F. ) ;
#50552 = DIRECTION ( 'NONE',  ( 0.000000000000000000, 1.000000000000000000, 0.000000000000000000 ) ) ;
#50553 = DIRECTION ( 'NONE',  ( -0.000000000000000000, 1.000000000000000000, -0.000000000000000000 ) ) ;
#50554 = VERTEX_POINT ( 'NONE', #73636 ) ;
#50555 = DIRECTION ( 'NONE',  ( 1.000000000000000000, 3.773278334444167608E-23, 8.201307833595939069E-29 ) ) ;
#50556 = ORIENTED_EDGE ( 'NONE', *, *, #49557, .F. ) ;
#50557 = VERTEX_POINT ( 'NONE', #5614 ) ;
#50558 = VERTEX_POINT ( 'NONE', #74621 ) ;
#50559 = CARTESIAN_POINT ( 'NONE',  ( -23.71328795744024021, 5.965225279485594001, -17.58350715675015152 ) ) ;
#50560 = CARTESIAN_POINT ( 'NONE',  ( -110.2093792378191921, -29.50249512742697888, 5.585400078537770874 ) ) ;
#50561 = CARTESIAN_POINT ( 'NONE',  ( -123.5228709571500616, -23.48786465467242479, 11.44779295918253759 ) ) ;
#50562 = CARTESIAN_POINT ( 'NONE',  ( 18.17922461840205983, -9.147185827878928421, -1.500000000000002220 ) ) ;
#50563 = ORIENTED_EDGE ( 'NONE', *, *, #33872, .F. ) ;
#50564 = ORGANIZATION ( 'NAUO-ORG13', 'UNSPECIFIED', 'UNSPECIFIED' ) ;
#50565 = CARTESIAN_POINT ( 'NONE',  ( -71.70484777582788638, -25.23825382336761081, 6.283456011705152555 ) ) ;
#50566 = CARTESIAN_POINT ( 'NONE',  ( -38.52287095715006870, -29.50247984919015209, -1.443849546365060466 ) ) ;
#50567 = EDGE_CURVE ( 'NONE', #70059, #61929, #67526, .T. ) ;
#50568 = B_SPLINE_CURVE_WITH_KNOTS ( 'NONE', 3,
 ( #97559, #35673, #51899, #27566, #60018, #36660 ),
 .UNSPECIFIED., .F., .F.,
 ( 4, 2, 4 ),
 ( 0.000000000000000000, 0.001380764517854763014, 0.002761529035709526028 ),
 .UNSPECIFIED. ) ;
#50570 = DIRECTION ( 'NONE',  ( -3.773278334453079030E-23, 0.9999999999976377785, 2.173523156925979128E-06 ) ) ;
#50569 = AXIS2_PLACEMENT_3D ( 'NONE', #65489, #34014, #26400 ) ;
#50571 = CARTESIAN_POINT ( 'NONE',  ( -71.60924725748338915, -25.25855199099994053, 6.721927571088929021 ) ) ;
#50572 = ORIENTED_EDGE ( 'NONE', *, *, #70513, .T. ) ;
#50573 = CARTESIAN_POINT ( 'NONE',  ( -28.66129012810275256, -24.76880947087198237, 2.702369889720187324 ) ) ;
#50574 = CARTESIAN_POINT ( 'NONE',  ( -97.55620429048339304, -24.66019654487200086, 8.947790411086128159 ) ) ;
#50575 = LOCAL_TIME ( 0, 54, 15.00000000000000000, #35784 ) ;
#50576 = ORIENTED_EDGE ( 'NONE', *, *, #60941, .T. ) ;
#50577 = CARTESIAN_POINT ( 'NONE',  ( -20.31193019649481357, 4.361987795224258946, -1.500000000000002220 ) ) ;
#50578 = ORIENTED_EDGE ( 'NONE', *, *, #17717, .T. ) ;
#50580 = ORIENTED_EDGE ( 'NONE', *, *, #72369, .F. ) ;
#50579 = FACE_OUTER_BOUND ( 'NONE', #63214, .T. ) ;
#50581 = CARTESIAN_POINT ( 'NONE',  ( 8.978253834636468866, -5.876774720514426953, 0.000000000000000000 ) ) ;
#50582 = FACE_OUTER_BOUND ( 'NONE', #23960, .T. ) ;
#50583 = VERTEX_POINT ( 'NONE', #28442 ) ;
#50584 = VERTEX_POINT ( 'NONE', #98448 ) ;
#50585 = CARTESIAN_POINT ( 'NONE',  ( -29.49875734969025842, -5.965225279485572685, 15.62202280011862321 ) ) ;
#50586 = EDGE_CURVE ( 'NONE', #26032, #83737, #21322, .T. ) ;
#50587 = CARTESIAN_POINT ( 'NONE',  ( 10.46399479596398052, 3.316774720514422903, -27.03001098546561209 ) ) ;
#50588 = CARTESIAN_POINT ( 'NONE',  ( -86.52287095715009002, -24.33832256527048798, 0.1851278514138618714 ) ) ;
#50589 = CARTESIAN_POINT ( 'NONE',  ( -43.51355794557933621, -23.73791477778911130, 11.05961554403171121 ) ) ;
#50591 = ORIENTED_EDGE ( 'NONE', *, *, #25289, .T. ) ;
#50590 = CARTESIAN_POINT ( 'NONE',  ( -17.20036718215007099, 13.84871166177648583, 11.49999999999999645 ) ) ;
#50592 = CARTESIAN_POINT ( 'NONE',  ( -108.5121574744787267, -24.65952944569305316, 1.056160979905706121 ) ) ;
#50593 = EDGE_CURVE ( 'NONE', #88484, #33442, #86707, .T. ) ;
#50594 = CARTESIAN_POINT ( 'NONE',  ( -21.91535228782390732, -5.629186751109307885, 11.49999999999998934 ) ) ;
#50595 = ADVANCED_FACE ( 'NONE', ( #30947 ), #45683, .F. ) ;
#50597 = VERTEX_POINT ( 'NONE', #61914 ) ;
#50596 = CARTESIAN_POINT ( 'NONE',  ( -115.5149135104634439, -24.73531770709096023, 8.716586749053508498 ) ) ;
#50598 = EDGE_CURVE ( 'NONE', #31243, #57287, #6111, .T. ) ;
#50599 = ORIENTED_EDGE ( 'NONE', *, *, #99793, .T. ) ;
#50600 = EDGE_CURVE ( 'NONE', #91623, #39871, #26144, .T. ) ;
#50601 = DIRECTION ( 'NONE',  ( 0.000000000000000000, -1.000000000000000000, 0.000000000000000000 ) ) ;
#50602 = VECTOR ( 'NONE', #16514, 1000.000000000000114 ) ;
#50603 = CARTESIAN_POINT ( 'NONE',  ( -57.53785648602210046, -24.51419770103157703, 9.386484678747175181 ) ) ;
#50604 = VERTEX_POINT ( 'NONE', #3 ) ;
#50605 = CARTESIAN_POINT ( 'NONE',  ( 7.804836024166685426, 19.70032748343534834, -1.500000000000002220 ) ) ;
#50606 = CARTESIAN_POINT ( 'NONE',  ( 32.84232313084854837, 4.840274619473185602, -11.71291885348858663 ) ) ;
#50607 = CARTESIAN_POINT ( 'NONE',  ( -80.62287095715004170, -23.48786465467241058, 11.44779295918254469 ) ) ;
#50608 = CARTESIAN_POINT ( 'NONE',  ( 18.98964132805693694, -11.70494588174365092, -1.500000000000002220 ) ) ;
#50609 = CARTESIAN_POINT ( 'NONE',  ( 7.526024287269984292, 1.682774720514426114, 9.032262774691707463 ) ) ;
#50610 = ADVANCED_FACE ( 'NONE', ( #7613 ), #85233, .F. ) ;
#50611 = ORIENTED_EDGE ( 'NONE', *, *, #33507, .T. ) ;
#50612 = CARTESIAN_POINT ( 'NONE',  ( -125.5228709571500616, -29.50247984919015209, -1.443849546365044922 ) ) ;
#50613 = FACE_OUTER_BOUND ( 'NONE', #38991, .T. ) ;
#50614 = LINE ( 'NONE', #49629, #57718 ) ;
#50615 = DIRECTION ( 'NONE',  ( -0.000000000000000000, 1.000000000000000000, -0.000000000000000000 ) ) ;
#50616 = CARTESIAN_POINT ( 'NONE',  ( -16.16875682573952133, 10.94412424577950915, -1.500000000000002220 ) ) ;
#50617 = AXIS2_PLACEMENT_3D ( 'NONE', #85694, #24293, #32408 ) ;
#50618 = CARTESIAN_POINT ( 'NONE',  ( -19.34459864454321831, 9.218434461607088792, 11.49999999999998934 ) ) ;
#50619 = CARTESIAN_POINT ( 'NONE',  ( -26.72449842520168062, -24.57999555349612208, 1.897194066446994620 ) ) ;
#50620 = AXIS2_PLACEMENT_3D ( 'NONE', #79841, #12323, #95573 ) ;
#50621 = CARTESIAN_POINT ( 'NONE',  ( -2.169994883066378222, 10.75358048763950869, 0.000000000000000000 ) ) ;
#50622 = PLANE ( 'NONE',  #24923 ) ;
#50623 = CARTESIAN_POINT ( 'NONE',  ( -19.58686714514938387, 11.73587220785771379, -1.500000000000002220 ) ) ;
#50624 = CARTESIAN_POINT ( 'NONE',  ( 6.965660145040495391E-18, 1.826774720514430905, -5.724587470723507785E-18 ) ) ;
#50625 = CARTESIAN_POINT ( 'NONE',  ( -102.5870889699518216, -24.51314013834316086, 0.6176544820404232805 ) ) ;
#50626 = LINE ( 'NONE', #50133, #16806 ) ;
#50627 = CARTESIAN_POINT ( 'NONE',  ( -1.345660788846553935, -19.86331345790170033, 11.49999999999999645 ) ) ;
#50628 = CARTESIAN_POINT ( 'NONE',  ( -104.5551282687516448, -23.96119346886880663, -0.6495511937832033622 ) ) ;
#50629 = CARTESIAN_POINT ( 'NONE',  ( -89.40841769935769889, -25.27880950044345809, 5.947789066509453271 ) ) ;
#50630 = CARTESIAN_POINT ( 'NONE',  ( -48.65307323584794119, -23.73766607897670866, -1.055555164236436250 ) ) ;
#50631 = ORIENTED_EDGE ( 'NONE', *, *, #91943, .F. ) ;
#50632 = FACE_OUTER_BOUND ( 'NONE', #25212, .T. ) ;
#50633 = EDGE_CURVE ( 'NONE', #56283, #46259, #31474, .T. ) ;
#50634 = CARTESIAN_POINT ( 'NONE',  ( -32.40922458005066176, -25.16370864782812689, 7.203858152271859439 ) ) ;
#50635 = CARTESIAN_POINT ( 'NONE',  ( 21.03555826204448209, -5.341079136732027166, 11.49999999999998934 ) ) ;
#50636 = CARTESIAN_POINT ( 'NONE',  ( -3.302878749216429544, 14.80319218833827044, 8.673617379884035472E-16 ) ) ;
#50637 = CARTESIAN_POINT ( 'NONE',  ( -15.85469643196389278, -11.46343829903102396, -1.500000000000002220 ) ) ;
#50638 = CARTESIAN_POINT ( 'NONE',  ( -55.60865192297863757, -23.85049219812685806, 10.88485053497527133 ) ) ;
#50639 = EDGE_CURVE ( 'NONE', #56586, #20842, #7911, .T. ) ;
#50640 = VECTOR ( 'NONE', #12911, 1000.000000000000000 ) ;
#50641 = B_SPLINE_CURVE_WITH_KNOTS ( 'NONE', 3,
 ( #83584, #74483, #6474, #45544, #61277, #5968, #99790, #37427 ),
 .UNSPECIFIED., .F., .F.,
 ( 4, 2, 2, 4 ),
 ( 6.384118678608731864E-06, 0.002007151183507255819, 0.003007534715921579473, 0.004007918248335902260 ),
 .UNSPECIFIED. ) ;
#50642 = DATE_AND_TIME ( #78192, #55494 ) ;
#50643 = LOCAL_TIME ( 0, 54, 15.00000000000000000, #46258 ) ;
#50644 = DIRECTION ( 'NONE',  ( 0.000000000000000000, 0.000000000000000000, -1.000000000000000000 ) ) ;
#50645 = CARTESIAN_POINT ( 'NONE',  ( -19.95082702767638239, -4.354873812894156870, 11.49999999999999645 ) ) ;
#50646 = CARTESIAN_POINT ( 'NONE',  ( -50.11049603129085739, -25.30358447871552841, 5.223373167154639063 ) ) ;
#50647 = B_SPLINE_CURVE_WITH_KNOTS ( 'NONE', 3,
 ( #96305, #4954, #2973, #89691 ),
 .UNSPECIFIED., .F., .F.,
 ( 4, 4 ),
 ( 0.7310220049200362169, 0.7400284361921516396 ),
 .UNSPECIFIED. ) ;
#50648 = FACE_OUTER_BOUND ( 'NONE', #82654, .T. ) ;
#50649 = AXIS2_PLACEMENT_3D ( 'NONE', #70968, #40008, #84677 ) ;
#50650 = ORIENTED_EDGE ( 'NONE', *, *, #76895, .T. ) ;
#50651 = EDGE_CURVE ( 'NONE', #16488, #3436, #98953, .T. ) ;
#50652 = LINE ( 'NONE', #34925, #31364 ) ;
#50653 = LINE ( 'NONE', #73485, #99521 ) ;
#50654 = CARTESIAN_POINT ( 'NONE',  ( 2.021814659504407579E-13, -19.30000000000000426, -1.500000000000002220 ) ) ;
#50655 = AXIS2_PLACEMENT_3D ( 'NONE', #40719, #17377, #9764 ) ;
#50656 = ADVANCED_FACE ( 'NONE', ( #92342 ), #92123, .T. ) ;
#50657 = CARTESIAN_POINT ( 'NONE',  ( -109.5138115999294968, -24.51314013834315375, 0.6176544820404177294 ) ) ;
#50658 = VERTEX_POINT ( 'NONE', #2019 ) ;
#50659 = DIRECTION ( 'NONE',  ( 1.000000000000000000, 3.773278334444166432E-23, 8.201307841325785021E-29 ) ) ;
#50660 = CARTESIAN_POINT ( 'NONE',  ( 10.47623847176155820, -20.49086732513842080, 11.49999999999999645 ) ) ;
#50661 = CARTESIAN_POINT ( 'NONE',  ( -17.61067154241388977, 14.45706175128816184, -1.500000000000002220 ) ) ;
#50662 = CARTESIAN_POINT ( 'NONE',  ( -70.34543693012690824, -25.04307398257883577, 7.563174194274490780 ) ) ;
#50663 = B_SPLINE_SURFACE_WITH_KNOTS ( 'NONE', 3, 1, ( 
 ( #44285, #5705 ),
 ( #75214, #7196 ),
 ( #69098, #30539 ),
 ( #53889, #8213 ),
 ( #24927, #71620 ),
 ( #93938, #47279 ),
 ( #17828, #39151 ),
 ( #86828, #70108 ),
 ( #16316, #79213 ),
 ( #31538, #71118 ),
 ( #77698, #2116 ),
 ( #79717, #64536 ),
 ( #23926, #40163 ),
 ( #62502, #33551 ),
 ( #10213, #93431 ) ),
 .UNSPECIFIED., .F., .F., .F.,
 ( 4, 1, 1, 1, 1, 1, 1, 1, 1, 1, 1, 1, 4 ),
 ( 2, 2 ),
 ( 0.000000000000000000, 0.09025424934267306520, 0.1785397915286855430, 0.2660930338538194384, 0.3546309779571704679, 0.4418861533505633599, 0.5257469151636473548, 0.6081136336036379042, 0.6901972728278812363, 0.7708214843303337060, 0.8483261812554098169, 0.9240117400247429558, 0.9999999999999998890 ),
 ( 0.000000000000000000, 1.000000000000000000 ),
 .UNSPECIFIED. ) ;
#50664 = CARTESIAN_POINT ( 'NONE',  ( -40.52287095715009002, -24.91544648472626022, 1.928969306349431756 ) ) ;
#50665 = FACE_OUTER_BOUND ( 'NONE', #98440, .T. ) ;
#50666 = CARTESIAN_POINT ( 'NONE',  ( -54.52287095715004739, -23.96127896941631619, -0.6493128931038086860 ) ) ;
#50667 = CARTESIAN_POINT ( 'NONE',  ( -89.52287095715010423, -24.34917612407033616, 0.1852690917477812227 ) ) ;
#50668 = CARTESIAN_POINT ( 'NONE',  ( -21.73523922981167189, -2.474665994198115726, 11.49999999999998934 ) ) ;
#50669 = CC_DESIGN_PERSON_AND_ORGANIZATION_ASSIGNMENT ( #17932, #94545, ( #29568 ) ) ;
#50670 = CARTESIAN_POINT ( 'NONE',  ( -0.1426030150137701236, -21.20389190742571373, -1.497999999999532594 ) ) ;
#50671 = AXIS2_PLACEMENT_3D ( 'NONE', #65, #91903, #85805 ) ;
#50672 = DIRECTION ( 'NONE',  ( -1.000000000000000000, 0.000000000000000000, 0.000000000000000000 ) ) ;
#50673 = CARTESIAN_POINT ( 'NONE',  ( -71.70647227915280553, -25.25299663069663936, 6.133628806981914927 ) ) ;
#50674 = LINE ( 'NONE', #81620, #32317 ) ;
#50675 = ORIENTED_EDGE ( 'NONE', *, *, #15700, .T. ) ;
#50676 = PRODUCT ( 'Tape Measure Hook', 'Tape Measure Hook', '', ( #79949 ) ) ;
#50677 = CARTESIAN_POINT ( 'NONE',  ( -12.60687543931603471, -16.05746371069360379, -1.500000000000002220 ) ) ;
#50678 = VERTEX_POINT ( 'NONE', #32454 ) ;
#50679 = ORIENTED_EDGE ( 'NONE', *, *, #68734, .F. ) ;
#50680 = ORIENTED_EDGE ( 'NONE', *, *, #59886, .T. ) ;
#50681 = VERTEX_POINT ( 'NONE', #2517 ) ;
#50682 = CARTESIAN_POINT ( 'NONE',  ( -13.44081803467414638, 18.71018530922267686, 11.49999999999998934 ) ) ;
#50683 = CARTESIAN_POINT ( 'NONE',  ( 29.70220533433691301, -6.376774720514426953, 28.20564067601639735 ) ) ;
#50684 = CARTESIAN_POINT ( 'NONE',  ( -6.497366621441947210, -19.08602653180391329, -1.500000000000002220 ) ) ;
#50685 = VERTEX_POINT ( 'NONE', #3021 ) ;
#50686 = FACE_OUTER_BOUND ( 'NONE', #96449, .T. ) ;
#50687 = CARTESIAN_POINT ( 'NONE',  ( -91.62287095715004170, -29.50248528299804818, 1.056150453629040253 ) ) ;
#50688 = CARTESIAN_POINT ( 'NONE',  ( -95.58939892478511524, -24.52300882791530512, 0.6510814631126408125 ) ) ;
#50689 = CARTESIAN_POINT ( 'NONE',  ( -41.62287095715006302, -23.72773821059535493, 11.05748984161097503 ) ) ;
#50691 = ORIENTED_EDGE ( 'NONE', *, *, #79919, .T. ) ;
#50690 = CARTESIAN_POINT ( 'NONE',  ( 8.370372042246325250, 19.68514866842044242, 11.49999999999999645 ) ) ;
#50692 = CARTESIAN_POINT ( 'NONE',  ( -24.90875734969025501, -5.965225279485572685, 19.84760796525321780 ) ) ;
#50693 = CIRCLE ( 'NONE', #57233, 4.450000000000000178 ) ;
#50694 = ORIENTED_EDGE ( 'NONE', *, *, #9694, .T. ) ;
#50695 = CARTESIAN_POINT ( 'NONE',  ( 22.20168578472828358, 1.497490109320031682, -1.500000000000002220 ) ) ;
#50696 = CARTESIAN_POINT ( 'NONE',  ( 20.35908867758196550, 3.722869731652943770, -1.500000000000002220 ) ) ;
#50697 = VERTEX_POINT ( 'NONE', #62414 ) ;
#50698 = LINE ( 'NONE', #81647, #59923 ) ;
#50699 = VERTEX_POINT ( 'NONE', #39569 ) ;
#50700 = CARTESIAN_POINT ( 'NONE',  ( -81.52287095715010423, -23.48783264083388289, -1.443836473375922580 ) ) ;
#50701 = VERTEX_POINT ( 'NONE', #62928 ) ;
#50702 = CARTESIAN_POINT ( 'NONE',  ( 9.069233782100962316, -3.316774720514428232, -28.07145878873749112 ) ) ;
#50703 = CARTESIAN_POINT ( 'NONE',  ( 0.7041596644206948863, -20.94928778062849162, -1.500000000000002220 ) ) ;
#50704 = EDGE_CURVE ( 'NONE', #49734, #44058, #87715, .T. ) ;
#50705 = CARTESIAN_POINT ( 'NONE',  ( -5.132426408838210108, -21.30661980433056968, 11.49999999999999645 ) ) ;
#50706 = CARTESIAN_POINT ( 'NONE',  ( -26.38306202989770455, -24.89279797102699732, 6.654069566590164797 ) ) ;
#50707 = CARTESIAN_POINT ( 'NONE',  ( 8.356338879324495039, -20.90460381316865934, -1.500000000000002220 ) ) ;
#50708 = CARTESIAN_POINT ( 'NONE',  ( 20.71091302404612833, 3.140364381853995912, -1.500000000000002220 ) ) ;
#50709 = CARTESIAN_POINT ( 'NONE',  ( -38.48005118028396510, -24.65952944569304606, 1.056160979905694131 ) ) ;
#50710 = CARTESIAN_POINT ( 'NONE',  ( 5.771117285127500551, -6.376774720514417183, 20.39900056875960388 ) ) ;
#50711 = CARTESIAN_POINT ( 'NONE',  ( -119.5171998032949432, -24.66019654487200441, 8.947790411086108620 ) ) ;
#50712 = VECTOR ( 'NONE', #30276, 1000.000000000000000 ) ;
#50713 = CARTESIAN_POINT ( 'NONE',  ( -32.08503310962682065, -24.87219037988794312, 1.747789950295618899 ) ) ;
#50714 = ORIENTED_EDGE ( 'NONE', *, *, #64488, .F. ) ;
#50715 = ORGANIZATION ( 'NAUO-ORG5', 'UNSPECIFIED', 'UNSPECIFIED' ) ;
#50716 = ADVANCED_FACE ( 'NONE', ( #41582 ), #9114, .F. ) ;
#50717 = ORIENTED_EDGE ( 'NONE', *, *, #39792, .T. ) ;
#50718 = VERTEX_POINT ( 'NONE', #78606 ) ;
#50719 = ADVANCED_FACE ( 'NONE', ( #94347 ), #16721, .T. ) ;
#50720 = CARTESIAN_POINT ( 'NONE',  ( -52.57794712450625951, -24.65952944569304606, 1.056160979905696573 ) ) ;
#50721 = EDGE_LOOP ( 'NONE', ( #71209, #55024, #8094, #1985 ) ) ;
#50722 = CARTESIAN_POINT ( 'NONE',  ( 20.90071823198991297, 5.034746273075951351, -1.500000000000002220 ) ) ;
#50723 = AXIS2_PLACEMENT_3D ( 'NONE', #15182, #84693, #46146 ) ;
#50724 = CARTESIAN_POINT ( 'NONE',  ( -28.52287095715005805, -23.31185441368106126, 11.44779303854528685 ) ) ;
#50725 = ORIENTED_EDGE ( 'NONE', *, *, #98497, .T. ) ;
#50726 = CARTESIAN_POINT ( 'NONE',  ( -18.71117167593497399, 9.704403692310313190, -1.500000000000002220 ) ) ;
#50727 = CARTESIAN_POINT ( 'NONE',  ( -92.58953762381672448, -24.64965694238407323, 8.947790433994651238 ) ) ;
#50728 = CARTESIAN_POINT ( 'NONE',  ( -52.62287095715004881, -23.73907113216990439, -1.053371485793232143 ) ) ;
#50729 = CARTESIAN_POINT ( 'NONE',  ( -50.54314373887315526, -24.40133493613049609, 9.663955038902804162 ) ) ;
#50730 = CARTESIAN_POINT ( 'NONE',  ( -101.5853492316966822, -24.65952944569305316, 1.056160979905706121 ) ) ;
#50731 = CARTESIAN_POINT ( 'NONE',  ( -109.3648162840242293, -25.29802075622466262, 4.345455213388392579 ) ) ;
#50732 = CARTESIAN_POINT ( 'NONE',  ( -13.58966412916292299, 17.40808962483262690, -1.500000000000002220 ) ) ;
#50733 = VECTOR ( 'NONE', #45588, 1000.000000000000000 ) ;
#50734 = ORIENTED_EDGE ( 'NONE', *, *, #51149, .T. ) ;
#50735 = CARTESIAN_POINT ( 'NONE',  ( -116.5876151828773999, -24.65952944569305316, 1.056160979905712560 ) ) ;
#50736 = EDGE_CURVE ( 'NONE', #65047, #66631, #39364, .T. ) ;
#50737 = B_SPLINE_CURVE_WITH_KNOTS ( 'NONE', 3,
 ( #40650, #71600, #56387, #70086, #85302, #87309 ),
 .UNSPECIFIED., .F., .F.,
 ( 4, 2, 4 ),
 ( 0.000000000000000000, 0.001380901958385389412, 0.002761803916770778824 ),
 .UNSPECIFIED. ) ;
#50738 = CARTESIAN_POINT ( 'NONE',  ( -108.9573313204422647, -25.28251216705303150, 4.249596787124276354 ) ) ;
#50739 = CARTESIAN_POINT ( 'NONE',  ( -41.84702555354165554, -25.31624510665928796, 4.480638910303021305 ) ) ;
#50740 = CARTESIAN_POINT ( 'NONE',  ( -62.53909850713881724, -24.51419770103156281, 9.386484678747184063 ) ) ;
#50741 = FACE_OUTER_BOUND ( 'NONE', #33570, .T. ) ;
#50742 = CARTESIAN_POINT ( 'NONE',  ( 21.34331307443176584, 0.5271963136488534429, 11.49999999999998934 ) ) ;
#50743 = CARTESIAN_POINT ( 'NONE',  ( -26.12992370186784896, -24.95752881727359096, 5.611782011825503957 ) ) ;
#50744 = FACE_OUTER_BOUND ( 'NONE', #19098, .T. ) ;
#50745 = B_SPLINE_CURVE_WITH_KNOTS ( 'NONE', 3,
 ( #7710, #1109, #8723, #38152, #7203, #32051 ),
 .UNSPECIFIED., .F., .F.,
 ( 4, 2, 4 ),
 ( 0.000000000000000000, 0.001380764517854766050, 0.002761529035709532100 ),
 .UNSPECIFIED. ) ;
#50746 = CARTESIAN_POINT ( 'NONE',  ( -84.58953762381672448, -24.66019654487199730, 8.947790411086112172 ) ) ;
#50747 = FACE_OUTER_BOUND ( 'NONE', #48851, .T. ) ;
#50748 = CARTESIAN_POINT ( 'NONE',  ( -17.75566480456612695, 14.03706703302619374, -1.500000000000002220 ) ) ;
#50749 = B_SPLINE_SURFACE_WITH_KNOTS ( 'NONE', 3, 3, ( 
 ( #25040, #71231, #70227, #39266 ),
 ( #30663, #15924, #706, #93543 ),
 ( #62624, #24038, #54504, #84941 ),
 ( #17433, #1719, #23024, #78814 ),
 ( #32656, #48394, #47393, #61632 ),
 ( #77319, #46387, #63633, #85949 ),
 ( #63128, #9311, #62124, #56015 ) ),
 .UNSPECIFIED., .F., .F., .F.,
 ( 4, 3, 4 ),
 ( 4, 4 ),
 ( 0.0004766839783830419445, 0.1029713700210903166, 0.2054660560637975864 ),
 ( 0.009496412973245757505, 0.01051351915677940785 ),
 .UNSPECIFIED. ) ;
#50750 = CARTESIAN_POINT ( 'NONE',  ( -65.52287095715006160, -24.99156044556202616, 7.747789690856173195 ) ) ;
#50751 = ORIENTED_EDGE ( 'NONE', *, *, #74622, .F. ) ;
#50752 = CARTESIAN_POINT ( 'NONE',  ( -35.62287095715007013, -24.92604778743017491, 8.074972756849351896 ) ) ;
#50753 = CARTESIAN_POINT ( 'NONE',  ( 25.61870917940689196, 0.3587747205144265483, 29.49402280011862487 ) ) ;
#50754 = CARTESIAN_POINT ( 'NONE',  ( 10.86211995951333620, 16.47970581058804740, 11.49999999999999645 ) ) ;
#50755 = DIRECTION ( 'NONE',  ( 1.000000000000000000, 0.000000000000000000, 0.000000000000000000 ) ) ;
#50756 = CARTESIAN_POINT ( 'NONE',  ( -32.07722060962680644, -25.10952229683068282, 7.362941523434161084 ) ) ;
#50757 = EDGE_CURVE ( 'NONE', #72523, #63848, #50983, .T. ) ;
#50758 = EDGE_LOOP ( 'NONE', ( #11410, #514, #32700, #44764 ) ) ;
#50759 = DIRECTION ( 'NONE',  ( 1.000000000000000000, -0.000000000000000000, -0.000000000000000000 ) ) ;
#50760 = CARTESIAN_POINT ( 'NONE',  ( -28.91304442625643034, -25.26026382785371283, 2.072903053319643529 ) ) ;
#50761 = VECTOR ( 'NONE', #96883, 1000.000000000000000 ) ;
#50762 = CARTESIAN_POINT ( 'NONE',  ( -101.1944152955115044, -25.17353290942304156, 6.858246026101943116 ) ) ;
#50763 = CARTESIAN_POINT ( 'NONE',  ( -4.285004571687458963, -21.18589511591401831, -1.500000000000002220 ) ) ;
#50764 = FACE_OUTER_BOUND ( 'NONE', #1042, .T. ) ;
#50765 = CARTESIAN_POINT ( 'NONE',  ( -70.58953762381671027, -25.00158670708909270, 2.256160236439167299 ) ) ;
#50766 = LINE ( 'NONE', #44146, #20504 ) ;
#50767 = CARTESIAN_POINT ( 'NONE',  ( -80.68529634371549264, -25.04456290340675295, 7.556292259115348742 ) ) ;
#50768 = CARTESIAN_POINT ( 'NONE',  ( -19.57314199983870751, -2.777824058246878280, -1.500000000000002220 ) ) ;
#50769 = ADVANCED_FACE ( 'NONE', ( #93338 ), #9616, .F. ) ;
#50770 = VERTEX_POINT ( 'NONE', #23830 ) ;
#50771 = AXIS2_PLACEMENT_3D ( 'NONE', #715, #31664, #31162 ) ;
#50772 = CARTESIAN_POINT ( 'NONE',  ( 18.82617747125253871, -7.458514806974097411, 11.49999999999999645 ) ) ;
#50773 = CARTESIAN_POINT ( 'NONE',  ( -119.5228709571500474, -24.35013146730203815, 9.818937971375092388 ) ) ;
#50774 = EDGE_CURVE ( 'NONE', #47959, #46913, #81781, .T. ) ;
#50775 = EDGE_CURVE ( 'NONE', #51679, #34175, #1516, .T. ) ;
#50776 = CARTESIAN_POINT ( 'NONE',  ( 6.251785340501501587, -6.376774720514424288, 21.46941214867599612 ) ) ;
#50777 = ORIENTED_EDGE ( 'NONE', *, *, #9109, .T. ) ;
#50778 = CARTESIAN_POINT ( 'NONE',  ( -100.3686882637329063, -25.30212793431289953, 4.712266316240064867 ) ) ;
#50779 = CARTESIAN_POINT ( 'NONE',  ( 33.61456970919605425, 3.316774720514426900, -11.35828564741663449 ) ) ;
#50780 = LINE ( 'NONE', #66027, #32117 ) ;
#50781 = DIRECTION ( 'NONE',  ( 0.000000000000000000, 1.000000000000000000, 0.000000000000000000 ) ) ;
#50782 = FACE_OUTER_BOUND ( 'NONE', #54193, .T. ) ;
#50783 = CARTESIAN_POINT ( 'NONE',  ( 17.67427751897593069, 9.450557017276361549, 11.49999999999998934 ) ) ;
#50784 = CARTESIAN_POINT ( 'NONE',  ( 13.91401389203221406, -5.965225279485572685, 158.0376437107427137 ) ) ;
#50785 = ORIENTED_EDGE ( 'NONE', *, *, #6562, .F. ) ;
#50786 = AXIS2_PLACEMENT_3D ( 'NONE', #36416, #22670, #68865 ) ;
#50787 = CARTESIAN_POINT ( 'NONE',  ( -90.52287095715006160, -23.47596703998600631, 11.44779298504228393 ) ) ;
#50788 = CARTESIAN_POINT ( 'NONE',  ( -104.6228709571500559, -29.50250243563736774, 8.947779886222138046 ) ) ;
#50789 = DIRECTION ( 'NONE',  ( -0.000000000000000000, 1.000000000000000000, -0.000000000000000000 ) ) ;
#50790 = FACE_OUTER_BOUND ( 'NONE', #53219, .T. ) ;
#50791 = ADVANCED_FACE ( 'NONE', ( #48700 ), #32961, .F. ) ;
#50792 = EDGE_CURVE ( 'NONE', #91107, #94475, #33450, .T. ) ;
#50793 = CARTESIAN_POINT ( 'NONE',  ( 14.43441819133292370, 3.316774720514429120, -28.36222020317234183 ) ) ;
#50794 = AXIS2_PLACEMENT_3D ( 'NONE', #46028, #94179, #38899 ) ;
#50795 = FACE_OUTER_BOUND ( 'NONE', #45852, .T. ) ;
#50796 = ORIENTED_EDGE ( 'NONE', *, *, #84088, .F. ) ;
#50797 = CARTESIAN_POINT ( 'NONE',  ( 0.8761431260907562857, 20.31601184897261092, 11.49999999999998934 ) ) ;
#50798 = VECTOR ( 'NONE', #47361, 1000.000000000000114 ) ;
#50799 = ORIENTED_EDGE ( 'NONE', *, *, #79102, .F. ) ;
#50800 = CARTESIAN_POINT ( 'NONE',  ( -20.69623851537618364, -9.862649113751288610, 11.49999999999998934 ) ) ;
#50801 = CARTESIAN_POINT ( 'NONE',  ( 29.68632914399157130, 6.069062472358077720, 27.51067976151145800 ) ) ;
#50803 = ORIENTED_EDGE ( 'NONE', *, *, #4887, .F. ) ;
#50802 = EDGE_CURVE ( 'NONE', #59266, #23124, #25839, .T. ) ;
#50804 = CARTESIAN_POINT ( 'NONE',  ( -37.62287095715005592, -23.47593901973091235, -1.443836447539011525 ) ) ;
#50805 = EDGE_CURVE ( 'NONE', #12406, #91720, #16340, .T. ) ;
#50806 = CARTESIAN_POINT ( 'NONE',  ( -3.108974358974359475, -5.876774720514418071, 20.36458333333334281 ) ) ;
#50807 = DIRECTION ( 'NONE',  ( 1.000000000000000000, 0.000000000000000000, -2.168404344971008868E-16 ) ) ;
#50808 = CARTESIAN_POINT ( 'NONE',  ( 15.74494995282791088, 14.18698661492608615, 11.49999999999999645 ) ) ;
#50809 = CARTESIAN_POINT ( 'NONE',  ( -15.96568504569681402, -15.38390974582250692, -1.500000000000002220 ) ) ;
#50810 = CARTESIAN_POINT ( 'NONE',  ( 20.46650637700042097, -2.330123182410055893, 11.49999999999998934 ) ) ;
#50811 = EDGE_LOOP ( 'NONE', ( #17621, #93968, #30193, #46148 ) ) ;
#50812 = CARTESIAN_POINT ( 'NONE',  ( -41.49888018455134642, -24.15543982623907127, -0.2315651400026566831 ) ) ;
#50813 = ORIENTED_EDGE ( 'NONE', *, *, #12908, .F. ) ;
#50814 = CARTESIAN_POINT ( 'NONE',  ( 6.555906488453394410, -6.376774720514426065, 21.46941147007026274 ) ) ;
#50815 = DIRECTION ( 'NONE',  ( -1.000000000000000000, -3.773278334444166432E-23, -8.201307841325785021E-29 ) ) ;
#50816 = ORIENTED_EDGE ( 'NONE', *, *, #93361, .F. ) ;
#50817 = ORIENTED_EDGE ( 'NONE', *, *, #60434, .T. ) ;
#50818 = ORIENTED_EDGE ( 'NONE', *, *, #67017, .F. ) ;
#50819 = PLANE ( 'NONE',  #21062 ) ;
#50820 = CARTESIAN_POINT ( 'NONE',  ( -28.52390393553966774, -24.49968521371325991, 8.947790409070464079 ) ) ;
#50821 = CARTESIAN_POINT ( 'NONE',  ( 15.88393883468596712, -3.596971506839818034, -28.01277999924163709 ) ) ;
#50822 = CARTESIAN_POINT ( 'NONE',  ( -3.546427018491999483, -20.45703643143680850, -1.500000000000002220 ) ) ;
#50823 = EDGE_CURVE ( 'NONE', #37127, #81082, #43078, .T. ) ;
#50824 = CARTESIAN_POINT ( 'NONE',  ( 6.244050601037331560, 20.82503750550150912, 11.49999999999999645 ) ) ;
#50825 = ORIENTED_EDGE ( 'NONE', *, *, #20226, .F. ) ;
#50826 = VECTOR ( 'NONE', #33986, 1000.000000000000000 ) ;
#50827 = CARTESIAN_POINT ( 'NONE',  ( -10.59832330691884295, -5.965225279485572685, -27.05373799718300987 ) ) ;
#50828 = CARTESIAN_POINT ( 'NONE',  ( -119.6228709571500701, -23.96177878511308634, 10.65340807706329507 ) ) ;
#50829 = CARTESIAN_POINT ( 'NONE',  ( -14.39434090420295220, 17.20869321163716492, -1.500000000000002220 ) ) ;
#50830 = CARTESIAN_POINT ( 'NONE',  ( -83.52287095715006160, -29.50248528299804818, 1.056150453629038477 ) ) ;
#50831 = CARTESIAN_POINT ( 'NONE',  ( -0.1490770655183801252, -21.12008023607309681, -1.443836447538997758 ) ) ;
#50832 = ORIENTED_EDGE ( 'NONE', *, *, #55091, .F. ) ;
#50833 = DIRECTION ( 'NONE',  ( 4.818676322157798854E-17, 0.000000000000000000, 1.000000000000000000 ) ) ;
#50834 = CARTESIAN_POINT ( 'NONE',  ( -97.62287095715005592, -29.50248528299804818, 1.056150453629042030 ) ) ;
#50835 = B_SPLINE_CURVE_WITH_KNOTS ( 'NONE', 3,
 ( #71971, #2452, #64375, #56755 ),
 .UNSPECIFIED., .F., .F.,
 ( 4, 4 ),
 ( 0.000000000000000000, 9.999999999999592548E-05 ),
 .UNSPECIFIED. ) ;
#50836 = AXIS2_PLACEMENT_3D ( 'NONE', #66358, #50120, #65864 ) ;
#50837 = VERTEX_POINT ( 'NONE', #26345 ) ;
#50838 = EDGE_LOOP ( 'NONE', ( #41754, #29327, #20378, #26218 ) ) ;
#50840 = ADVANCED_FACE ( 'NONE', ( #66923 ), #97842, .F. ) ;
#50839 = CARTESIAN_POINT ( 'NONE',  ( -46.53512403956532495, -24.51419770103157347, 9.386484678747180510 ) ) ;
#50841 = ORIENTED_EDGE ( 'NONE', *, *, #33756, .T. ) ;
#50842 = CARTESIAN_POINT ( 'NONE',  ( -16.05942832139214360, -14.02155611864158402, -1.500000000000002220 ) ) ;
#50843 = EDGE_CURVE ( 'NONE', #19111, #36659, #88250, .T. ) ;
#50844 = ORIENTED_EDGE ( 'NONE', *, *, #13917, .F. ) ;
#50845 = CARTESIAN_POINT ( 'NONE',  ( -88.51122574139041888, -24.15543982623907127, -0.2315651400026634277 ) ) ;
#50846 = CARTESIAN_POINT ( 'NONE',  ( 16.32745387341675780, -14.53119815553504068, 11.49999999999998934 ) ) ;
#50847 = DIRECTION ( 'NONE',  ( 0.000000000000000000, 0.000000000000000000, -1.000000000000000000 ) ) ;
#50848 = CARTESIAN_POINT ( 'NONE',  ( -7.973561950239375307, 21.24132968703115765, 11.49999999999998934 ) ) ;
#50849 = CARTESIAN_POINT ( 'NONE',  ( -41.42599659256448774, -25.18431008552816408, 3.925284320572509866 ) ) ;
#50850 = CARTESIAN_POINT ( 'NONE',  ( -24.97666371003640151, 5.965225279485592225, -15.72894043976419098 ) ) ;
#50851 = CARTESIAN_POINT ( 'NONE',  ( 15.37660858059359725, 15.65766701038582021, -1.500000000000002220 ) ) ;
#50852 = CARTESIAN_POINT ( 'NONE',  ( 6.887358010905132666, -5.876774720514425177, 21.32574817943157086 ) ) ;
#50853 = VERTEX_POINT ( 'NONE', #73031 ) ;
#50854 = CARTESIAN_POINT ( 'NONE',  ( -122.5540027605393618, -24.51419770103158413, 9.386484678747169852 ) ) ;
#50855 = LINE ( 'NONE', #4680, #29746 ) ;
#50856 = EDGE_CURVE ( 'NONE', #95392, #47965, #98656, .T. ) ;
#50857 = EDGE_CURVE ( 'NONE', #84112, #91875, #52563, .T. ) ;
#50858 = ORIENTED_EDGE ( 'NONE', *, *, #45751, .F. ) ;
#50859 = CARTESIAN_POINT ( 'NONE',  ( -99.62287095715005592, -23.72773821059535848, 11.05748984161097503 ) ) ;
#50860 = ORIENTED_EDGE ( 'NONE', *, *, #59697, .T. ) ;
#50861 = CARTESIAN_POINT ( 'NONE',  ( 32.45853543194704116, 5.965225279485572685, 9.169203677920338080 ) ) ;
#50862 = CARTESIAN_POINT ( 'NONE',  ( -20.41429444750324862, -24.04291568128049050, 1.633150109380534509 ) ) ;
#50863 = CARTESIAN_POINT ( 'NONE',  ( -20.48789480994130230, 5.740754632170482097, -1.500000000000002220 ) ) ;
#50864 = CARTESIAN_POINT ( 'NONE',  ( -98.54804105917907009, -24.51419770103155926, 9.386484678747176957 ) ) ;
#50865 = CARTESIAN_POINT ( 'NONE',  ( -26.09929425038925999, -24.97064932688204664, 4.716438222426610594 ) ) ;
#50866 = CARTESIAN_POINT ( 'NONE',  ( -85.53826683509211648, -25.00158670708911046, 2.256160236439219702 ) ) ;
#50867 = CARTESIAN_POINT ( 'NONE',  ( -68.49381102065314053, -24.65952944569304606, 1.056160979905701236 ) ) ;
#50868 = VECTOR ( 'NONE', #23798, 1000.000000000000000 ) ;
#50869 = CARTESIAN_POINT ( 'NONE',  ( -117.5924224532624720, -23.73791477778912551, 11.05961554403169878 ) ) ;
#50870 = ORIENTED_EDGE ( 'NONE', *, *, #25508, .T. ) ;
#50871 = CARTESIAN_POINT ( 'NONE',  ( 18.00893756148942870, 7.586210683597776949, 11.49999999999999645 ) ) ;
#50872 = CARTESIAN_POINT ( 'NONE',  ( -67.52287095715006160, -24.66019654487199730, 8.947790411086115725 ) ) ;
#50873 = CIRCLE ( 'NONE', #19916, 2.350000000000000089 ) ;
#50875 = CARTESIAN_POINT ( 'NONE',  ( -116.6228709571500417, -23.48786465467241769, 11.44779295918253759 ) ) ;
#50874 = B_SPLINE_CURVE_WITH_KNOTS ( 'NONE', 3,
 ( #55880, #23900, #62480, #63498 ),
 .UNSPECIFIED., .F., .F.,
 ( 4, 4 ),
 ( 0.000000000000000000, 9.999999999998897304E-05 ),
 .UNSPECIFIED. ) ;
#50876 = EDGE_LOOP ( 'NONE', ( #47820, #35334, #29023, #11512 ) ) ;
#50877 = CARTESIAN_POINT ( 'NONE',  ( 3.960462906497916435, -5.876774720514426953, 21.82884394085917279 ) ) ;
#50878 = CARTESIAN_POINT ( 'NONE',  ( -101.1688285314437223, -25.06333783557038686, 7.418091300476992167 ) ) ;
#50879 = B_SPLINE_CURVE_WITH_KNOTS ( 'NONE', 3,
 ( #91573, #39781, #76340, #70745, #8338, #6840, #37797, #68750, #69747, #77831, #32172, #54522, #99667, #30172, #15941, #8841 ),
 .UNSPECIFIED., .F., .F.,
 ( 4, 2, 2, 2, 2, 2, 2, 4 ),
 ( 0.000000000000000000, 0.0001833998957598680242, 0.0003667997915197360485, 0.0005501996872796041270, 0.0007335995830394720970, 0.001100399374559177029, 0.001283799270319020171, 0.001467199166078863096 ),
 .UNSPECIFIED. ) ;
#50880 = DIRECTION ( 'NONE',  ( 0.9762960071199348056, 0.2164396139380966033, -0.000000000000000000 ) ) ;
#50881 = CARTESIAN_POINT ( 'NONE',  ( -45.62287095715004881, -24.91544648472620338, 1.928969306349229473 ) ) ;
#50882 = EDGE_CURVE ( 'NONE', #64842, #36479, #69558, .T. ) ;
#50883 = CARTESIAN_POINT ( 'NONE',  ( 17.62393913918218402, -8.800128315780904487, 11.49999999999998934 ) ) ;
#50884 = ORIENTED_EDGE ( 'NONE', *, *, #84767, .T. ) ;
#50885 = CARTESIAN_POINT ( 'NONE',  ( 1.437548984227666304, -5.319565594357255733, 0.000000000000000000 ) ) ;
#50886 = FACE_OUTER_BOUND ( 'NONE', #10011, .T. ) ;
#50887 = COORDINATED_UNIVERSAL_TIME_OFFSET ( 0, 0, .AHEAD. ) ;
#50888 = ORIENTED_EDGE ( 'NONE', *, *, #10652, .T. ) ;
#50889 = FACE_OUTER_BOUND ( 'NONE', #82633, .T. ) ;
#50890 = CARTESIAN_POINT ( 'NONE',  ( -121.5228709571500616, -23.47596703998600631, 11.44779298504227860 ) ) ;
#50891 = CARTESIAN_POINT ( 'NONE',  ( -104.9228709571501099, -23.47593901973090880, -1.443836447538997092 ) ) ;
#50892 = CARTESIAN_POINT ( 'NONE',  ( -118.6235039205847386, -24.65952944569305316, 1.056160979905708119 ) ) ;
#50893 = CARTESIAN_POINT ( 'NONE',  ( 5.359050311451609261, -6.376774720514420736, 21.05346524168807676 ) ) ;
#50894 = LINE ( 'NONE', #96554, #92684 ) ;
#50895 = LINE ( 'NONE', #2728, #49494 ) ;
#50896 = CARTESIAN_POINT ( 'NONE',  ( 19.80199147212610811, 2.383747631481649254, -1.500000000000002220 ) ) ;
#50897 = VECTOR ( 'NONE', #83096, 1000.000000000000000 ) ;
#50898 = CARTESIAN_POINT ( 'NONE',  ( -54.52287095715009002, -24.51387760970724372, 9.387446482453405849 ) ) ;
#50899 = CARTESIAN_POINT ( 'NONE',  ( -0.05358151576393885979, -22.35634517190537807, 0.9392753064497983972 ) ) ;
#50900 = ORIENTED_EDGE ( 'NONE', *, *, #82552, .T. ) ;
#50901 = DIRECTION ( 'NONE',  ( -0.000000000000000000, -1.000000000000000000, -0.000000000000000000 ) ) ;
#50902 = CARTESIAN_POINT ( 'NONE',  ( 4.127208352283176396, -5.876774720514423400, 21.39624840817692686 ) ) ;
#50903 = VECTOR ( 'NONE', #43323, 1000.000000000000000 ) ;
#50904 = CARTESIAN_POINT ( 'NONE',  ( 9.196673285530609476, -6.376774720514424288, -25.00509208784493964 ) ) ;
#50905 = CARTESIAN_POINT ( 'NONE',  ( -122.6228709571500701, -23.48783264082479505, -1.443836473390058828 ) ) ;
#50906 = CARTESIAN_POINT ( 'NONE',  ( -7.243541020599075786, -6.376774720514408301, 19.27798293355755632 ) ) ;
#50907 = CARTESIAN_POINT ( 'NONE',  ( -74.62287095715005592, -23.47593901973091235, -1.443836447539006196 ) ) ;
#50908 = CARTESIAN_POINT ( 'NONE',  ( -50.66424699104888418, -25.18847548320762186, 3.319059850524417765 ) ) ;
#50910 = ADVANCED_FACE ( 'NONE', ( #26844 ), #19222, .F. ) ;
#50909 = ORIENTED_EDGE ( 'NONE', *, *, #98392, .F. ) ;
#50911 = DIRECTION ( 'NONE',  ( 0.000000000000000000, 0.000000000000000000, 1.000000000000000000 ) ) ;
#50912 = FACE_OUTER_BOUND ( 'NONE', #81665, .T. ) ;
#50913 = VERTEX_POINT ( 'NONE', #89244 ) ;
#50914 = CARTESIAN_POINT ( 'NONE',  ( 17.32893120472914816, 10.46255702124672027, 11.49999999999998934 ) ) ;
#50915 = FACE_OUTER_BOUND ( 'NONE', #53109, .T. ) ;
#50916 = B_SPLINE_CURVE_WITH_KNOTS ( 'NONE', 3,
 ( #37641, #70097, #30019, #61492, #16804, #69601, #577, #100011, #70595, #82, #8199, #91923, #39137, #46256 ),
 .UNSPECIFIED., .F., .F.,
 ( 4, 2, 2, 2, 2, 2, 4 ),
 ( 0.000000000000000000, 0.0001851154269384487790, 0.0003702308538768975580, 0.0007404617077537563015, 0.001110692561630614991, 0.001295807988569044064, 0.001480923415507472921 ),
 .UNSPECIFIED. ) ;
#50917 = CARTESIAN_POINT ( 'NONE',  ( 5.184553252003285984, 5.965225279485572685, -28.06387035751381731 ) ) ;
#50918 = EDGE_CURVE ( 'NONE', #98447, #89470, #15093, .T. ) ;
#50919 = ADVANCED_FACE ( 'NONE', ( #81128 ), #11609, .T. ) ;
#50920 = DIRECTION ( 'NONE',  ( 0.000000000000000000, -1.000000000000000000, 0.000000000000000000 ) ) ;
#50921 = SHAPE_REPRESENTATION ( 'Spring-loaded Plate_Varsay\X2\0131\X0\lan', ( #37391 ), #27759 ) ;
#50922 = ADVANCED_FACE ( 'NONE', ( #50686 ), #35463, .T. ) ;
#50923 = VERTEX_POINT ( 'NONE', #89746 ) ;
#50924 = CARTESIAN_POINT ( 'NONE',  ( 6.499999999999992895, -1.874386984050377894E-16, 2.100000000000000977 ) ) ;
#50925 = CARTESIAN_POINT ( 'NONE',  ( -52.52287095715008292, -24.66019654487198665, 8.947790411086131712 ) ) ;
#50926 = CARTESIAN_POINT ( 'NONE',  ( -2.827821146493835425, 19.88259668395040691, -1.500000000000002220 ) ) ;
#50927 = CARTESIAN_POINT ( 'NONE',  ( -15.31302551872622075, -14.39686070098267479, 11.49999999999999645 ) ) ;
#50928 = EDGE_CURVE ( 'NONE', #60977, #32935, #97355, .T. ) ;
#50929 = CARTESIAN_POINT ( 'NONE',  ( -28.54571666164230948, -24.94250516244451532, 7.283072174430436974 ) ) ;
#50930 = CARTESIAN_POINT ( 'NONE',  ( -89.81226385320381667, -25.26877915520014994, 5.947789088310639904 ) ) ;
#50931 = CARTESIAN_POINT ( 'NONE',  ( -21.12782282263547984, 6.412464199276892707, -1.500000000000002220 ) ) ;
#50932 = CARTESIAN_POINT ( 'NONE',  ( -42.52287095715005449, -24.64898659630367206, 1.056161002820819261 ) ) ;
#50933 = CARTESIAN_POINT ( 'NONE',  ( -55.62287095715004170, -24.99132157543083821, 2.256160258750667502 ) ) ;
#50934 = CARTESIAN_POINT ( 'NONE',  ( -50.10737344585005815, -25.27344765917630554, 3.323112495376625564 ) ) ;
#50935 = ORIENTED_EDGE ( 'NONE', *, *, #47715, .T. ) ;
#50936 = CARTESIAN_POINT ( 'NONE',  ( -100.4381051993576364, -25.12049752546738191, 2.832404795212222215 ) ) ;
#50937 = B_SPLINE_SURFACE_WITH_KNOTS ( 'NONE', 3, 3, ( 
 ( #93274, #55245, #86171, #94781 ),
 ( #32894, #54241, #15656, #63868 ),
 ( #63364, #70455, #23764, #53739 ),
 ( #77545, #62865, #16154, #38994 ),
 ( #17159, #94279, #61853, #47626 ),
 ( #54740, #433, #24762, #62349 ),
 ( #30886, #71463, #85674, #55745 ) ),
 .UNSPECIFIED., .F., .F., .F.,
 ( 4, 3, 4 ),
 ( 4, 4 ),
 ( 0.0004766839783822873398, 0.1029713700210899419, 0.2054660560637975864 ),
 ( 0.03950404640253154381, 0.04053499805299270314 ),
 .UNSPECIFIED. ) ;
#50938 = CARTESIAN_POINT ( 'NONE',  ( 1.351731822651893733, -3.882286141751411179, 8.999999999999994671 ) ) ;
#50939 = ORIENTED_EDGE ( 'NONE', *, *, #4885, .F. ) ;
#50940 = ORIENTED_EDGE ( 'NONE', *, *, #55206, .T. ) ;
#50941 = CARTESIAN_POINT ( 'NONE',  ( -55.52287095715005449, -25.00158670708909270, 2.256160236439166411 ) ) ;
#50942 = CARTESIAN_POINT ( 'NONE',  ( 19.24418710706453339, -0.5000000000000000000, 2.346898003627108320 ) ) ;
#50943 = CARTESIAN_POINT ( 'NONE',  ( -62.52287095715006160, -23.47593901973090169, -1.443836447538997092 ) ) ;
#50944 = CARTESIAN_POINT ( 'NONE',  ( 9.149160795417088821, -18.46424698110740437, -1.500000000000002220 ) ) ;
#50945 = EDGE_CURVE ( 'NONE', #88122, #31070, #20215, .T. ) ;
#50946 = CARTESIAN_POINT ( 'NONE',  ( -20.54356019850136050, 6.435454313062578535, 11.49999999999999645 ) ) ;
#50947 = ORIENTED_EDGE ( 'NONE', *, *, #49409, .T. ) ;
#50948 = CARTESIAN_POINT ( 'NONE',  ( -49.28469068309977530, -25.24826530213481846, 6.282384552296719882 ) ) ;
#50949 = DIRECTION ( 'NONE',  ( -3.773278334453079618E-23, 0.9999999999976377785, 2.173523156925979975E-06 ) ) ;
#50950 = CARTESIAN_POINT ( 'NONE',  ( -4.286263797015736595E-16, -2.056774720514426669, -3.500000000000000000 ) ) ;
#50951 = CARTESIAN_POINT ( 'NONE',  ( 22.01400519847025450, -3.885951517071169370, 11.49999999999998934 ) ) ;
#50952 = CARTESIAN_POINT ( 'NONE',  ( -59.62287095715004170, -24.35013146730203815, 9.818937971375111928 ) ) ;
#50953 = FACE_OUTER_BOUND ( 'NONE', #58046, .T. ) ;
#50954 = EDGE_CURVE ( 'NONE', #76857, #7414, #84103, .T. ) ;
#50955 = ORIENTED_EDGE ( 'NONE', *, *, #43196, .T. ) ;
#50956 = LINE ( 'NONE', #6258, #72823 ) ;
#50957 = CARTESIAN_POINT ( 'NONE',  ( -51.70072539166533687, -25.26311289191998455, 3.987152081390995306 ) ) ;
#50958 = B_SPLINE_CURVE_WITH_KNOTS ( 'NONE', 3,
 ( #92555, #15928, #46895, #8325, #17436, #3240, #88459, #16935, #2231, #34173, #57522, #95066, #48398, #25043 ),
 .UNSPECIFIED., .F., .F.,
 ( 4, 2, 2, 2, 2, 2, 4 ),
 ( 0.000000000000000000, 0.0003092239551898974103, 0.0004638359327848582585, 0.0006184479103798191067, 0.0009276718655697721366, 0.001082283843164748380, 0.001236895820759724733 ),
 .UNSPECIFIED. ) ;
#50959 = CARTESIAN_POINT ( 'NONE',  ( 8.468106961216914641, 19.09613275528424836, -1.500000000000002220 ) ) ;
#50960 = ORIENTED_EDGE ( 'NONE', *, *, #4885, .T. ) ;
#50961 = VECTOR ( 'NONE', #19309, 1000.000000000000114 ) ;
#50964 = ORIENTED_EDGE ( 'NONE', *, *, #96079, .T. ) ;
#50963 = EDGE_CURVE ( 'NONE', #84227, #13356, #58781, .T. ) ;
#50962 = DIRECTION ( 'NONE',  ( 0.7071067811865474617, -0.000000000000000000, 0.7071067811865474617 ) ) ;
#50965 = VERTEX_POINT ( 'NONE', #95853 ) ;
#50966 = CARTESIAN_POINT ( 'NONE',  ( -100.6334151984021759, -24.15602025860896518, 10.28564288303536856 ) ) ;
#50967 = CARTESIAN_POINT ( 'NONE',  ( -18.40674794014382698, -10.35651468716735657, -1.500000000000002220 ) ) ;
#50968 = ORIENTED_EDGE ( 'NONE', *, *, #5798, .F. ) ;
#50969 = CARTESIAN_POINT ( 'NONE',  ( -85.62287095715002749, -25.00182538069145011, 7.747789668545099317 ) ) ;
#50970 = PLANE ( 'NONE',  #46648 ) ;
#50971 = DIRECTION ( 'NONE',  ( -0.000000000000000000, -0.000000000000000000, 1.000000000000000000 ) ) ;
#50972 = DIRECTION ( 'NONE',  ( -3.491481338843133355E-15, 1.000000000000000000, -2.352173255807804438E-16 ) ) ;
#50973 = CARTESIAN_POINT ( 'NONE',  ( 7.190659024148910561, -6.376774720514413630, 19.91543959911579620 ) ) ;
#50974 = CARTESIAN_POINT ( 'NONE',  ( -20.31635052000798325, -7.690577546848336610, -1.500000000000002220 ) ) ;
#50975 = CARTESIAN_POINT ( 'NONE',  ( -81.04964064216432007, -25.12224358380520783, 6.946763632574976199 ) ) ;
#50977 = EDGE_LOOP ( 'NONE', ( #54084, #27954, #94616, #38428 ) ) ;
#50976 = CARTESIAN_POINT ( 'NONE',  ( -11.95080204275630464, 18.75100984808165094, 11.49999999999999645 ) ) ;
#50978 = FACE_OUTER_BOUND ( 'NONE', #33107, .T. ) ;
#50979 = LINE ( 'NONE', #42871, #63818 ) ;
#50980 = FACE_OUTER_BOUND ( 'NONE', #64088, .T. ) ;
#50982 = ORIENTED_EDGE ( 'NONE', *, *, #17827, .F. ) ;
#50981 = EDGE_CURVE ( 'NONE', #88881, #57483, #83618, .T. ) ;
#50983 = CIRCLE ( 'NONE', #62345, 1.306876713926001354 ) ;
#50984 = EDGE_CURVE ( 'NONE', #6550, #39939, #61120, .T. ) ;
#50986 = VERTEX_POINT ( 'NONE', #30837 ) ;
#50985 = CARTESIAN_POINT ( 'NONE',  ( -40.62287095715004170, -25.00158670708908204, 2.256160236439166411 ) ) ;
#50987 = ORIENTED_EDGE ( 'NONE', *, *, #16004, .F. ) ;
#50988 = CARTESIAN_POINT ( 'NONE',  ( -101.1944152955115186, -25.17323144036708626, 6.858246026757193192 ) ) ;
#50989 = LINE ( 'NONE', #94268, #61181 ) ;
#50990 = FACE_OUTER_BOUND ( 'NONE', #53224, .T. ) ;
#50991 = CARTESIAN_POINT ( 'NONE',  ( -37.62287095715005592, -24.66019654487199020, 8.947790411086135265 ) ) ;
#50992 = CARTESIAN_POINT ( 'NONE',  ( -66.52287095715010423, -23.72773821059536914, 11.05748984161097326 ) ) ;
#50993 = VERTEX_POINT ( 'NONE', #29335 ) ;
#50994 = CARTESIAN_POINT ( 'NONE',  ( -13.43510958081001050, -13.94331287200543024, 11.49999999999999645 ) ) ;
#50995 = CARTESIAN_POINT ( 'NONE',  ( -69.52287095715006160, -23.47593901973090169, -1.443836447538996870 ) ) ;
#50996 = CARTESIAN_POINT ( 'NONE',  ( -17.93832129671990572, 13.47109510200611560, -1.500000000000002220 ) ) ;
#50997 = ORIENTED_EDGE ( 'NONE', *, *, #78839, .T. ) ;
#50998 = DIRECTION ( 'NONE',  ( 0.000000000000000000, -1.000000000000000000, 0.000000000000000000 ) ) ;
#50999 = DIRECTION ( 'NONE',  ( -3.773278334453079030E-23, 0.9999999999976377785, 2.173523156925979128E-06 ) ) ;
#51000 = DIRECTION ( 'NONE',  ( 0.000000000000000000, -1.000000000000000000, 0.000000000000000000 ) ) ;
#51001 = CARTESIAN_POINT ( 'NONE',  ( -63.92776651206412453, -24.47917135695840685, 9.440663514584127114 ) ) ;
#51002 = CARTESIAN_POINT ( 'NONE',  ( 16.73968668634701729, 10.17700309559984717, -1.500000000000002220 ) ) ;
#51003 = CARTESIAN_POINT ( 'NONE',  ( -46.48849370679067761, -24.51314013834315020, 0.6176544820404062941 ) ) ;
#51004 = VERTEX_POINT ( 'NONE', #61802 ) ;
#51005 = CIRCLE ( 'NONE', #72088, 28.96799999999999642 ) ;
#51006 = CARTESIAN_POINT ( 'NONE',  ( -20.49900048275977227, -6.559984590058941301, 11.49999999999998934 ) ) ;
#51007 = CARTESIAN_POINT ( 'NONE',  ( -121.5228709571501042, -23.48783264082477018, -1.443836473390083253 ) ) ;
#51008 = CARTESIAN_POINT ( 'NONE',  ( -71.28784841027113828, -25.25639446183122772, 6.387102990573659156 ) ) ;
#51009 = DIRECTION ( 'NONE',  ( -3.773278334453080206E-23, 0.9999999999976377785, 2.173523156925979975E-06 ) ) ;
#51010 = CARTESIAN_POINT ( 'NONE',  ( -99.52818128268205555, -25.27473369906244471, 3.976272290400146847 ) ) ;
#51011 = CARTESIAN_POINT ( 'NONE',  ( 8.986065527603487979, -21.13286776747340667, -1.500000000000002220 ) ) ;
#51012 = DATE_AND_TIME ( #6320, #48989 ) ;
#51013 = CARTESIAN_POINT ( 'NONE',  ( -61.62287095715004881, -29.50250243563736774, 8.947779886222145151 ) ) ;
#51014 = CARTESIAN_POINT ( 'NONE',  ( 8.499999999999989342, 18.74999999999999645, 0.000000000000000000 ) ) ;
#51015 = CARTESIAN_POINT ( 'NONE',  ( -15.35229381799144299, -13.07563953244551591, 11.49999999999999645 ) ) ;
#51016 = CARTESIAN_POINT ( 'NONE',  ( -109.1001591083545179, -25.28814224509513053, 3.548368719171229646 ) ) ;
#51017 = CARTESIAN_POINT ( 'NONE',  ( -32.62373933420111882, -24.66019654487198665, 8.947790411086131712 ) ) ;
#51018 = DIRECTION ( 'NONE',  ( -3.773278334444167608E-23, 1.000000000000000000, 0.000000000000000000 ) ) ;
#51019 = CARTESIAN_POINT ( 'NONE',  ( -0.02075734969026423599, 5.866774720514426278, -0.08597719988137648983 ) ) ;
#51020 = CARTESIAN_POINT ( 'NONE',  ( -82.52287095715004739, -23.95044443724992789, 10.65354141964649592 ) ) ;
#51021 = CARTESIAN_POINT ( 'NONE',  ( -12.84220538718065185, 15.17226672225704398, -1.500000000000002220 ) ) ;
#51022 = PLANE ( 'NONE',  #73903 ) ;
#51023 = CARTESIAN_POINT ( 'NONE',  ( 14.14096853472169535, -13.71769858867784464, -1.500000000000002220 ) ) ;
#51024 = CARTESIAN_POINT ( 'NONE',  ( -42.63429243087625764, -24.34968618360933590, 0.1864209137778841396 ) ) ;
#51025 = DIRECTION ( 'NONE',  ( 0.000000000000000000, 0.000000000000000000, 1.000000000000000000 ) ) ;
#51026 = DIRECTION ( 'NONE',  ( -1.000000000000000000, -0.000000000000000000, -0.000000000000000000 ) ) ;
#51027 = CARTESIAN_POINT ( 'NONE',  ( -9.157874670058189892, -18.46812626297970539, 11.49999999999999645 ) ) ;
#51028 = CARTESIAN_POINT ( 'NONE',  ( -39.31539998891226162, -25.31628649467095116, 5.139621149922747989 ) ) ;
#51029 = B_SPLINE_CURVE_WITH_KNOTS ( 'NONE', 3,
 ( #62734, #76421, #15527, #61731 ),
 .UNSPECIFIED., .F., .F.,
 ( 4, 4 ),
 ( 0.000000000000000000, 0.001096191829319139886 ),
 .UNSPECIFIED. ) ;
#51030 = VECTOR ( 'NONE', #51400, 1000.000000000000000 ) ;
#51031 = FACE_OUTER_BOUND ( 'NONE', #81297, .T. ) ;
#51032 = CARTESIAN_POINT ( 'NONE',  ( -19.66899025692886838, 11.29834648773183581, 11.49999999999999645 ) ) ;
#51033 = ORIENTED_EDGE ( 'NONE', *, *, #69613, .T. ) ;
#51034 = CARTESIAN_POINT ( 'NONE',  ( -86.52287095715001897, -23.73907113217710929, -1.053371485780543848 ) ) ;
#51036 = EDGE_CURVE ( 'NONE', #23353, #51831, #49096, .T. ) ;
#51035 = CARTESIAN_POINT ( 'NONE',  ( 30.62555539057593634, 4.734697315945937568, 27.74929510164747981 ) ) ;
#51037 = EDGE_CURVE ( 'NONE', #60506, #89004, #3085, .T. ) ;
#51038 = FACE_BOUND ( 'NONE', #36717, .T. ) ;
#51039 = VECTOR ( 'NONE', #40594, 1000.000000000000114 ) ;
#51040 = ADVANCED_FACE ( 'NONE', ( #98337 ), #38661, .T. ) ;
#51041 = CARTESIAN_POINT ( 'NONE',  ( -56.52287095715006870, -24.51387760970724372, 9.387446482453409402 ) ) ;
#51042 = EDGE_CURVE ( 'NONE', #89130, #89740, #55831, .T. ) ;
#51043 = ORIENTED_EDGE ( 'NONE', *, *, #40871, .F. ) ;
#51044 = EDGE_CURVE ( 'NONE', #38058, #5126, #52662, .T. ) ;
#51045 = ORIENTED_EDGE ( 'NONE', *, *, #66774, .F. ) ;
#51046 = CARTESIAN_POINT ( 'NONE',  ( -99.33852787251029781, -25.22239172282626285, 6.423926351378344890 ) ) ;
#51047 = CARTESIAN_POINT ( 'NONE',  ( -9.520747347383798243, -20.79447232172871907, -1.500000000000002220 ) ) ;
#51048 = CARTESIAN_POINT ( 'NONE',  ( -52.62287095715005592, -29.50250243563736774, 8.947779886222146928 ) ) ;
#51049 = CARTESIAN_POINT ( 'NONE',  ( 14.26105141482337935, -16.23293960606763520, -1.500000000000002220 ) ) ;
#51050 = CARTESIAN_POINT ( 'NONE',  ( -113.5154120510410536, -24.51419770103157347, 9.386484678747168076 ) ) ;
#51051 = CARTESIAN_POINT ( 'NONE',  ( -115.5228709571500616, -24.99156044556202616, 7.747789690856173195 ) ) ;
#51052 = CARTESIAN_POINT ( 'NONE',  ( 20.50669422456317292, -9.396423750077818937, 11.49999999999999645 ) ) ;
#51053 = ORIENTED_EDGE ( 'NONE', *, *, #37873, .F. ) ;
#51054 = CARTESIAN_POINT ( 'NONE',  ( -68.62287095715005592, -24.64965695001468404, 8.947790433994184056 ) ) ;
#51055 = CARTESIAN_POINT ( 'NONE',  ( 21.11370014442628218, -6.196533921283487345, -1.500000000000002220 ) ) ;
#51056 = CARTESIAN_POINT ( 'NONE',  ( -64.52287095715006160, -24.64898659630528854, 1.056161002820822592 ) ) ;
#51057 = CARTESIAN_POINT ( 'NONE',  ( -112.5895376238167387, -24.64965694238407679, 8.947790433994649462 ) ) ;
#51058 = EDGE_LOOP ( 'NONE', ( #64312, #64290, #68206, #30616 ) ) ;
#51059 = LINE ( 'NONE', #89119, #86454 ) ;
#51060 = CARTESIAN_POINT ( 'NONE',  ( -0.3544984435505275644, -5.876774720514408301, 19.15251819062245531 ) ) ;
#51061 = ORIENTED_EDGE ( 'NONE', *, *, #9781, .T. ) ;
#51062 = CARTESIAN_POINT ( 'NONE',  ( -76.52287095715007581, -29.50250243563736774, 8.947779886222141599 ) ) ;
#51063 = ORIENTED_EDGE ( 'NONE', *, *, #43196, .F. ) ;
#51064 = ORIENTED_EDGE ( 'NONE', *, *, #33291, .F. ) ;
#51065 = ORIENTED_EDGE ( 'NONE', *, *, #81234, .T. ) ;
#51066 = DIRECTION ( 'NONE',  ( 0.000000000000000000, 0.000000000000000000, -1.000000000000000000 ) ) ;
#51067 = CARTESIAN_POINT ( 'NONE',  ( -100.4381051993576506, -25.11033443737754212, 2.832404817301930056 ) ) ;
#51068 = DIRECTION ( 'NONE',  ( 0.000000000000000000, 0.000000000000000000, 1.000000000000000000 ) ) ;
#51069 = CARTESIAN_POINT ( 'NONE',  ( 19.80222353126469415, -4.898785079568316547, -1.500000000000002220 ) ) ;
#51070 = EDGE_LOOP ( 'NONE', ( #62192, #76174, #50343, #49764 ) ) ;
#51071 = DIRECTION ( 'NONE',  ( -1.955152872784845154E-15, -1.000000000000000000, 3.740001113483016365E-15 ) ) ;
#51072 = CARTESIAN_POINT ( 'NONE',  ( -51.01463207101524944, -25.14354145956054509, 2.962925292413864486 ) ) ;
#51073 = CARTESIAN_POINT ( 'NONE',  ( -97.52287095715007581, -23.47593901973090524, -1.443836447538996648 ) ) ;
#51074 = CARTESIAN_POINT ( 'NONE',  ( -71.70128661679227378, -25.25855123413748871, 6.373708393512837134 ) ) ;
#51075 = ADVANCED_FACE ( 'NONE', ( #25220 ), #71918, .T. ) ;
#51076 = ORIENTED_EDGE ( 'NONE', *, *, #57246, .F. ) ;
#51077 = LINE ( 'NONE', #82018, #27399 ) ;
#51078 = CARTESIAN_POINT ( 'NONE',  ( -94.52287095715007581, -23.47593901973090524, -1.443836447538996648 ) ) ;
#51079 = AXIS2_PLACEMENT_3D ( 'NONE', #85317, #93936, #76692 ) ;
#51080 = ORIENTED_EDGE ( 'NONE', *, *, #55390, .F. ) ;
#51081 = CARTESIAN_POINT ( 'NONE',  ( -3.546427018491999483, -20.45703643143680850, -1.500000000000002220 ) ) ;
#51082 = ORIENTED_EDGE ( 'NONE', *, *, #43593, .F. ) ;
#51084 = ORIENTED_EDGE ( 'NONE', *, *, #89843, .T. ) ;
#51083 = CARTESIAN_POINT ( 'NONE',  ( -29.49875734969026198, -0.3587747205144265483, 10.11402280011862587 ) ) ;
#51085 = DIRECTION ( 'NONE',  ( -3.773278334453079618E-23, 0.9999999999976377785, 2.173523156925979975E-06 ) ) ;
#51086 = CARTESIAN_POINT ( 'NONE',  ( -129.5556839989185960, -24.66019654487200086, 8.947790411086113949 ) ) ;
#51087 = EDGE_LOOP ( 'NONE', ( #9082, #31836, #1610, #26223 ) ) ;
#51088 = ORIENTED_EDGE ( 'NONE', *, *, #60363, .F. ) ;
#51089 = CARTESIAN_POINT ( 'NONE',  ( 3.180076745125953508, -0.3587747205143968499, -28.87659520466658236 ) ) ;
#51090 = CARTESIAN_POINT ( 'NONE',  ( -117.2170248000532951, -25.23482019547913424, 3.690485340690507154 ) ) ;
#51091 = CARTESIAN_POINT ( 'NONE',  ( -4.537657931416015700, -5.876774720514410077, 19.25713806424188235 ) ) ;
#51092 = CARTESIAN_POINT ( 'NONE',  ( -43.54650061354490020, -24.15620529776627734, 10.23563542870661003 ) ) ;
#51094 = ORIENTED_EDGE ( 'NONE', *, *, #72694, .F. ) ;
#51093 = CARTESIAN_POINT ( 'NONE',  ( 17.21905055353458991, -13.78536315820828229, 11.49999999999999645 ) ) ;
#51095 = CARTESIAN_POINT ( 'NONE',  ( -119.6228709571500559, -29.50247984919015209, -1.443849546365046699 ) ) ;
#51096 = CARTESIAN_POINT ( 'NONE',  ( -17.13258802378025791, -14.77425600068537115, -1.500000000000002220 ) ) ;
#51097 = ADVANCED_FACE ( 'NONE', ( #7997 ), #17109, .T. ) ;
#51099 = ORIENTED_EDGE ( 'NONE', *, *, #88271, .F. ) ;
#51098 = CARTESIAN_POINT ( 'NONE',  ( -115.5522222404271560, -24.63419186844613051, 9.035850630976920428 ) ) ;
#51100 = ORIENTED_EDGE ( 'NONE', *, *, #51559, .F. ) ;
#51101 = DIRECTION ( 'NONE',  ( -0.000000000000000000, -1.000000000000000000, -0.000000000000000000 ) ) ;
#51102 = ADVANCED_FACE ( 'NONE', ( #93727 ), #2402, .T. ) ;
#51103 = AXIS2_PLACEMENT_3D ( 'NONE', #29318, #60290, #91213 ) ;
#51104 = CARTESIAN_POINT ( 'NONE',  ( -57.63796015616722457, -24.15620529776628089, 10.23563542870660470 ) ) ;
#51105 = ORIENTED_EDGE ( 'NONE', *, *, #487, .F. ) ;
#51106 = CARTESIAN_POINT ( 'NONE',  ( -20.37118330240554087, -5.769015352940915164, 11.49999999999998934 ) ) ;
#51107 = CARTESIAN_POINT ( 'NONE',  ( -89.52287095715004739, -24.51387760970726148, 9.387446482453416507 ) ) ;
#51108 = CARTESIAN_POINT ( 'NONE',  ( 10.43072250204971851, -19.66636941823637841, -1.500000000000002220 ) ) ;
#51109 = DIRECTION ( 'NONE',  ( -0.000000000000000000, 1.000000000000000000, -0.000000000000000000 ) ) ;
#51110 = VECTOR ( 'NONE', #78763, 1000.000000000000114 ) ;
#51111 = ORIENTED_EDGE ( 'NONE', *, *, #62509, .T. ) ;
#51112 = CARTESIAN_POINT ( 'NONE',  ( -0.1426030150137709562, -21.20389190742572083, 11.50200000000000422 ) ) ;
#51113 = CARTESIAN_POINT ( 'NONE',  ( -37.58096006492539942, -24.51314013834315375, 0.6176544820404124003 ) ) ;
#51114 = VECTOR ( 'NONE', #56560, 1000.000000000000000 ) ;
#51115 = CARTESIAN_POINT ( 'NONE',  ( -79.62287095715004170, -23.47596703998600631, 11.44779298504227860 ) ) ;
#51116 = LINE ( 'NONE', #26778, #22638 ) ;
#51117 = CARTESIAN_POINT ( 'NONE',  ( 16.96702763494397104, -9.608290155750392358, -1.500000000000002220 ) ) ;
#51118 = CARTESIAN_POINT ( 'NONE',  ( 5.397486108853063236, 20.74927772461418485, -1.500000000000002220 ) ) ;
#51119 = CARTESIAN_POINT ( 'NONE',  ( -26.85447117215736412, -24.92774709175325043, 1.825771349380765907 ) ) ;
#51120 = CARTESIAN_POINT ( 'NONE',  ( 30.93860345374796594, 0.6647747205144264315, 20.86760796525322093 ) ) ;
#51121 = CARTESIAN_POINT ( 'NONE',  ( -34.52287095715005449, -23.72747288104469732, -1.053458166803228346 ) ) ;
#51122 = CARTESIAN_POINT ( 'NONE',  ( 4.306090731860143350, 22.38281141545218844, -1.500000000000002220 ) ) ;
#51123 = APPROVAL_ROLE ( '' ) ;
#51124 = CARTESIAN_POINT ( 'NONE',  ( -79.52287095715010423, -23.47593901973090524, -1.443836447538996870 ) ) ;
#51125 = DIRECTION ( 'NONE',  ( -3.773278334453079030E-23, 0.9999999999976377785, 2.173523156925979128E-06 ) ) ;
#51126 = CARTESIAN_POINT ( 'NONE',  ( 12.47747183659840786, 15.48776231947736015, 11.49999999999999645 ) ) ;
#51127 = DIRECTION ( 'NONE',  ( -0.000000000000000000, -1.000000000000000000, -0.000000000000000000 ) ) ;
#51128 = CARTESIAN_POINT ( 'NONE',  ( -71.52287095715007581, -24.64965694238408034, 8.947790433994200043 ) ) ;
#51129 = LINE ( 'NONE', #82568, #73149 ) ;
#51130 = ORIENTED_EDGE ( 'NONE', *, *, #91023, .T. ) ;
#51131 = DIRECTION ( 'NONE',  ( 0.000000000000000000, 0.000000000000000000, 1.000000000000000000 ) ) ;
#51132 = CARTESIAN_POINT ( 'NONE',  ( 0.000000000000000000, -2.056774720514426669, 3.500000000000000000 ) ) ;
#51133 = CARTESIAN_POINT ( 'NONE',  ( 5.343276940429747768, -21.04383479052346217, -1.500000000000002220 ) ) ;
#51134 = CARTESIAN_POINT ( 'NONE',  ( -94.52287095715006160, -24.64898659630367916, 1.056161002820827921 ) ) ;
#51135 = CARTESIAN_POINT ( 'NONE',  ( 17.37147561666312257, 8.948746033654231269, -1.500000000000002220 ) ) ;
#51136 = LINE ( 'NONE', #20673, #8566 ) ;
#51137 = ORIENTED_EDGE ( 'NONE', *, *, #1952, .F. ) ;
#51138 = APPROVAL_ROLE ( '' ) ;
#51139 = VECTOR ( 'NONE', #81355, 1000.000000000000114 ) ;
#51141 = CARTESIAN_POINT ( 'NONE',  ( -60.62287095715007723, -24.52323809116982645, 9.355190652339427260 ) ) ;
#51140 = B_SPLINE_CURVE_WITH_KNOTS ( 'NONE', 3,
 ( #48945, #41840, #16467, #3280 ),
 .UNSPECIFIED., .F., .F.,
 ( 4, 4 ),
 ( 0.007875538328797549587, 0.009214210883376282302 ),
 .UNSPECIFIED. ) ;
#51142 = CARTESIAN_POINT ( 'NONE',  ( 16.92567061652012228, 11.46397006495115534, 11.49999999999999645 ) ) ;
#51143 = LINE ( 'NONE', #73984, #44123 ) ;
#51144 = CARTESIAN_POINT ( 'NONE',  ( -39.62287095715004881, -24.50321055353805022, 9.387540953477534700 ) ) ;
#51145 = EDGE_LOOP ( 'NONE', ( #26375, #11861, #95203, #15942 ) ) ;
#51146 = CARTESIAN_POINT ( 'NONE',  ( -62.62287095715009144, -23.96127896941632685, -0.6493128931037860374 ) ) ;
#51147 = CARTESIAN_POINT ( 'NONE',  ( -106.6228709571500275, -24.33927499327855060, 9.819080762295810061 ) ) ;
